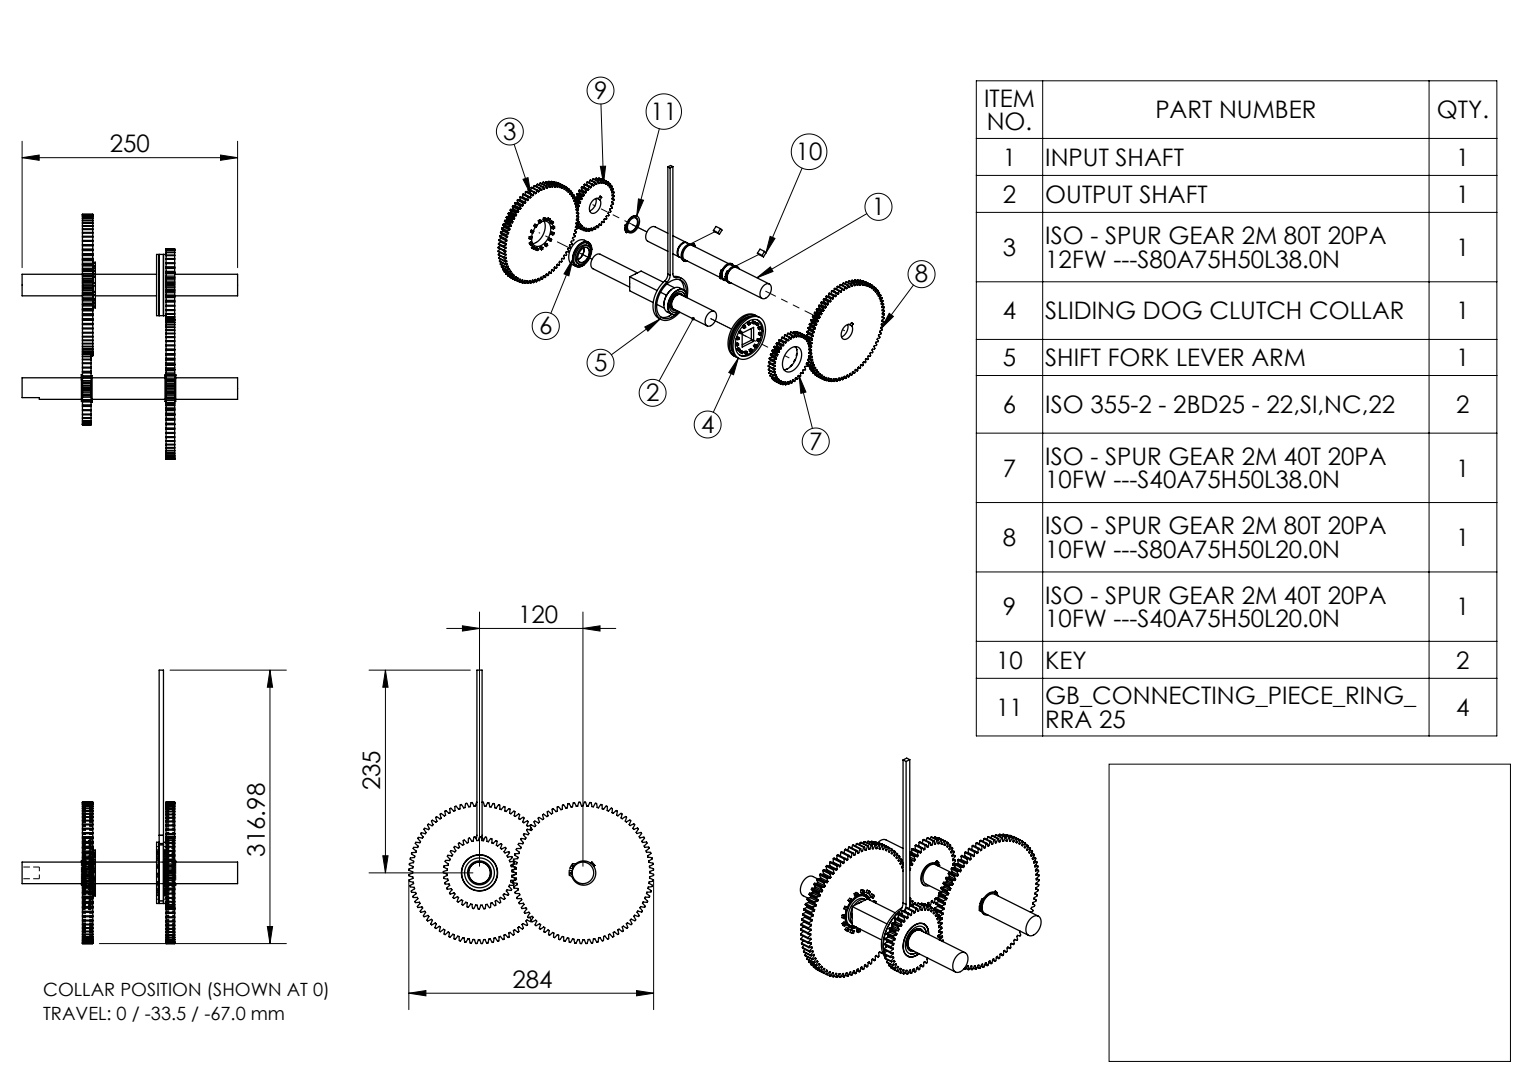
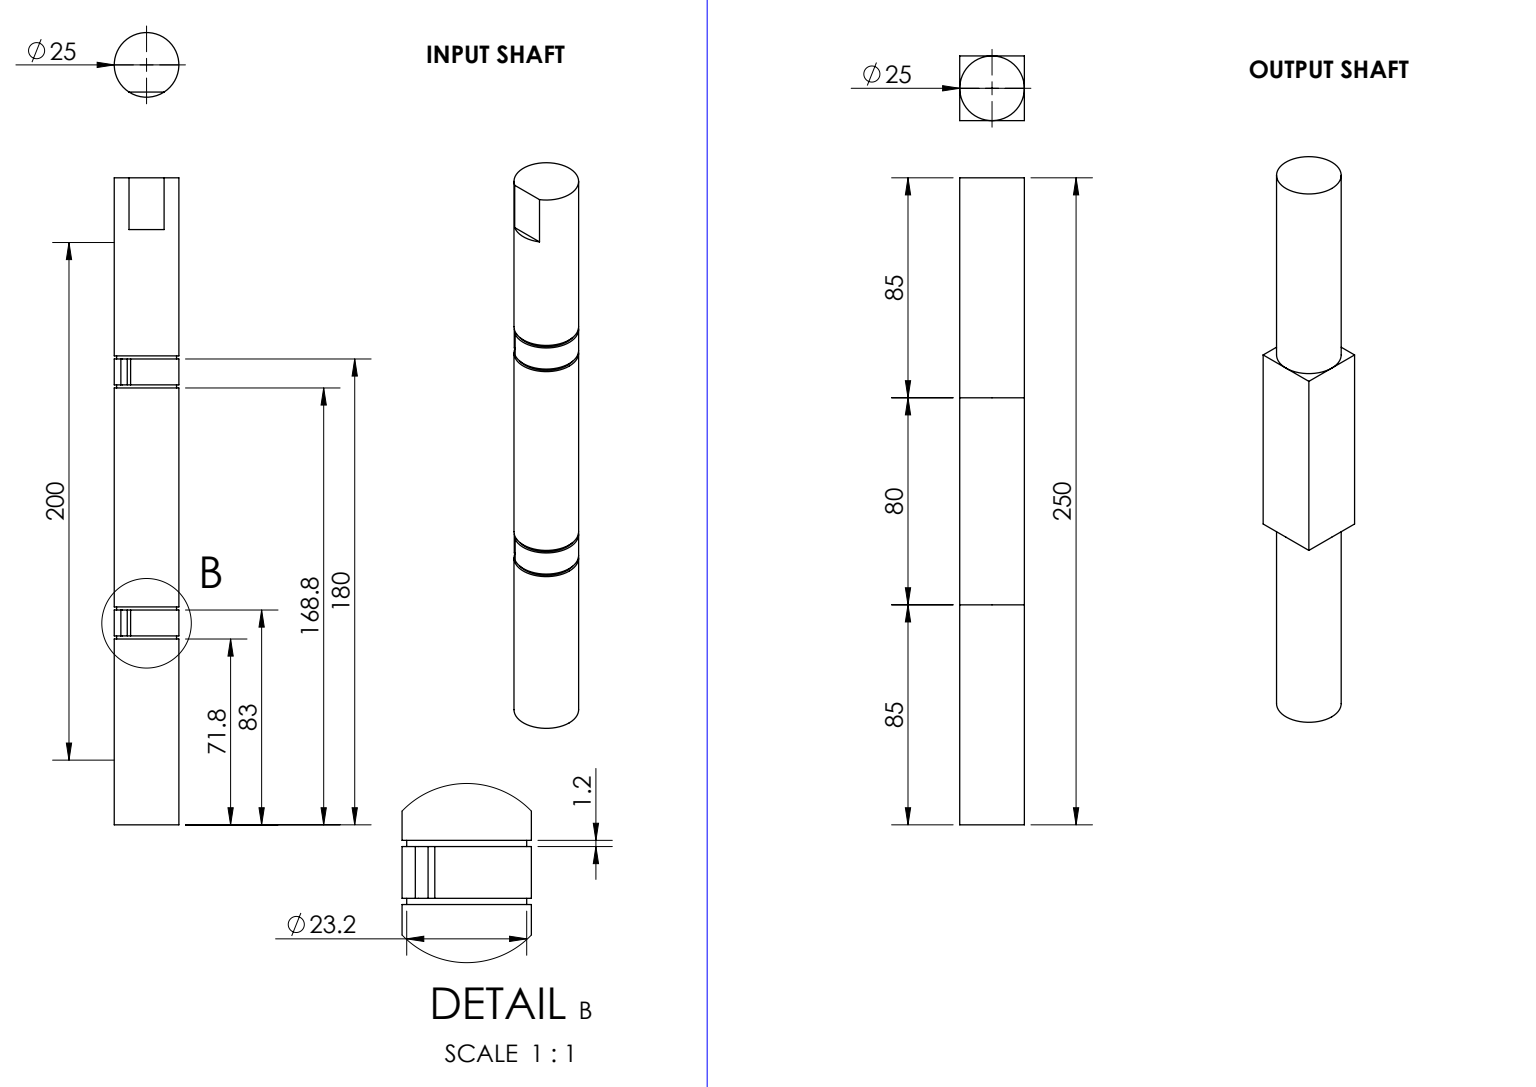
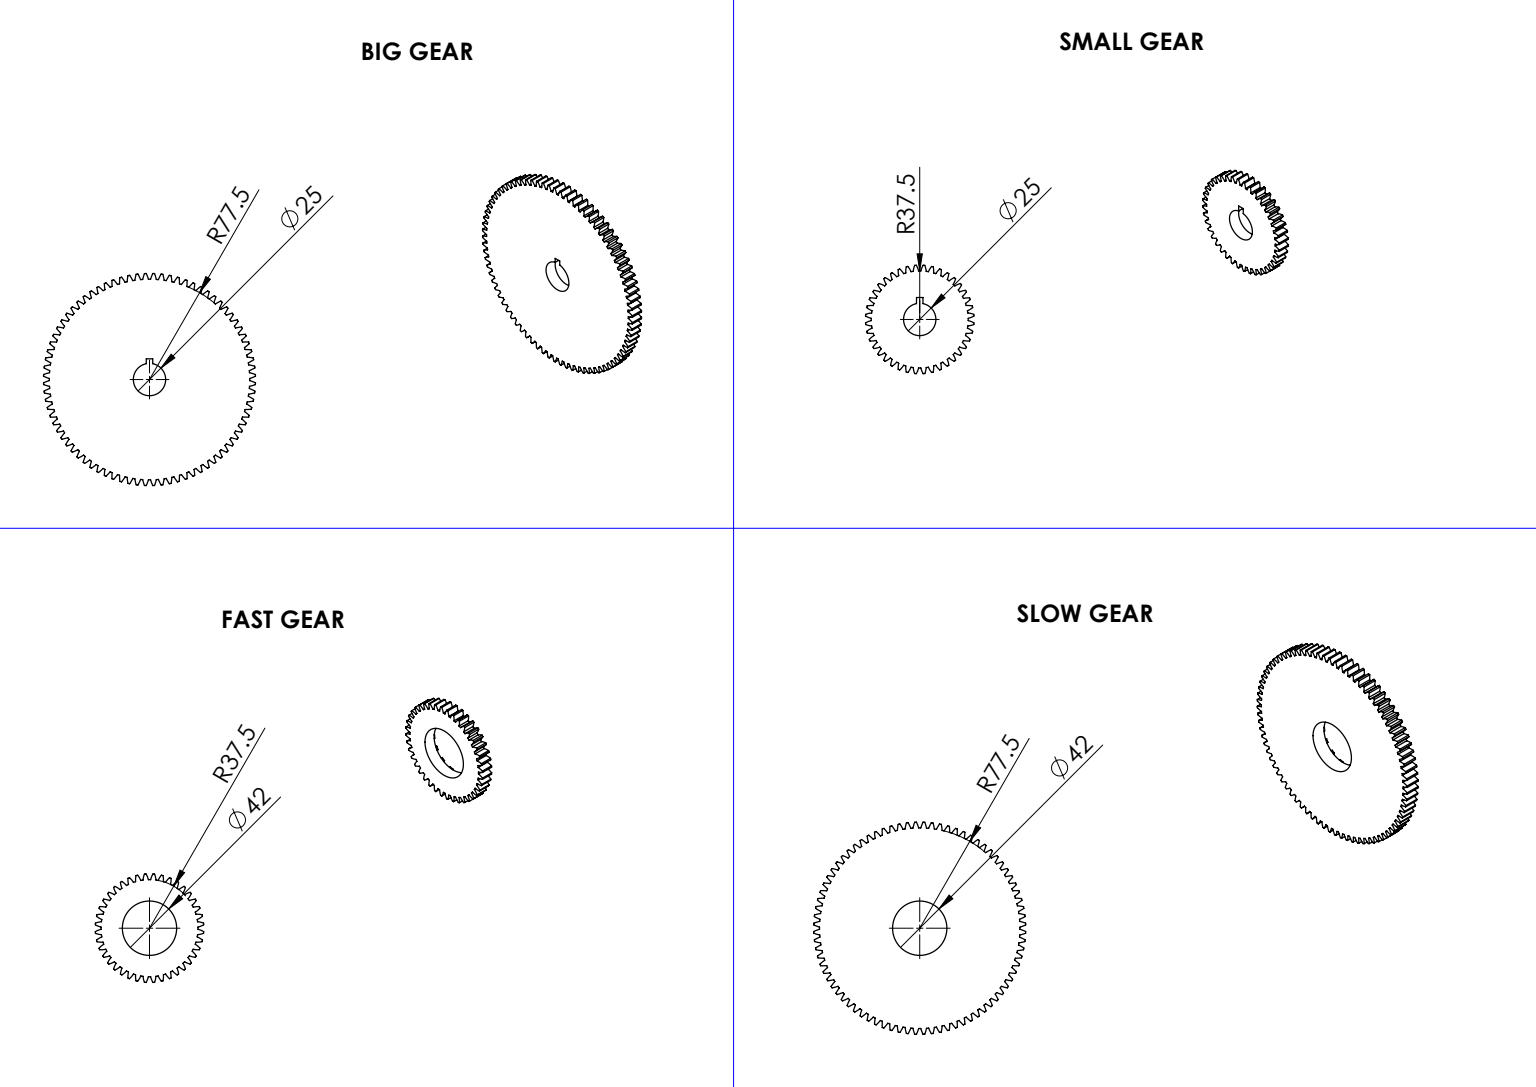
ISO-10303-21;
HEADER;
FILE_DESCRIPTION (('STEP AP214'),
    '1' );
FILE_NAME ('BR-543',
    '2026-09-30T12:41:04',
    ( '' ),
    ( '' ),
    'SwSTEP 2.0',
    'SolidWorks 2026',
    '' );
FILE_SCHEMA (( 'AUTOMOTIVE_DESIGN' ));
ENDSEC;

DATA;
#1 = AXIS2_PLACEMENT_3D ( 'NONE', #4503, #33619, #30682 ) ;
#2 = EDGE_CURVE ( 'NONE', #44254, #29847, #44238, .T. ) ;
#3 = DIRECTION ( 'NONE',  ( -1.000000000000000000, 0.000000000000000000, 0.000000000000000000 ) ) ;
#4 = VECTOR ( 'NONE', #40602, 1000.000000000000000 ) ;
#5 = EDGE_LOOP ( 'NONE', ( #19827, #27831, #3071, #30075 ) ) ;
#6 = ORIENTED_EDGE ( 'NONE', *, *, #30386, .F. ) ;
#7 = CARTESIAN_POINT ( 'NONE',  ( 0.000000000000000000, -15.33399622253423722, -80.55351364060604169 ) ) ;
#8 = ORIENTED_EDGE ( 'NONE', *, *, #47564, .F. ) ;
#9 = CARTESIAN_POINT ( 'NONE',  ( 0.000000000000000000, -120.0000000000000000, -5.500000000000000000 ) ) ;
#10 = DIRECTION ( 'NONE',  ( 1.000000000000000000, 0.000000000000000000, 0.000000000000000000 ) ) ;
#11 = ORIENTED_EDGE ( 'NONE', *, *, #30239, .T. ) ;
#12 = ORIENTED_EDGE ( 'NONE', *, *, #41227, .F. ) ;
#13 = LINE ( 'NONE', #16590, #37780 ) ;
#14 = CARTESIAN_POINT ( 'NONE',  ( 10.00000000000000000, 68.26794271651262136, 31.47745569255165066 ) ) ;
#15 = ORIENTED_EDGE ( 'NONE', *, *, #7786, .T. ) ;
#16 = ADVANCED_FACE ( 'NONE', ( #23120 ), #30468, .T. ) ;
#18 = VERTEX_POINT ( 'NONE', #22403 ) ;
#17 = DIRECTION ( 'NONE',  ( 0.000000000000000000, 0.000000000000000000, 1.000000000000000000 ) ) ;
#19 = CARTESIAN_POINT ( 'NONE',  ( 0.000000000000000000, 44.99326035066052043, 68.55367621811159040 ) ) ;
#20 = VERTEX_POINT ( 'NONE', #356 ) ;
#21 = CARTESIAN_POINT ( 'NONE',  ( 11.99999999999999822, 70.53064760720316428, -26.01480285779861035 ) ) ;
#22 = ORIENTED_EDGE ( 'NONE', *, *, #45043, .F. ) ;
#23 = LINE ( 'NONE', #29422, #16608 ) ;
#24 = DIRECTION ( 'NONE',  ( -1.000000000000000000, 0.000000000000000000, -0.000000000000000000 ) ) ;
#25 = ORIENTED_EDGE ( 'NONE', *, *, #6574, .F. ) ;
#26 = DIRECTION ( 'NONE',  ( -1.000000000000000000, -0.000000000000000000, -0.000000000000000000 ) ) ;
#27 = FACE_BOUND ( 'NONE', #47699, .T. ) ;
#28 = DIRECTION ( 'NONE',  ( 0.000000000000000000, 0.000000000000000000, 1.000000000000000000 ) ) ;
#29 = CARTESIAN_POINT ( 'NONE',  ( 10.00000000000000000, 31.46837873494978055, 68.27212725128286763 ) ) ;
#30 = DIRECTION ( 'NONE',  ( -0.6516173805718067369, 0.7585478161175716050, 0.000000000000000000 ) ) ;
#32 = AXIS2_PLACEMENT_3D ( 'NONE', #39036, #42465, #12856 ) ;
#31 = DIRECTION ( 'NONE',  ( 1.000000000000000000, 0.000000000000000000, -0.000000000000000000 ) ) ;
#33 = VECTOR ( 'NONE', #5683, 1000.000000000000000 ) ;
#34 = DIRECTION ( 'NONE',  ( -1.000000000000000000, 0.000000000000000000, 0.000000000000000000 ) ) ;
#35 = CARTESIAN_POINT ( 'NONE',  ( 10.00000000000000000, 0.000000000000000000, 0.000000000000000000 ) ) ;
#36 = FACE_OUTER_BOUND ( 'NONE', #8537, .T. ) ;
#37 = DIRECTION ( 'NONE',  ( -0.000000000000000000, -0.9945218953682741780, 0.1045284632676447834 ) ) ;
#38 = EDGE_CURVE ( 'NONE', #36456, #38853, #23936, .T. ) ;
#39 = AXIS2_PLACEMENT_3D ( 'NONE', #46336, #27993, #5460 ) ;
#40 = AXIS2_PLACEMENT_3D ( 'NONE', #4431, #34260, #12011 ) ;
#41 = ADVANCED_FACE ( 'NONE', ( #48333 ), #4038, .T. ) ;
#42 = DIRECTION ( 'NONE',  ( -1.000000000000000000, -0.000000000000000000, -0.000000000000000000 ) ) ;
#43 = DIRECTION ( 'NONE',  ( -1.000000000000000000, -0.000000000000000000, -0.000000000000000000 ) ) ;
#44 = CARTESIAN_POINT ( 'NONE',  ( 0.000000000000000000, 73.44644590900061587, 24.73286445877730699 ) ) ;
#45 = CARTESIAN_POINT ( 'NONE',  ( 0.000000000000000000, 0.000000000000000000, 0.000000000000000000 ) ) ;
#46 = EDGE_CURVE ( 'NONE', #39583, #27608, #108, .T. ) ;
#47 = AXIS2_PLACEMENT_3D ( 'NONE', #3704, #48253, #7378 ) ;
#48 = AXIS2_PLACEMENT_3D ( 'NONE', #27504, #9364, #31182 ) ;
#49 = EDGE_LOOP ( 'NONE', ( #19145, #44753, #19555, #4360 ) ) ;
#50 = DIRECTION ( 'NONE',  ( 0.000000000000000000, -0.4999999999999930611, 0.8660254037844425934 ) ) ;
#51 = VECTOR ( 'NONE', #46939, 1000.000000000000000 ) ;
#52 = ORIENTED_EDGE ( 'NONE', *, *, #13978, .F. ) ;
#53 = ADVANCED_FACE ( 'NONE', ( #40751 ), #41250, .T. ) ;
#54 = DIRECTION ( 'NONE',  ( -1.000000000000000000, -0.000000000000000000, -0.000000000000000000 ) ) ;
#55 = CARTESIAN_POINT ( 'NONE',  ( -0.09991859744143775923, 0.8239637576285355758, -54.99999999999998579 ) ) ;
#56 = PLANE ( 'NONE',  #43244 ) ;
#57 = ORIENTED_EDGE ( 'NONE', *, *, #193, .F. ) ;
#58 = DIRECTION ( 'NONE',  ( -1.000000000000000000, -0.000000000000000000, 0.000000000000000000 ) ) ;
#59 = VERTEX_POINT ( 'NONE', #33639 ) ;
#60 = ORIENTED_EDGE ( 'NONE', *, *, #2903, .T. ) ;
#61 = VECTOR ( 'NONE', #12342, 1000.000000000000114 ) ;
#62 = EDGE_CURVE ( 'NONE', #675, #34767, #3595, .T. ) ;
#63 = CARTESIAN_POINT ( 'NONE',  ( -1.895993822078342774E-14, 1.063390998062931622E-14, -55.00000000000000000 ) ) ;
#64 = AXIS2_PLACEMENT_3D ( 'NONE', #6293, #21927, #48124 ) ;
#65 = DIRECTION ( 'NONE',  ( 0.000000000000000000, 1.000000000000000000, 0.000000000000000000 ) ) ;
#67 = ORIENTED_EDGE ( 'NONE', *, *, #48394, .T. ) ;
#66 = DIRECTION ( 'NONE',  ( -0.000000000000000000, -0.000000000000000000, -1.000000000000000000 ) ) ;
#68 = CIRCLE ( 'NONE', #32916, 31.99999999999998224 ) ;
#69 = CIRCLE ( 'NONE', #28969, 16.00000000000000000 ) ;
#70 = EDGE_LOOP ( 'NONE', ( #7032, #13998, #28047, #46307 ) ) ;
#71 = EDGE_LOOP ( 'NONE', ( #28920, #38356, #28549, #18145 ) ) ;
#72 = VECTOR ( 'NONE', #4615, 1000.000000000000000 ) ;
#73 = FACE_OUTER_BOUND ( 'NONE', #11350, .T. ) ;
#74 = CARTESIAN_POINT ( 'NONE',  ( 0.000000000000000000, -132.5000000000000000, -40.00000000000000711 ) ) ;
#75 = AXIS2_PLACEMENT_3D ( 'NONE', #43340, #46778, #40148 ) ;
#76 = CARTESIAN_POINT ( 'NONE',  ( 11.99999999999999822, -79.10210256391353312, -21.60688246758669706 ) ) ;
#77 = EDGE_CURVE ( 'NONE', #36483, #38214, #37203, .T. ) ;
#79 = ORIENTED_EDGE ( 'NONE', *, *, #47708, .T. ) ;
#78 = CYLINDRICAL_SURFACE ( 'NONE', #28876, 31.99999999999999289 ) ;
#80 = ORIENTED_EDGE ( 'NONE', *, *, #29393, .F. ) ;
#81 = CIRCLE ( 'NONE', #41433, 15.99999999999999822 ) ;
#82 = LINE ( 'NONE', #3762, #40454 ) ;
#83 = ORIENTED_EDGE ( 'NONE', *, *, #8742, .F. ) ;
#84 = ORIENTED_EDGE ( 'NONE', *, *, #45252, .T. ) ;
#85 = DIRECTION ( 'NONE',  ( -1.000000000000000000, 0.000000000000000000, 0.000000000000000000 ) ) ;
#86 = DIRECTION ( 'NONE',  ( 0.000000000000000000, -0.9510565162951500895, -0.3090169943749581649 ) ) ;
#87 = CARTESIAN_POINT ( 'NONE',  ( 10.00000000000000000, 40.68715046381928602, 10.41901085202092503 ) ) ;
#88 = DIRECTION ( 'NONE',  ( 0.000000000000000000, 0.000000000000000000, 1.000000000000000000 ) ) ;
#89 = ORIENTED_EDGE ( 'NONE', *, *, #44736, .T. ) ;
#90 = CARTESIAN_POINT ( 'NONE',  ( 50.00005079999999680, 12.24744871391589207, 2.500000000000000000 ) ) ;
#91 = CARTESIAN_POINT ( 'NONE',  ( 10.00000000000000000, -77.49459641780886443, 0.8261519478428377417 ) ) ;
#92 = DIRECTION ( 'NONE',  ( 0.000000000000000000, 0.000000000000000000, 1.000000000000000000 ) ) ;
#93 = DIRECTION ( 'NONE',  ( 0.000000000000000000, -0.8660254037844427044, 0.4999999999999929501 ) ) ;
#94 = DIRECTION ( 'NONE',  ( 0.000000000000000000, 0.7071067811865436870, 0.7071067811865512365 ) ) ;
#95 = DIRECTION ( 'NONE',  ( 1.000000000000000000, -0.000000000000000000, -0.000000000000000000 ) ) ;
#96 = LINE ( 'NONE', #11386, #41562 ) ;
#97 = FACE_OUTER_BOUND ( 'NONE', #38480, .T. ) ;
#98 = EDGE_CURVE ( 'NONE', #12600, #11050, #41482, .T. ) ;
#99 = CARTESIAN_POINT ( 'NONE',  ( 10.00000000000000000, 66.50666863322000211, 39.78640506895629869 ) ) ;
#100 = DIRECTION ( 'NONE',  ( 0.000000000000000000, 0.000000000000000000, 1.000000000000000000 ) ) ;
#101 = EDGE_CURVE ( 'NONE', #47663, #34988, #41134, .T. ) ;
#102 = CARTESIAN_POINT ( 'NONE',  ( 0.000000000000000000, -35.38097989696503021, -12.42422080174676147 ) ) ;
#103 = AXIS2_PLACEMENT_3D ( 'NONE', #39241, #24552, #10332 ) ;
#104 = ORIENTED_EDGE ( 'NONE', *, *, #8668, .T. ) ;
#105 = DIRECTION ( 'NONE',  ( 0.000000000000000000, 0.000000000000000000, -1.000000000000000000 ) ) ;
#106 = CARTESIAN_POINT ( 'NONE',  ( 5.000000000000000000, -21.40280677340398086, 36.13751322684410638 ) ) ;
#107 = AXIS2_PLACEMENT_3D ( 'NONE', #4062, #37590, #7958 ) ;
#108 = LINE ( 'NONE', #14814, #16119 ) ;
#109 = EDGE_CURVE ( 'NONE', #16565, #7964, #26553, .T. ) ;
#110 = FACE_OUTER_BOUND ( 'NONE', #38176, .T. ) ;
#111 = AXIS2_PLACEMENT_3D ( 'NONE', #11902, #26827, #41763 ) ;
#112 = AXIS2_PLACEMENT_3D ( 'NONE', #19745, #19502, #42285 ) ;
#113 = EDGE_CURVE ( 'NONE', #23918, #3261, #44911, .T. ) ;
#114 = CARTESIAN_POINT ( 'NONE',  ( 10.00000000000000000, -75.11764819372145041, 29.05362095685286761 ) ) ;
#115 = CIRCLE ( 'NONE', #9512, 12.49999999999999645 ) ;
#116 = ORIENTED_EDGE ( 'NONE', *, *, #2991, .T. ) ;
#117 = AXIS2_PLACEMENT_3D ( 'NONE', #11604, #8408, #37057 ) ;
#118 = CIRCLE ( 'NONE', #32928, 31.99999999999998224 ) ;
#119 = CARTESIAN_POINT ( 'NONE',  ( 15.00000000000000000, -22.67460108101782978, -6.353146135317906840 ) ) ;
#120 = ORIENTED_EDGE ( 'NONE', *, *, #24250, .F. ) ;
#121 = ADVANCED_FACE ( 'NONE', ( #18943 ), #45382, .T. ) ;
#122 = CARTESIAN_POINT ( 'NONE',  ( 23.49916127795269460, -121.5130826919798039, -5.500000000000000000 ) ) ;
#123 = CARTESIAN_POINT ( 'NONE',  ( 5.999999999999999112, 56.15606465354958488, 59.75363087400094741 ) ) ;
#124 = CARTESIAN_POINT ( 'NONE',  ( 0.000000000000000000, 0.000000000000000000, 0.000000000000000000 ) ) ;
#125 = ORIENTED_EDGE ( 'NONE', *, *, #42452, .T. ) ;
#126 = CARTESIAN_POINT ( 'NONE',  ( 0.000000000000000000, 0.000000000000000000, 0.000000000000000000 ) ) ;
#127 = VERTEX_POINT ( 'NONE', #19425 ) ;
#128 = ORIENTED_EDGE ( 'NONE', *, *, #23966, .T. ) ;
#129 = DIRECTION ( 'NONE',  ( 0.000000000000000000, 0.000000000000000000, 1.000000000000000000 ) ) ;
#130 = CYLINDRICAL_SURFACE ( 'NONE', #29804, 16.00000000000000000 ) ;
#131 = CIRCLE ( 'NONE', #25925, 31.99999999999998934 ) ;
#132 = PLANE ( 'NONE',  #10280 ) ;
#134 = ORIENTED_EDGE ( 'NONE', *, *, #17388, .T. ) ;
#133 = AXIS2_PLACEMENT_3D ( 'NONE', #22370, #41687, #26758 ) ;
#135 = ORIENTED_EDGE ( 'NONE', *, *, #5274, .F. ) ;
#136 = CARTESIAN_POINT ( 'NONE',  ( 11.99999999999999822, 0.000000000000000000, 0.000000000000000000 ) ) ;
#137 = ORIENTED_EDGE ( 'NONE', *, *, #38242, .F. ) ;
#138 = CIRCLE ( 'NONE', #1733, 82.00000000000000000 ) ;
#139 = DIRECTION ( 'NONE',  ( -1.000000000000000000, 0.000000000000000000, 0.000000000000000000 ) ) ;
#140 = EDGE_CURVE ( 'NONE', #28665, #44874, #33290, .T. ) ;
#141 = CARTESIAN_POINT ( 'NONE',  ( 0.000000000000000000, -37.16516213103273714, -4.992566952385376844 ) ) ;
#142 = CARTESIAN_POINT ( 'NONE',  ( 10.00000000000000000, 9.188173127307898369, -40.98264845739739570 ) ) ;
#143 = CARTESIAN_POINT ( 'NONE',  ( 11.99999999999999822, 0.000000000000000000, 0.000000000000000000 ) ) ;
#144 = DIRECTION ( 'NONE',  ( -1.000000000000000000, -0.000000000000000000, -0.000000000000000000 ) ) ;
#145 = CARTESIAN_POINT ( 'NONE',  ( 0.000000000000000000, -27.13269053701078448, -25.88420570971428702 ) ) ;
#146 = EDGE_CURVE ( 'NONE', #7626, #23140, #26277, .T. ) ;
#147 = VECTOR ( 'NONE', #27818, 1000.000000000000000 ) ;
#148 = CARTESIAN_POINT ( 'NONE',  ( -12.49999999999999645, 0.000000000000000000, 125.0000000000000000 ) ) ;
#149 = ORIENTED_EDGE ( 'NONE', *, *, #40004, .F. ) ;
#150 = LINE ( 'NONE', #15351, #37624 ) ;
#151 = DIRECTION ( 'NONE',  ( 0.000000000000000000, 0.000000000000000000, -1.000000000000000000 ) ) ;
#152 = ORIENTED_EDGE ( 'NONE', *, *, #45219, .T. ) ;
#153 = CARTESIAN_POINT ( 'NONE',  ( 10.00000000000000000, 69.42325613327439271, 34.44570377933623462 ) ) ;
#154 = ORIENTED_EDGE ( 'NONE', *, *, #22343, .F. ) ;
#155 = DIRECTION ( 'NONE',  ( 0.000000000000000000, -0.9876883405951359940, -0.1564344650402420545 ) ) ;
#156 = EDGE_LOOP ( 'NONE', ( #423, #28551, #31287, #3442 ) ) ;
#157 = PLANE ( 'NONE',  #35526 ) ;
#158 = LINE ( 'NONE', #18756, #11859 ) ;
#159 = DIRECTION ( 'NONE',  ( 0.000000000000000000, 0.000000000000000000, 1.000000000000000000 ) ) ;
#160 = EDGE_CURVE ( 'NONE', #47761, #19570, #831, .T. ) ;
#161 = ADVANCED_FACE ( 'NONE', ( #29498 ), #7218, .T. ) ;
#162 = EDGE_CURVE ( 'NONE', #27382, #12203, #17667, .T. ) ;
#163 = LINE ( 'NONE', #8479, #41980 ) ;
#164 = DIRECTION ( 'NONE',  ( -0.9966891607226785466, -0.08130631524010122069, 0.000000000000000000 ) ) ;
#165 = CARTESIAN_POINT ( 'NONE',  ( 9.984461079971730157, -95.40710393340120277, 5.500000000000000000 ) ) ;
#166 = DIRECTION ( 'NONE',  ( 0.000000000000000000, 0.000000000000000000, -1.000000000000000000 ) ) ;
#167 = ORIENTED_EDGE ( 'NONE', *, *, #8723, .T. ) ;
#168 = AXIS2_PLACEMENT_3D ( 'NONE', #35916, #17077, #34956 ) ;
#169 = DIRECTION ( 'NONE',  ( 1.000000000000000000, 0.000000000000000000, 0.000000000000000000 ) ) ;
#170 = EDGE_CURVE ( 'NONE', #39780, #42290, #34086, .T. ) ;
#171 = LINE ( 'NONE', #44725, #4221 ) ;
#172 = ORIENTED_EDGE ( 'NONE', *, *, #6354, .T. ) ;
#173 = AXIS2_PLACEMENT_3D ( 'NONE', #10404, #35866, #3285 ) ;
#174 = CIRCLE ( 'NONE', #27550, 82.00000000000000000 ) ;
#175 = EDGE_LOOP ( 'NONE', ( #21889, #27226, #23925, #32939 ) ) ;
#176 = CARTESIAN_POINT ( 'NONE',  ( 10.00000000000000000, -37.01155633439053361, -6.555932627142825986 ) ) ;
#177 = CARTESIAN_POINT ( 'NONE',  ( 11.99999999999999822, -46.53671651293991118, 59.03961581697383565 ) ) ;
#178 = EDGE_LOOP ( 'NONE', ( #25337, #24092, #4200, #25066 ) ) ;
#179 = VECTOR ( 'NONE', #33994, 1000.000000000000227 ) ;
#180 = DIRECTION ( 'NONE',  ( 0.000000000000000000, 0.000000000000000000, 1.000000000000000000 ) ) ;
#181 = ORIENTED_EDGE ( 'NONE', *, *, #17068, .F. ) ;
#182 = EDGE_LOOP ( 'NONE', ( #38740, #26443, #686, #38124 ) ) ;
#183 = DIRECTION ( 'NONE',  ( -1.000000000000000000, 0.000000000000000000, -0.000000000000000000 ) ) ;
#185 = ORIENTED_EDGE ( 'NONE', *, *, #40077, .F. ) ;
#184 = DIRECTION ( 'NONE',  ( -1.000000000000000000, 0.000000000000000000, 0.000000000000000000 ) ) ;
#186 = CARTESIAN_POINT ( 'NONE',  ( -3.000000000000000000, 22.07842321921481243, 8.187992925817422218 ) ) ;
#187 = EDGE_CURVE ( 'NONE', #17280, #1537, #37135, .T. ) ;
#188 = VERTEX_POINT ( 'NONE', #17657 ) ;
#189 = DIRECTION ( 'NONE',  ( -1.000000000000000000, 0.000000000000000000, 0.000000000000000000 ) ) ;
#190 = ORIENTED_EDGE ( 'NONE', *, *, #24530, .T. ) ;
#191 = CARTESIAN_POINT ( 'NONE',  ( -3.000000000000000000, 8.688484142254221609, -21.88630264137359660 ) ) ;
#192 = CIRCLE ( 'NONE', #29910, 31.99999999999999645 ) ;
#193 = EDGE_CURVE ( 'NONE', #40856, #22912, #44332, .T. ) ;
#194 = FACE_OUTER_BOUND ( 'NONE', #46071, .T. ) ;
#195 = AXIS2_PLACEMENT_3D ( 'NONE', #12772, #42643, #24265 ) ;
#196 = LINE ( 'NONE', #26891, #33016 ) ;
#197 = EDGE_CURVE ( 'NONE', #46520, #36004, #14581, .T. ) ;
#198 = EDGE_LOOP ( 'NONE', ( #6220, #43941, #13520, #1756 ) ) ;
#199 = VERTEX_POINT ( 'NONE', #18124 ) ;
#200 = AXIS2_PLACEMENT_3D ( 'NONE', #41654, #37008, #21837 ) ;
#201 = PRESENTATION_STYLE_ASSIGNMENT (( #44758 ) ) ;
#202 = DIRECTION ( 'NONE',  ( -1.000000000000000000, 0.000000000000000000, 0.000000000000000000 ) ) ;
#203 = ORIENTED_EDGE ( 'NONE', *, *, #19001, .T. ) ;
#204 = ORIENTED_EDGE ( 'NONE', *, *, #32028, .T. ) ;
#205 = CARTESIAN_POINT ( 'NONE',  ( 10.00000000000000000, 73.44644590900061587, 24.73286445877730699 ) ) ;
#206 = ORIENTED_EDGE ( 'NONE', *, *, #20064, .T. ) ;
#207 = AXIS2_PLACEMENT_3D ( 'NONE', #33978, #19292, #34217 ) ;
#208 = FACE_OUTER_BOUND ( 'NONE', #42941, .T. ) ;
#209 = DIRECTION ( 'NONE',  ( 1.000000000000000000, 0.000000000000000000, 0.000000000000000000 ) ) ;
#210 = DIRECTION ( 'NONE',  ( 0.000000000000000000, 0.000000000000000000, 1.000000000000000000 ) ) ;
#211 = CARTESIAN_POINT ( 'NONE',  ( 21.85433023846371370, -135.0628101570779620, 5.500000000000000000 ) ) ;
#212 = CARTESIAN_POINT ( 'NONE',  ( 0.4301293587033142574, -121.4370068666438556, 2.500000000000000000 ) ) ;
#213 = LINE ( 'NONE', #34466, #35925 ) ;
#214 = AXIS2_PLACEMENT_3D ( 'NONE', #47187, #31809, #24426 ) ;
#215 = ADVANCED_FACE ( 'NONE', ( #21326 ), #36975, .T. ) ;
#216 = CARTESIAN_POINT ( 'NONE',  ( 0.000000000000000000, 66.50666863322000211, 39.78640506895629159 ) ) ;
#217 = CARTESIAN_POINT ( 'NONE',  ( 5.000000000000000000, -77.16300072079641836, -27.74655509720751567 ) ) ;
#218 = DIRECTION ( 'NONE',  ( 1.000000000000000000, -0.000000000000000000, 0.000000000000000000 ) ) ;
#219 = AXIS2_PLACEMENT_3D ( 'NONE', #16274, #42449, #45632 ) ;
#220 = CYLINDRICAL_SURFACE ( 'NONE', #39354, 42.00000000000000000 ) ;
#221 = DIRECTION ( 'NONE',  ( -1.000000000000000000, 0.000000000000000000, 0.000000000000000000 ) ) ;
#222 = CARTESIAN_POINT ( 'NONE',  ( -8.826826895187510402, -94.96827758698185562, 5.500000000000000000 ) ) ;
#223 = ADVANCED_FACE ( 'NONE', ( #47514 ), #10805, .T. ) ;
#224 = EDGE_LOOP ( 'NONE', ( #47074, #36686, #31550, #45019 ) ) ;
#225 = UNCERTAINTY_MEASURE_WITH_UNIT (LENGTH_MEASURE( 1.000000000000000082E-05 ), #18543, 'distance_accuracy_value', 'NONE');
#226 = CARTESIAN_POINT ( 'NONE',  ( 0.000000000000000000, 39.78640506895604290, 66.50666863322015843 ) ) ;
#227 = CYLINDRICAL_SURFACE ( 'NONE', #7289, 31.99999999999999289 ) ;
#228 = VECTOR ( 'NONE', #26678, 1000.000000000000000 ) ;
#229 = LINE ( 'NONE', #34247, #6562 ) ;
#230 = EDGE_LOOP ( 'NONE', ( #30613, #47609, #22194, #5952 ) ) ;
#231 = CIRCLE ( 'NONE', #23691, 31.99999999999998934 ) ;
#232 = FACE_OUTER_BOUND ( 'NONE', #26033, .T. ) ;
#233 = CIRCLE ( 'NONE', #34611, 32.00000000000000000 ) ;
#234 = AXIS2_PLACEMENT_3D ( 'NONE', #44816, #29883, #40658 ) ;
#235 = EDGE_LOOP ( 'NONE', ( #42907, #14172, #33989, #24634 ) ) ;
#236 = AXIS2_PLACEMENT_3D ( 'NONE', #34388, #44950, #7968 ) ;
#237 = ORIENTED_EDGE ( 'NONE', *, *, #11573, .F. ) ;
#238 = ORIENTED_EDGE ( 'NONE', *, *, #33137, .T. ) ;
#239 = VERTEX_POINT ( 'NONE', #25711 ) ;
#240 = CARTESIAN_POINT ( 'NONE',  ( -10.00000000000000000, 0.000000000000000000, 0.000000000000000000 ) ) ;
#241 = CIRCLE ( 'NONE', #16690, 77.49900000000000944 ) ;
#242 = CARTESIAN_POINT ( 'NONE',  ( 11.99999999999999822, -72.35432306680469594, -20.40083707022958848 ) ) ;
#243 = EDGE_CURVE ( 'NONE', #41330, #45432, #37225, .T. ) ;
#244 = VECTOR ( 'NONE', #1818, 1000.000000000000114 ) ;
#245 = AXIS2_PLACEMENT_3D ( 'NONE', #38051, #45152, #27276 ) ;
#246 = ORIENTED_EDGE ( 'NONE', *, *, #42379, .F. ) ;
#247 = ORIENTED_EDGE ( 'NONE', *, *, #3753, .T. ) ;
#248 = CARTESIAN_POINT ( 'NONE',  ( 0.000000000000000000, -17.80606268964563554, 33.00180498840040855 ) ) ;
#249 = AXIS2_PLACEMENT_3D ( 'NONE', #38479, #7888, #30651 ) ;
#250 = EDGE_LOOP ( 'NONE', ( #16090, #5934 ) ) ;
#251 = EDGE_CURVE ( 'NONE', #37160, #31484, #24741, .T. ) ;
#252 = CARTESIAN_POINT ( 'NONE',  ( 15.00000000000000000, -18.13022148937242761, 15.02647892043569122 ) ) ;
#253 = CARTESIAN_POINT ( 'NONE',  ( 11.99999999999999822, 0.000000000000000000, 0.000000000000000000 ) ) ;
#254 = EDGE_LOOP ( 'NONE', ( #41035, #46518, #11215, #569 ) ) ;
#255 = EDGE_CURVE ( 'NONE', #32703, #15443, #43843, .T. ) ;
#257 = ORIENTED_EDGE ( 'NONE', *, *, #33177, .T. ) ;
#256 = VECTOR ( 'NONE', #6458, 1000.000000000000000 ) ;
#258 = DIRECTION ( 'NONE',  ( -1.000000000000000000, -0.000000000000000000, 0.000000000000000000 ) ) ;
#259 = DIRECTION ( 'NONE',  ( -1.000000000000000000, -0.000000000000000000, -0.000000000000000000 ) ) ;
#260 = ORIENTED_EDGE ( 'NONE', *, *, #36083, .F. ) ;
#261 = DIRECTION ( 'NONE',  ( 1.000000000000000000, 0.000000000000000000, 0.000000000000000000 ) ) ;
#262 = FACE_OUTER_BOUND ( 'NONE', #8926, .T. ) ;
#263 = ORIENTED_EDGE ( 'NONE', *, *, #42270, .F. ) ;
#264 = CARTESIAN_POINT ( 'NONE',  ( 10.00000000000000000, 51.03279382321166224, -55.19960302592011914 ) ) ;
#265 = ORIENTED_EDGE ( 'NONE', *, *, #11352, .T. ) ;
#266 = EDGE_LOOP ( 'NONE', ( #6, #16108, #6404, #41831 ) ) ;
#267 = CARTESIAN_POINT ( 'NONE',  ( 10.00000000000000000, -39.04073710021356192, 15.48615015657568250 ) ) ;
#268 = CYLINDRICAL_SURFACE ( 'NONE', #17660, 42.00000000000000000 ) ;
#269 = EDGE_CURVE ( 'NONE', #2093, #2200, #29638, .T. ) ;
#270 = VERTEX_POINT ( 'NONE', #3695 ) ;
#271 = CARTESIAN_POINT ( 'NONE',  ( 0.000000000000000000, 0.000000000000000000, 0.000000000000000000 ) ) ;
#272 = DIRECTION ( 'NONE',  ( -1.000000000000000000, 0.000000000000000000, 0.000000000000000000 ) ) ;
#273 = DIRECTION ( 'NONE',  ( -0.6064928550163533050, -0.7950889364178781449, 0.000000000000000000 ) ) ;
#274 = CYLINDRICAL_SURFACE ( 'NONE', #40603, 1.000000000000000888 ) ;
#275 = ADVANCED_FACE ( 'NONE', ( #40907 ), #7371, .T. ) ;
#276 = DIRECTION ( 'NONE',  ( 0.000000000000000000, -1.301042606982602560E-15, 1.000000000000000000 ) ) ;
#277 = ADVANCED_FACE ( 'NONE', ( #13989 ), #2725, .T. ) ;
#278 = CIRCLE ( 'NONE', #3373, 13.90444123027096879 ) ;
#279 = CARTESIAN_POINT ( 'NONE',  ( 10.00000000000000000, -26.79245525562738095, 32.34446384429961796 ) ) ;
#280 = CARTESIAN_POINT ( 'NONE',  ( 0.000000000000000000, 55.38113227695782115, 54.21277698773695164 ) ) ;
#281 = EDGE_CURVE ( 'NONE', #11209, #5995, #44811, .T. ) ;
#282 = DIRECTION ( 'NONE',  ( -1.000000000000000000, -0.000000000000000000, 0.000000000000000000 ) ) ;
#283 = DIRECTION ( 'NONE',  ( -0.3853207896976533764, 0.9227826878668546895, 0.000000000000000000 ) ) ;
#284 = CARTESIAN_POINT ( 'NONE',  ( 8.452893869119503023, -12.51233732111638375, -1.199999999999999956 ) ) ;
#285 = VECTOR ( 'NONE', #16064, 1000.000000000000114 ) ;
#286 = CIRCLE ( 'NONE', #18276, 31.99999999999998934 ) ;
#287 = AXIS2_PLACEMENT_3D ( 'NONE', #20110, #9559, #24504 ) ;
#288 = DIRECTION ( 'NONE',  ( 0.000000000000000000, 0.000000000000000000, 1.000000000000000000 ) ) ;
#289 = CARTESIAN_POINT ( 'NONE',  ( 4.250000000000000000, -13.95926121303099343, 0.000000000000000000 ) ) ;
#290 = DIRECTION ( 'NONE',  ( -0.000000000000000000, -0.000000000000000000, -1.000000000000000000 ) ) ;
#291 = DIRECTION ( 'NONE',  ( 0.000000000000000000, 0.8910065241883657894, 0.4539904997395510788 ) ) ;
#292 = ADVANCED_FACE ( 'NONE', ( #26219 ), #25226, .T. ) ;
#293 = VERTEX_POINT ( 'NONE', #36498 ) ;
#295 = CARTESIAN_POINT ( 'NONE',  ( 12.00000000000000000, -22.67460108101782268, -6.353146135317906840 ) ) ;
#294 = AXIS2_PLACEMENT_3D ( 'NONE', #42649, #20350, #47033 ) ;
#296 = VECTOR ( 'NONE', #11332, 1000.000000000000227 ) ;
#297 = ORIENTED_EDGE ( 'NONE', *, *, #34739, .T. ) ;
#298 = VECTOR ( 'NONE', #22798, 1000.000000000000000 ) ;
#299 = CARTESIAN_POINT ( 'NONE',  ( 10.00000000000000000, 0.000000000000000000, 37.49900000000000233 ) ) ;
#300 = CIRCLE ( 'NONE', #29270, 31.99999999999998934 ) ;
#301 = LINE ( 'NONE', #38005, #1852 ) ;
#302 = CIRCLE ( 'NONE', #25312, 77.49899999999999523 ) ;
#303 = ORIENTED_EDGE ( 'NONE', *, *, #45962, .F. ) ;
#304 = FACE_OUTER_BOUND ( 'NONE', #9767, .T. ) ;
#305 = ORIENTED_EDGE ( 'NONE', *, *, #40170, .F. ) ;
#306 = AXIS2_PLACEMENT_3D ( 'NONE', #44003, #15120, #25632 ) ;
#307 = AXIS2_PLACEMENT_3D ( 'NONE', #36278, #3214, #10821 ) ;
#308 = LINE ( 'NONE', #34316, #47986 ) ;
#309 = DIRECTION ( 'NONE',  ( 0.8774505977381978905, 0.4796670183876304283, 0.000000000000000000 ) ) ;
#310 = AXIS2_PLACEMENT_3D ( 'NONE', #28216, #39492, #24550 ) ;
#312 = ORIENTED_EDGE ( 'NONE', *, *, #16850, .T. ) ;
#311 = CARTESIAN_POINT ( 'NONE',  ( -12.49999999999999822, -120.0000000000000000, 125.0000000000000000 ) ) ;
#313 = CIRCLE ( 'NONE', #39395, 32.00000000000000000 ) ;
#314 = EDGE_LOOP ( 'NONE', ( #30103, #6984, #5328, #6114 ) ) ;
#315 = EDGE_CURVE ( 'NONE', #36078, #25303, #48171, .T. ) ;
#316 = ORIENTED_EDGE ( 'NONE', *, *, #31067, .T. ) ;
#317 = EDGE_CURVE ( 'NONE', #20770, #27040, #8563, .T. ) ;
#318 = EDGE_CURVE ( 'NONE', #41614, #22825, #9882, .T. ) ;
#319 = DIRECTION ( 'NONE',  ( 0.000000000000000000, -1.000000000000000000, -1.047444401652940007E-14 ) ) ;
#320 = CYLINDRICAL_SURFACE ( 'NONE', #47599, 37.49900000000000233 ) ;
#321 = CYLINDRICAL_SURFACE ( 'NONE', #35288, 31.99999999999998579 ) ;
#322 = EDGE_CURVE ( 'NONE', #35660, #31329, #38199, .T. ) ;
#323 = CARTESIAN_POINT ( 'NONE',  ( 11.99999999999999822, -49.70050353004846500, -59.46389618802017907 ) ) ;
#324 = VECTOR ( 'NONE', #48391, 1000.000000000000114 ) ;
#325 = AXIS2_PLACEMENT_3D ( 'NONE', #13479, #5912, #24495 ) ;
#326 = EDGE_LOOP ( 'NONE', ( #36542, #32345 ) ) ;
#327 = CARTESIAN_POINT ( 'NONE',  ( 21.07894319797337701, -103.8699611390234878, 5.500000000000000000 ) ) ;
#328 = ORIENTED_EDGE ( 'NONE', *, *, #15612, .F. ) ;
#329 = ORIENTED_EDGE ( 'NONE', *, *, #30247, .T. ) ;
#330 = EDGE_CURVE ( 'NONE', #44007, #20943, #37237, .T. ) ;
#331 = AXIS2_PLACEMENT_3D ( 'NONE', #33275, #33743, #3658 ) ;
#332 = LINE ( 'NONE', #22378, #45772 ) ;
#333 = AXIS2_PLACEMENT_3D ( 'NONE', #25881, #22476, #15130 ) ;
#334 = LINE ( 'NONE', #7681, #29329 ) ;
#335 = CARTESIAN_POINT ( 'NONE',  ( 10.00000000000000000, 0.000000000000000000, 0.000000000000000000 ) ) ;
#336 = CARTESIAN_POINT ( 'NONE',  ( 0.000000000000000000, 0.000000000000000000, 0.000000000000000000 ) ) ;
#337 = VERTEX_POINT ( 'NONE', #15210 ) ;
#338 = CARTESIAN_POINT ( 'NONE',  ( 5.000000000000002665, -80.28980883073769803, 16.65972982744906261 ) ) ;
#339 = VECTOR ( 'NONE', #11184, 1000.000000000000000 ) ;
#340 = DIRECTION ( 'NONE',  ( -1.000000000000000000, 0.000000000000000000, -0.000000000000000000 ) ) ;
#341 = CARTESIAN_POINT ( 'NONE',  ( 11.99999999999999822, 0.000000000000000000, 0.000000000000000000 ) ) ;
#342 = CARTESIAN_POINT ( 'NONE',  ( -12.50000000000000000, -107.5000000000000000, 2.500000000000000000 ) ) ;
#343 = CYLINDRICAL_SURFACE ( 'NONE', #30928, 31.99999999999998579 ) ;
#344 = DIRECTION ( 'NONE',  ( 0.000000000000000000, -0.1045284632676569680, -0.9945218953682730678 ) ) ;
#345 = ADVANCED_FACE ( 'NONE', ( #515 ), #15447, .T. ) ;
#346 = DIRECTION ( 'NONE',  ( -1.000000000000000000, -0.000000000000000000, 0.000000000000000000 ) ) ;
#347 = CARTESIAN_POINT ( 'NONE',  ( 0.000000000000000000, 68.27212725128275395, -31.46837873495001503 ) ) ;
#348 = DIRECTION ( 'NONE',  ( -1.000000000000000000, 0.000000000000000000, -0.000000000000000000 ) ) ;
#349 = CYLINDRICAL_SURFACE ( 'NONE', #37017, 77.49899999999999523 ) ;
#350 = LINE ( 'NONE', #7467, #9858 ) ;
#351 = EDGE_CURVE ( 'NONE', #24067, #38319, #7847, .T. ) ;
#352 = VERTEX_POINT ( 'NONE', #977 ) ;
#353 = CIRCLE ( 'NONE', #5049, 42.00000000000000000 ) ;
#354 = DIRECTION ( 'NONE',  ( -1.000000000000000000, 0.000000000000000000, 0.000000000000000000 ) ) ;
#355 = DIRECTION ( 'NONE',  ( 0.8541291221503275466, -0.5200609990132993854, 0.000000000000000000 ) ) ;
#356 = CARTESIAN_POINT ( 'NONE',  ( 10.00000000000000000, -41.91543099594816368, -2.663952781846588014 ) ) ;
#357 = AXIS2_PLACEMENT_3D ( 'NONE', #6016, #12869, #17238 ) ;
#358 = CIRCLE ( 'NONE', #28492, 42.00000000000000000 ) ;
#359 = DIRECTION ( 'NONE',  ( -1.000000000000000000, 0.000000000000000000, 0.000000000000000000 ) ) ;
#360 = ORIENTED_EDGE ( 'NONE', *, *, #10558, .T. ) ;
#361 = VERTEX_POINT ( 'NONE', #3941 ) ;
#362 = ADVANCED_FACE ( 'NONE', ( #19342 ), #12497, .T. ) ;
#363 = AXIS2_PLACEMENT_3D ( 'NONE', #3070, #22645, #37583 ) ;
#364 = CIRCLE ( 'NONE', #26154, 16.00000000000000355 ) ;
#365 = EDGE_LOOP ( 'NONE', ( #14092, #42320, #15486, #37127 ) ) ;
#366 = AXIS2_PLACEMENT_3D ( 'NONE', #37130, #40340, #3598 ) ;
#367 = ORIENTED_EDGE ( 'NONE', *, *, #45108, .T. ) ;
#368 = VECTOR ( 'NONE', #28016, 1000.000000000000000 ) ;
#369 = AXIS2_PLACEMENT_3D ( 'NONE', #26235, #32831, #22557 ) ;
#370 = CARTESIAN_POINT ( 'NONE',  ( 12.13205353604972991, -140.1820037904669789, 5.500000000000000000 ) ) ;
#371 = VERTEX_POINT ( 'NONE', #8335 ) ;
#372 = AXIS2_PLACEMENT_3D ( 'NONE', #44697, #34162, #22185 ) ;
#373 = ADVANCED_FACE ( 'NONE', ( #37707 ), #45293, .T. ) ;
#374 = DIRECTION ( 'NONE',  ( -1.000000000000000000, -0.000000000000000000, -0.000000000000000000 ) ) ;
#375 = EDGE_LOOP ( 'NONE', ( #30574, #18631, #26654, #43679 ) ) ;
#376 = EDGE_CURVE ( 'NONE', #24228, #15279, #8089, .T. ) ;
#377 = DIRECTION ( 'NONE',  ( 0.000000000000000000, 0.000000000000000000, 1.000000000000000000 ) ) ;
#378 = DIRECTION ( 'NONE',  ( 0.000000000000000000, -0.8660254037844421493, -0.4999999999999939493 ) ) ;
#379 = ORIENTED_EDGE ( 'NONE', *, *, #23228, .F. ) ;
#380 = CARTESIAN_POINT ( 'NONE',  ( -10.00000000000000000, 0.000000000000000000, 0.000000000000000000 ) ) ;
#381 = ORIENTED_EDGE ( 'NONE', *, *, #30250, .F. ) ;
#382 = EDGE_CURVE ( 'NONE', #975, #23651, #30608, .T. ) ;
#383 = ORIENTED_EDGE ( 'NONE', *, *, #20661, .T. ) ;
#384 = ORIENTED_EDGE ( 'NONE', *, *, #2359, .F. ) ;
#385 = ADVANCED_FACE ( 'NONE', ( #12022 ), #4437, .F. ) ;
#386 = FACE_OUTER_BOUND ( 'NONE', #9470, .T. ) ;
#387 = CARTESIAN_POINT ( 'NONE',  ( 12.00000000000000000, 6.762365576493647445, 25.66652317338391498 ) ) ;
#389 = DIRECTION ( 'NONE',  ( 0.000000000000000000, -0.9510565162951500895, -0.3090169943749581649 ) ) ;
#388 = CIRCLE ( 'NONE', #33997, 31.99999999999998579 ) ;
#390 = VERTEX_POINT ( 'NONE', #37472 ) ;
#391 = ORIENTED_EDGE ( 'NONE', *, *, #18436, .F. ) ;
#392 = ORIENTED_EDGE ( 'NONE', *, *, #17689, .T. ) ;
#393 = DIRECTION ( 'NONE',  ( -1.000000000000000000, 0.000000000000000000, -0.000000000000000000 ) ) ;
#394 = ORIENTED_EDGE ( 'NONE', *, *, #24277, .T. ) ;
#395 = EDGE_CURVE ( 'NONE', #25211, #20236, #36366, .T. ) ;
#396 = DIRECTION ( 'NONE',  ( 0.000000000000000000, 0.000000000000000000, 1.000000000000000000 ) ) ;
#397 = FACE_OUTER_BOUND ( 'NONE', #27506, .T. ) ;
#398 = CARTESIAN_POINT ( 'NONE',  ( 5.000000000000002665, 80.55351364060589958, 15.33399622253511829 ) ) ;
#399 = CARTESIAN_POINT ( 'NONE',  ( 10.00000000000000000, 17.80606268964585226, -33.00180498840028775 ) ) ;
#400 = DIRECTION ( 'NONE',  ( -1.000000000000000000, 0.000000000000000000, -0.000000000000000000 ) ) ;
#401 = DIRECTION ( 'NONE',  ( 0.000000000000000000, 0.9945218953682730678, -0.1045284632676570791 ) ) ;
#402 = DIRECTION ( 'NONE',  ( -1.000000000000000000, 0.000000000000000000, -0.000000000000000000 ) ) ;
#403 = FILL_AREA_STYLE ('',( #33451 ) ) ;
#404 = DIRECTION ( 'NONE',  ( -1.000000000000000000, 0.000000000000000000, 0.000000000000000000 ) ) ;
#405 = ORIENTED_EDGE ( 'NONE', *, *, #13443, .T. ) ;
#406 = CARTESIAN_POINT ( 'NONE',  ( 10.00000000000000000, 0.000000000000000000, 0.000000000000000000 ) ) ;
#407 = CIRCLE ( 'NONE', #6661, 16.00000000000000000 ) ;
#408 = AXIS2_PLACEMENT_3D ( 'NONE', #31501, #26915, #8309 ) ;
#409 = VERTEX_POINT ( 'NONE', #38435 ) ;
#410 = VERTEX_POINT ( 'NONE', #19816 ) ;
#411 = PLANE ( 'NONE',  #16338 ) ;
#412 = VECTOR ( 'NONE', #23395, 1000.000000000000000 ) ;
#413 = DIRECTION ( 'NONE',  ( -5.778480238264233142E-17, 1.000000000000000000, 0.000000000000000000 ) ) ;
#414 = CARTESIAN_POINT ( 'NONE',  ( 0.000000000000000000, -0.8828120875898013420, -37.48860685352291711 ) ) ;
#415 = DIRECTION ( 'NONE',  ( 0.000000000000000000, -0.9723699203976740035, -0.2334453638559161881 ) ) ;
#416 = AXIS2_PLACEMENT_3D ( 'NONE', #18456, #18686, #44643 ) ;
#417 = VECTOR ( 'NONE', #47685, 1000.000000000000000 ) ;
#418 = CARTESIAN_POINT ( 'NONE',  ( 10.00000000000000000, 32.34446384430010113, -26.79245525562679831 ) ) ;
#419 = DIRECTION ( 'NONE',  ( -1.000000000000000000, 0.000000000000000000, 0.000000000000000000 ) ) ;
#420 = AXIS2_PLACEMENT_3D ( 'NONE', #44361, #25025, #2755 ) ;
#421 = CARTESIAN_POINT ( 'NONE',  ( 0.000000000000000000, -37.01155633439053361, -6.555932627142825986 ) ) ;
#422 = LINE ( 'NONE', #22928, #45953 ) ;
#423 = ORIENTED_EDGE ( 'NONE', *, *, #2653, .T. ) ;
#424 = CIRCLE ( 'NONE', #33232, 31.99999999999999289 ) ;
#425 = DIRECTION ( 'NONE',  ( 0.000000000000000000, 0.000000000000000000, 1.000000000000000000 ) ) ;
#426 = CYLINDRICAL_SURFACE ( 'NONE', #16685, 16.00000000000000000 ) ;
#427 = ORIENTED_EDGE ( 'NONE', *, *, #28237, .T. ) ;
#428 = AXIS2_PLACEMENT_3D ( 'NONE', #42188, #26543, #8177 ) ;
#429 = ORIENTED_EDGE ( 'NONE', *, *, #45946, .F. ) ;
#430 = EDGE_LOOP ( 'NONE', ( #22082, #37942, #14548, #45186 ) ) ;
#431 = CARTESIAN_POINT ( 'NONE',  ( 5.000000000000002665, -81.50828551894234408, 8.966570791700407383 ) ) ;
#432 = CARTESIAN_POINT ( 'NONE',  ( 12.00000000000000000, 18.84667830672579925, -18.68964196561269375 ) ) ;
#433 = ORIENTED_EDGE ( 'NONE', *, *, #40581, .T. ) ;
#434 = AXIS2_PLACEMENT_3D ( 'NONE', #9833, #1772, #36012 ) ;
#435 = CIRCLE ( 'NONE', #37935, 16.00000000000000000 ) ;
#436 = EDGE_CURVE ( 'NONE', #26945, #36459, #32495, .T. ) ;
#437 = DIRECTION ( 'NONE',  ( 0.000000000000000000, 0.000000000000000000, 1.000000000000000000 ) ) ;
#438 = ORIENTED_EDGE ( 'NONE', *, *, #14400, .T. ) ;
#439 = EDGE_LOOP ( 'NONE', ( #31934, #23620, #8333, #8403 ) ) ;
#440 = CIRCLE ( 'NONE', #27049, 77.49900000000000944 ) ;
#441 = VERTEX_POINT ( 'NONE', #27431 ) ;
#442 = EDGE_CURVE ( 'NONE', #1544, #24479, #1223, .T. ) ;
#443 = CIRCLE ( 'NONE', #16876, 77.49899999999999523 ) ;
#444 = DIRECTION ( 'NONE',  ( 0.000000000000000000, 0.000000000000000000, 1.000000000000000000 ) ) ;
#445 = ADVANCED_FACE ( 'NONE', ( #22776 ), #33780, .F. ) ;
#447 = ORIENTED_EDGE ( 'NONE', *, *, #24140, .T. ) ;
#446 = CARTESIAN_POINT ( 'NONE',  ( -13.05994868825747446, -139.5943292883446532, 5.500000000000000000 ) ) ;
#448 = DIRECTION ( 'NONE',  ( -0.000000000000000000, -0.000000000000000000, -1.000000000000000000 ) ) ;
#449 = ORIENTED_EDGE ( 'NONE', *, *, #48116, .F. ) ;
#450 = CYLINDRICAL_SURFACE ( 'NONE', #508, 42.00000000000000000 ) ;
#451 = VERTEX_POINT ( 'NONE', #26459 ) ;
#452 = EDGE_LOOP ( 'NONE', ( #39151, #42607, #27629, #45892 ) ) ;
#453 = EDGE_CURVE ( 'NONE', #25264, #47247, #1479, .T. ) ;
#454 = FACE_OUTER_BOUND ( 'NONE', #32688, .T. ) ;
#455 = CIRCLE ( 'NONE', #41872, 77.49899999999999523 ) ;
#456 = EDGE_CURVE ( 'NONE', #8338, #715, #31710, .T. ) ;
#457 = CARTESIAN_POINT ( 'NONE',  ( 0.000000000000000000, 0.000000000000000000, 0.000000000000000000 ) ) ;
#458 = DIRECTION ( 'NONE',  ( 1.000000000000000000, 0.000000000000000000, 0.000000000000000000 ) ) ;
#459 = VECTOR ( 'NONE', #14578, 1000.000000000000114 ) ;
#460 = ORIENTED_EDGE ( 'NONE', *, *, #19536, .T. ) ;
#461 = VERTEX_POINT ( 'NONE', #39664 ) ;
#462 = FACE_OUTER_BOUND ( 'NONE', #2649, .T. ) ;
#463 = VECTOR ( 'NONE', #18147, 1000.000000000000114 ) ;
#464 = FACE_OUTER_BOUND ( 'NONE', #20083, .T. ) ;
#465 = ORIENTED_EDGE ( 'NONE', *, *, #395, .F. ) ;
#466 = ORIENTED_EDGE ( 'NONE', *, *, #39065, .F. ) ;
#467 = LINE ( 'NONE', #3892, #11924 ) ;
#468 = ORIENTED_EDGE ( 'NONE', *, *, #40787, .T. ) ;
#469 = CARTESIAN_POINT ( 'NONE',  ( 0.000000000000000000, 0.000000000000000000, 0.000000000000000000 ) ) ;
#471 = EDGE_CURVE ( 'NONE', #36574, #26337, #5917, .T. ) ;
#470 = DIRECTION ( 'NONE',  ( 1.000000000000000000, -0.000000000000000000, 0.000000000000000000 ) ) ;
#472 = DIRECTION ( 'NONE',  ( 0.000000000000000000, 0.000000000000000000, 1.000000000000000000 ) ) ;
#473 = DIRECTION ( 'NONE',  ( -0.000000000000000000, -0.000000000000000000, -1.000000000000000000 ) ) ;
#474 = ORIENTED_EDGE ( 'NONE', *, *, #31629, .F. ) ;
#475 = DIRECTION ( 'NONE',  ( -0.000000000000000000, 6.938893903907229364E-16, 1.000000000000000000 ) ) ;
#476 = DIRECTION ( 'NONE',  ( -1.000000000000000000, 0.000000000000000000, 0.000000000000000000 ) ) ;
#477 = ADVANCED_FACE ( 'NONE', ( #20544 ), #17119, .F. ) ;
#478 = CARTESIAN_POINT ( 'NONE',  ( 0.000000000000000000, -37.22597642581153821, -5.202137450156795850 ) ) ;
#479 = VECTOR ( 'NONE', #15922, 1000.000000000000000 ) ;
#480 = PLANE ( 'NONE',  #23178 ) ;
#481 = LINE ( 'NONE', #3406, #9026 ) ;
#482 = ORIENTED_EDGE ( 'NONE', *, *, #3297, .T. ) ;
#483 = CARTESIAN_POINT ( 'NONE',  ( 10.00000000000000000, 37.58145647212453611, 0.6853352020791767529 ) ) ;
#484 = CARTESIAN_POINT ( 'NONE',  ( 10.00000000000000000, 0.000000000000000000, 0.000000000000000000 ) ) ;
#485 = FILL_AREA_STYLE ('',( #30352 ) ) ;
#486 = AXIS2_PLACEMENT_3D ( 'NONE', #8349, #993, #38213 ) ;
#487 = LINE ( 'NONE', #45760, #16267 ) ;
#488 = VERTEX_POINT ( 'NONE', #2425 ) ;
#489 = EDGE_CURVE ( 'NONE', #6953, #36450, #38933, .T. ) ;
#490 = AXIS2_PLACEMENT_3D ( 'NONE', #7122, #21805, #36731 ) ;
#491 = CARTESIAN_POINT ( 'NONE',  ( 10.00000000000000000, -33.00180498840035170, -17.80606268964575278 ) ) ;
#492 = ADVANCED_FACE ( 'NONE', ( #9294 ), #21030, .T. ) ;
#493 = VECTOR ( 'NONE', #19133, 1000.000000000000000 ) ;
#494 = LINE ( 'NONE', #44786, #14354 ) ;
#495 = AXIS2_PLACEMENT_3D ( 'NONE', #15450, #22781, #48249 ) ;
#496 = FACE_OUTER_BOUND ( 'NONE', #5249, .T. ) ;
#497 = EDGE_CURVE ( 'NONE', #19153, #6597, #35001, .T. ) ;
#498 = EDGE_LOOP ( 'NONE', ( #18860, #40919, #13713 ) ) ;
#499 = AXIS2_PLACEMENT_3D ( 'NONE', #29602, #44534, #40396 ) ;
#500 = VERTEX_POINT ( 'NONE', #16404 ) ;
#501 = FACE_OUTER_BOUND ( 'NONE', #22747, .T. ) ;
#502 = ORIENTED_EDGE ( 'NONE', *, *, #10661, .T. ) ;
#503 = ORIENTED_EDGE ( 'NONE', *, *, #28074, .T. ) ;
#504 = ORIENTED_EDGE ( 'NONE', *, *, #40543, .F. ) ;
#505 = EDGE_CURVE ( 'NONE', #45334, #15443, #24468, .T. ) ;
#506 = EDGE_CURVE ( 'NONE', #11777, #14224, #24669, .T. ) ;
#507 = EDGE_CURVE ( 'NONE', #9625, #26682, #29342, .T. ) ;
#508 = AXIS2_PLACEMENT_3D ( 'NONE', #33725, #41100, #29346 ) ;
#509 = FACE_OUTER_BOUND ( 'NONE', #15713, .T. ) ;
#510 = ORIENTED_EDGE ( 'NONE', *, *, #9166, .F. ) ;
#511 = ORIENTED_EDGE ( 'NONE', *, *, #46423, .T. ) ;
#512 = CYLINDRICAL_SURFACE ( 'NONE', #29821, 16.00000000000000000 ) ;
#513 = ORIENTED_EDGE ( 'NONE', *, *, #3767, .F. ) ;
#514 = CIRCLE ( 'NONE', #27902, 82.00000000000000000 ) ;
#515 = FACE_OUTER_BOUND ( 'NONE', #30757, .T. ) ;
#516 = CARTESIAN_POINT ( 'NONE',  ( 10.00000000000000000, 0.000000000000000000, 0.000000000000000000 ) ) ;
#517 = ORIENTED_EDGE ( 'NONE', *, *, #27272, .F. ) ;
#518 = CARTESIAN_POINT ( 'NONE',  ( 0.000000000000000000, 0.000000000000000000, 0.000000000000000000 ) ) ;
#519 = ORIENTED_EDGE ( 'NONE', *, *, #3917, .T. ) ;
#520 = EDGE_CURVE ( 'NONE', #45830, #43377, #33250, .T. ) ;
#521 = CARTESIAN_POINT ( 'NONE',  ( 5.000000000000000000, 64.81221759200343513, 50.23322058963371006 ) ) ;
#522 = CYLINDRICAL_SURFACE ( 'NONE', #3979, 16.00000000000000000 ) ;
#523 = ORIENTED_EDGE ( 'NONE', *, *, #34532, .F. ) ;
#524 = AXIS2_PLACEMENT_3D ( 'NONE', #22263, #15169, #37667 ) ;
#525 = DIRECTION ( 'NONE',  ( 0.000000000000000000, 0.4539904997395412534, 0.8910065241883706744 ) ) ;
#526 = VERTEX_POINT ( 'NONE', #2197 ) ;
#527 = ORIENTED_EDGE ( 'NONE', *, *, #14213, .F. ) ;
#528 = CARTESIAN_POINT ( 'NONE',  ( 10.00000000000000000, 0.000000000000000000, 0.000000000000000000 ) ) ;
#529 = LINE ( 'NONE', #8818, #19135 ) ;
#530 = CARTESIAN_POINT ( 'NONE',  ( 12.00000000000000000, -19.89357724625003598, -12.59942793731059041 ) ) ;
#531 = FACE_OUTER_BOUND ( 'NONE', #25724, .T. ) ;
#532 = CARTESIAN_POINT ( 'NONE',  ( 11.99999999999999822, 0.000000000000000000, 0.000000000000000000 ) ) ;
#533 = PRESENTATION_LAYER_ASSIGNMENT (  '', '', ( #26317 ) ) ;
#534 = DIRECTION ( 'NONE',  ( -1.000000000000000000, 0.000000000000000000, 0.000000000000000000 ) ) ;
#535 = CARTESIAN_POINT ( 'NONE',  ( 0.000000000000000000, -65.59268652807183742, -36.72794159290312166 ) ) ;
#536 = CIRCLE ( 'NONE', #37253, 37.49900000000000944 ) ;
#537 = DIRECTION ( 'NONE',  ( -0.9730327541852497042, 0.2306669878475622604, 0.000000000000000000 ) ) ;
#538 = ORIENTED_EDGE ( 'NONE', *, *, #45114, .T. ) ;
#539 = CARTESIAN_POINT ( 'NONE',  ( 0.000000000000000000, -6.555932627142676772, 37.01155633439056203 ) ) ;
#540 = FACE_OUTER_BOUND ( 'NONE', #34689, .T. ) ;
#541 = DIRECTION ( 'NONE',  ( -1.000000000000000000, -0.000000000000000000, 0.000000000000000000 ) ) ;
#542 = DIRECTION ( 'NONE',  ( -0.000000000000000000, -0.000000000000000000, -1.000000000000000000 ) ) ;
#543 = FACE_OUTER_BOUND ( 'NONE', #33687, .T. ) ;
#544 = DIRECTION ( 'NONE',  ( 0.9918136447140100120, -0.1276937514489704939, 0.000000000000000000 ) ) ;
#545 = CARTESIAN_POINT ( 'NONE',  ( -10.00000000000000000, 0.000000000000000000, 0.000000000000000000 ) ) ;
#546 = ORIENTED_EDGE ( 'NONE', *, *, #47429, .F. ) ;
#547 = ORIENTED_EDGE ( 'NONE', *, *, #34805, .F. ) ;
#548 = CIRCLE ( 'NONE', #12256, 20.99999999999999645 ) ;
#549 = EDGE_CURVE ( 'NONE', #46629, #10383, #44192, .T. ) ;
#550 = FACE_BOUND ( 'NONE', #1348, .T. ) ;
#551 = VERTEX_POINT ( 'NONE', #27927 ) ;
#552 = CARTESIAN_POINT ( 'NONE',  ( 10.00000000000000000, 15.48615015657638239, -39.04073710021328480 ) ) ;
#553 = ADVANCED_FACE ( 'NONE', ( #16645 ), #46266, .T. ) ;
#554 = DIRECTION ( 'NONE',  ( -1.000000000000000000, -0.000000000000000000, -0.000000000000000000 ) ) ;
#555 = EDGE_CURVE ( 'NONE', #16750, #43974, #5886, .T. ) ;
#556 = ORIENTED_EDGE ( 'NONE', *, *, #41925, .F. ) ;
#557 = VECTOR ( 'NONE', #31928, 1000.000000000000000 ) ;
#558 = CARTESIAN_POINT ( 'NONE',  ( 11.99999999999999822, 0.000000000000000000, 0.000000000000000000 ) ) ;
#559 = ORIENTED_EDGE ( 'NONE', *, *, #10857, .F. ) ;
#560 = ORIENTED_EDGE ( 'NONE', *, *, #33166, .F. ) ;
#561 = EDGE_CURVE ( 'NONE', #22588, #42551, #8244, .T. ) ;
#562 = EDGE_CURVE ( 'NONE', #29283, #1846, #39411, .T. ) ;
#563 = CIRCLE ( 'NONE', #16197, 37.49900000000000233 ) ;
#564 = DIRECTION ( 'NONE',  ( 1.000000000000000000, 0.000000000000000000, 0.000000000000000000 ) ) ;
#565 = ORIENTED_EDGE ( 'NONE', *, *, #8773, .T. ) ;
#566 = CARTESIAN_POINT ( 'NONE',  ( 5.000000000000000000, -39.04073710021332744, -15.48615015657624205 ) ) ;
#568 = ORIENTED_EDGE ( 'NONE', *, *, #2288, .F. ) ;
#567 = LINE ( 'NONE', #45118, #45725 ) ;
#569 = ORIENTED_EDGE ( 'NONE', *, *, #23324, .F. ) ;
#570 = CARTESIAN_POINT ( 'NONE',  ( 16.30584220631899228, -140.9432449716519784, 5.500000000000000000 ) ) ;
#571 = CARTESIAN_POINT ( 'NONE',  ( 1.029419772574596825, -118.9089936151275140, 2.500000000000000000 ) ) ;
#572 = CARTESIAN_POINT ( 'NONE',  ( 0.000000000000000000, 35.92658777277525672, -10.74501242461245809 ) ) ;
#573 = ADVANCED_FACE ( 'NONE', ( #39161 ), #35489, .T. ) ;
#576 = ORIENTED_EDGE ( 'NONE', *, *, #44143, .F. ) ;
#575 = DIRECTION ( 'NONE',  ( 0.000000000000000000, 0.000000000000000000, -1.000000000000000000 ) ) ;
#574 = AXIS2_PLACEMENT_3D ( 'NONE', #17954, #2794, #25781 ) ;
#577 = ORIENTED_EDGE ( 'NONE', *, *, #21771, .T. ) ;
#578 = PLANE ( 'NONE',  #34185 ) ;
#579 = ORIENTED_EDGE ( 'NONE', *, *, #16817, .F. ) ;
#580 = ORIENTED_EDGE ( 'NONE', *, *, #37141, .T. ) ;
#581 = FACE_OUTER_BOUND ( 'NONE', #182, .T. ) ;
#582 = AXIS2_PLACEMENT_3D ( 'NONE', #32036, #28341, #6089 ) ;
#583 = DIRECTION ( 'NONE',  ( 0.000000000000000000, -6.938893903907231533E-15, 1.000000000000000000 ) ) ;
#584 = DIRECTION ( 'NONE',  ( -1.000000000000000000, 0.000000000000000000, -0.000000000000000000 ) ) ;
#585 = DIRECTION ( 'NONE',  ( 1.000000000000000000, -0.000000000000000000, -0.000000000000000000 ) ) ;
#586 = ORIENTED_EDGE ( 'NONE', *, *, #36028, .F. ) ;
#587 = DIRECTION ( 'NONE',  ( -1.000000000000000000, -0.000000000000000000, -0.000000000000000000 ) ) ;
#588 = CARTESIAN_POINT ( 'NONE',  ( -10.00000000000000000, 0.000000000000000000, 0.000000000000000000 ) ) ;
#589 = CARTESIAN_POINT ( 'NONE',  ( 11.99999999999999822, -75.11764819372145041, -2.946379043147127064 ) ) ;
#590 = CARTESIAN_POINT ( 'NONE',  ( 11.99999999999999822, 70.52718814184294160, -26.02418014898236720 ) ) ;
#591 = DIRECTION ( 'NONE',  ( 0.000000000000000000, 0.000000000000000000, 1.000000000000000000 ) ) ;
#592 = VECTOR ( 'NONE', #29908, 1000.000000000000000 ) ;
#593 = CARTESIAN_POINT ( 'NONE',  ( 11.99999999999999822, 23.16143007188530589, -73.95703589263951017 ) ) ;
#594 = LINE ( 'NONE', #15524, #29851 ) ;
#595 = DIRECTION ( 'NONE',  ( 0.000000000000000000, 0.000000000000000000, 1.000000000000000000 ) ) ;
#596 = DIRECTION ( 'NONE',  ( -1.000000000000000000, -0.000000000000000000, -0.000000000000000000 ) ) ;
#597 = CYLINDRICAL_SURFACE ( 'NONE', #16693, 16.00000000000000000 ) ;
#598 = CARTESIAN_POINT ( 'NONE',  ( 4.903647372192503795, -146.0423547792665886, 2.500000000000000000 ) ) ;
#599 = VECTOR ( 'NONE', #28662, 1000.000000000000000 ) ;
#600 = CARTESIAN_POINT ( 'NONE',  ( 10.00000000000000000, 20.41045688087824317, 72.35160999960824313 ) ) ;
#601 = CARTESIAN_POINT ( 'NONE',  ( 20.85212586905262100, -130.9402397935870965, 5.500000000000000000 ) ) ;
#602 = DIRECTION ( 'NONE',  ( 0.000000000000000000, 0.8910065241883655673, 0.4539904997395510233 ) ) ;
#603 = ORIENTED_EDGE ( 'NONE', *, *, #34407, .F. ) ;
#604 = ADVANCED_FACE ( 'NONE', ( #14175 ), #10985, .T. ) ;
#605 = ADVANCED_BREP_SHAPE_REPRESENTATION ( '', ( #3244, #11636 ), #6986 ) ;
#606 = EDGE_CURVE ( 'NONE', #20108, #44086, #18071, .T. ) ;
#607 = CYLINDRICAL_SURFACE ( 'NONE', #35407, 77.49899999999999523 ) ;
#608 = ADVANCED_FACE ( 'NONE', ( #40130 ), #32540, .F. ) ;
#609 = EDGE_LOOP ( 'NONE', ( #7379, #41637, #36281, #24453 ) ) ;
#610 = AXIS2_PLACEMENT_3D ( 'NONE', #4448, #45074, #4672 ) ;
#611 = ADVANCED_FACE ( 'NONE', ( #47931 ), #25903, .T. ) ;
#612 = CIRCLE ( 'NONE', #38144, 16.00000000000000355 ) ;
#613 = EDGE_LOOP ( 'NONE', ( #246, #43774, #36331, #19803 ) ) ;
#614 = DIRECTION ( 'NONE',  ( 0.000000000000000000, 0.000000000000000000, 1.000000000000000000 ) ) ;
#615 = ORIENTED_EDGE ( 'NONE', *, *, #34197, .T. ) ;
#616 = ADVANCED_FACE ( 'NONE', ( #6592 ), #18570, .T. ) ;
#617 = DIRECTION ( 'NONE',  ( 0.000000000000000000, 0.2334453638558991462, 0.9723699203976781114 ) ) ;
#618 = EDGE_CURVE ( 'NONE', #28447, #9412, #30123, .T. ) ;
#619 = DIRECTION ( 'NONE',  ( 0.000000000000000000, 0.000000000000000000, 1.000000000000000000 ) ) ;
#621 = ORIENTED_EDGE ( 'NONE', *, *, #41797, .T. ) ;
#620 = CARTESIAN_POINT ( 'NONE',  ( 10.00000000000000000, -10.41901085202050403, -40.68715046381940681 ) ) ;
#622 = EDGE_LOOP ( 'NONE', ( #38651, #1089, #2965, #8815 ) ) ;
#623 = DIRECTION ( 'NONE',  ( 0.000000000000000000, 0.000000000000000000, 1.000000000000000000 ) ) ;
#624 = ORIENTED_EDGE ( 'NONE', *, *, #30351, .F. ) ;
#625 = ORIENTED_EDGE ( 'NONE', *, *, #43707, .T. ) ;
#626 = LINE ( 'NONE', #4313, #10010 ) ;
#627 = LINE ( 'NONE', #33665, #22788 ) ;
#628 = CIRCLE ( 'NONE', #35006, 77.49899999999999523 ) ;
#629 = EDGE_CURVE ( 'NONE', #239, #20013, #47344, .T. ) ;
#630 = ORIENTED_EDGE ( 'NONE', *, *, #5378, .T. ) ;
#631 = EDGE_LOOP ( 'NONE', ( #17363, #21113 ) ) ;
#632 = ORIENTED_EDGE ( 'NONE', *, *, #24201, .T. ) ;
#633 = DIRECTION ( 'NONE',  ( 1.000000000000000000, 0.000000000000000000, 0.000000000000000000 ) ) ;
#634 = ORIENTED_EDGE ( 'NONE', *, *, #31497, .F. ) ;
#635 = DIRECTION ( 'NONE',  ( 0.000000000000000000, -0.1045284632676578424, 0.9945218953682729568 ) ) ;
#636 = DIRECTION ( 'NONE',  ( 0.000000000000000000, -0.5877852522924625900, -0.8090169943749551118 ) ) ;
#637 = DIRECTION ( 'NONE',  ( -1.000000000000000000, 0.000000000000000000, 0.000000000000000000 ) ) ;
#638 = CARTESIAN_POINT ( 'NONE',  ( 0.000000000000000000, -73.44644590900043113, -24.73286445877782924 ) ) ;
#639 = PLANE ( 'NONE',  #10239 ) ;
#640 = DIRECTION ( 'NONE',  ( -1.000000000000000000, 0.000000000000000000, 0.000000000000000000 ) ) ;
#641 = CARTESIAN_POINT ( 'NONE',  ( 0.000000000000000000, -74.18225833017913828, 34.94270380257611919 ) ) ;
#642 = DIRECTION ( 'NONE',  ( -0.000000000000000000, 1.000000000000000000, 0.000000000000000000 ) ) ;
#643 = CARTESIAN_POINT ( 'NONE',  ( 5.000000000000000000, 39.04073710021366139, -15.48615015657542138 ) ) ;
#644 = ORIENTED_EDGE ( 'NONE', *, *, #19554, .F. ) ;
#645 = EDGE_CURVE ( 'NONE', #28702, #28196, #9047, .T. ) ;
#646 = CARTESIAN_POINT ( 'NONE',  ( 0.000000000000000000, 74.18225833017937987, -34.94270380257560049 ) ) ;
#647 = AXIS2_PLACEMENT_3D ( 'NONE', #9074, #34765, #1982 ) ;
#648 = VERTEX_POINT ( 'NONE', #33003 ) ;
#649 = ORIENTED_EDGE ( 'NONE', *, *, #42063, .F. ) ;
#650 = CARTESIAN_POINT ( 'NONE',  ( 11.99999999999999822, 72.35160999960817207, 20.41045688087850607 ) ) ;
#651 = AXIS2_PLACEMENT_3D ( 'NONE', #9967, #24891, #25367 ) ;
#652 = CYLINDRICAL_SURFACE ( 'NONE', #35679, 31.99999999999998579 ) ;
#653 = DIRECTION ( 'NONE',  ( -1.000000000000000000, 0.000000000000000000, 0.000000000000000000 ) ) ;
#654 = DIRECTION ( 'NONE',  ( -1.000000000000000000, 0.000000000000000000, 0.000000000000000000 ) ) ;
#655 = AXIS2_PLACEMENT_3D ( 'NONE', #32476, #47405, #13879 ) ;
#656 = PLANE ( 'NONE',  #42750 ) ;
#657 = CYLINDRICAL_SURFACE ( 'NONE', #22466, 32.00000000000000000 ) ;
#658 = LINE ( 'NONE', #45694, #5225 ) ;
#659 = DIRECTION ( 'NONE',  ( -1.000000000000000000, 0.000000000000000000, 0.000000000000000000 ) ) ;
#660 = EDGE_CURVE ( 'NONE', #19520, #43729, #39526, .T. ) ;
#661 = EDGE_CURVE ( 'NONE', #30938, #23562, #21515, .T. ) ;
#662 = PRESENTATION_STYLE_ASSIGNMENT (( #11926 ) ) ;
#663 = CARTESIAN_POINT ( 'NONE',  ( 12.00000000000000000, 23.49999999999999645, -1.500000000000003997 ) ) ;
#664 = EDGE_CURVE ( 'NONE', #21593, #23778, #16081, .T. ) ;
#665 = ORIENTED_EDGE ( 'NONE', *, *, #3488, .F. ) ;
#666 = CIRCLE ( 'NONE', #23340, 82.00000000000000000 ) ;
#667 = EDGE_CURVE ( 'NONE', #33047, #27075, #32761, .T. ) ;
#668 = ORIENTED_EDGE ( 'NONE', *, *, #4841, .F. ) ;
#669 = ORIENTED_EDGE ( 'NONE', *, *, #7293, .T. ) ;
#670 = DIRECTION ( 'NONE',  ( 0.000000000000000000, 0.8090169943749486725, -0.5877852522924713607 ) ) ;
#671 = CYLINDRICAL_SURFACE ( 'NONE', #3431, 12.49999999999999645 ) ;
#672 = ORIENTED_EDGE ( 'NONE', *, *, #10306, .F. ) ;
#673 = ORIENTED_EDGE ( 'NONE', *, *, #36061, .T. ) ;
#674 = DIRECTION ( 'NONE',  ( -1.000000000000000000, 0.000000000000000000, 0.000000000000000000 ) ) ;
#675 = VERTEX_POINT ( 'NONE', #43788 ) ;
#676 = ORIENTED_EDGE ( 'NONE', *, *, #28784, .F. ) ;
#677 = AXIS2_PLACEMENT_3D ( 'NONE', #21476, #3341, #40339 ) ;
#678 = VECTOR ( 'NONE', #24830, 1000.000000000000114 ) ;
#679 = CARTESIAN_POINT ( 'NONE',  ( 0.000000000000000000, -37.16516213103273714, -4.992566952385376844 ) ) ;
#681 = ORIENTED_EDGE ( 'NONE', *, *, #2964, .F. ) ;
#680 = FACE_OUTER_BOUND ( 'NONE', #41723, .T. ) ;
#682 = CARTESIAN_POINT ( 'NONE',  ( 10.00000000000000000, -21.53537804866103045, 30.80686688397002371 ) ) ;
#683 = EDGE_LOOP ( 'NONE', ( #21682, #11838, #793, #16650 ) ) ;
#684 = CARTESIAN_POINT ( 'NONE',  ( 11.99999999999999822, 0.000000000000000000, 0.000000000000000000 ) ) ;
#685 = ORIENTED_EDGE ( 'NONE', *, *, #43394, .F. ) ;
#686 = ORIENTED_EDGE ( 'NONE', *, *, #40398, .T. ) ;
#687 = CARTESIAN_POINT ( 'NONE',  ( -3.000000000000000000, -0.9646360437375307573, 23.52805723605590060 ) ) ;
#688 = CARTESIAN_POINT ( 'NONE',  ( 11.99999999999999822, 0.000000000000000000, 0.000000000000000000 ) ) ;
#689 = DIRECTION ( 'NONE',  ( 0.000000000000000000, 0.000000000000000000, 1.000000000000000000 ) ) ;
#690 = VERTEX_POINT ( 'NONE', #14422 ) ;
#691 = ORIENTED_EDGE ( 'NONE', *, *, #27156, .F. ) ;
#692 = LINE ( 'NONE', #22726, #7106 ) ;
#693 = PLANE ( 'NONE',  #5618 ) ;
#694 = ORIENTED_EDGE ( 'NONE', *, *, #7584, .T. ) ;
#695 = APPLICATION_CONTEXT ( 'automotive_design' ) ;
#696 = DIRECTION ( 'NONE',  ( -1.000000000000000000, -0.000000000000000000, 0.000000000000000000 ) ) ;
#697 = VERTEX_POINT ( 'NONE', #29093 ) ;
#698 = DIRECTION ( 'NONE',  ( -1.000000000000000000, 0.000000000000000000, 0.000000000000000000 ) ) ;
#699 = CARTESIAN_POINT ( 'NONE',  ( 0.000000000000000000, 77.19088730480524418, 6.903761155838049390 ) ) ;
#700 = CARTESIAN_POINT ( 'NONE',  ( 0.000000000000000000, -17.28742895386031719, -75.54627589209962935 ) ) ;
#701 = DIRECTION ( 'NONE',  ( -1.000000000000000000, -0.000000000000000000, -0.000000000000000000 ) ) ;
#702 = CARTESIAN_POINT ( 'NONE',  ( 0.000000000000000000, -68.55367621811112144, -44.99326035066125939 ) ) ;
#703 = CARTESIAN_POINT ( 'NONE',  ( 0.000000000000000000, -35.38097989696520074, 12.42422080174625520 ) ) ;
#704 = CARTESIAN_POINT ( 'NONE',  ( 10.00000000000000000, -72.35432306680498016, 20.40083707022857951 ) ) ;
#705 = CARTESIAN_POINT ( 'NONE',  ( 0.000000000000000000, 56.15606465354958488, 59.75363087400094741 ) ) ;
#706 = CIRCLE ( 'NONE', #20238, 77.49900000000000944 ) ;
#707 = CARTESIAN_POINT ( 'NONE',  ( 10.00000000000000000, -46.11716303203234446, 67.80270845531873647 ) ) ;
#708 = VERTEX_POINT ( 'NONE', #39885 ) ;
#709 = ADVANCED_FACE ( 'NONE', ( #21264 ), #44029, .T. ) ;
#710 = VECTOR ( 'NONE', #35157, 1000.000000000000000 ) ;
#711 = DIRECTION ( 'NONE',  ( -1.000000000000000000, 0.000000000000000000, -0.000000000000000000 ) ) ;
#712 = CYLINDRICAL_SURFACE ( 'NONE', #5093, 82.00000000000000000 ) ;
#713 = ADVANCED_FACE ( 'NONE', ( #33259 ), #6835, .T. ) ;
#715 = VERTEX_POINT ( 'NONE', #2662 ) ;
#714 = AXIS2_PLACEMENT_3D ( 'NONE', #45123, #37045, #11592 ) ;
#716 = CARTESIAN_POINT ( 'NONE',  ( 10.00000000000000000, -6.555932627142143865, -37.01155633439065440 ) ) ;
#717 = ORIENTED_EDGE ( 'NONE', *, *, #17572, .F. ) ;
#718 = UNCERTAINTY_MEASURE_WITH_UNIT (LENGTH_MEASURE( 1.000000000000000082E-05 ), #46005, 'distance_accuracy_value', 'NONE');
#719 = DIRECTION ( 'NONE',  ( 0.000000000000000000, 0.5000000000000028866, 0.8660254037844369313 ) ) ;
#720 = EDGE_CURVE ( 'NONE', #1645, #9950, #13569, .T. ) ;
#721 = EDGE_CURVE ( 'NONE', #7607, #27429, #23665, .T. ) ;
#722 = LINE ( 'NONE', #11518, #33116 ) ;
#723 = LINE ( 'NONE', #22755, #12067 ) ;
#724 = ORIENTED_EDGE ( 'NONE', *, *, #41620, .T. ) ;
#725 =( GEOMETRIC_REPRESENTATION_CONTEXT ( 3 ) GLOBAL_UNCERTAINTY_ASSIGNED_CONTEXT ( ( #225 ) ) GLOBAL_UNIT_ASSIGNED_CONTEXT ( ( #18543, #39862, #44251 ) ) REPRESENTATION_CONTEXT ( 'NONE', 'WORKASPACE' ) );
#726 = CARTESIAN_POINT ( 'NONE',  ( 10.00000000000000000, 0.6853352020795618893, -37.58145647212453611 ) ) ;
#727 = ORIENTED_EDGE ( 'NONE', *, *, #37638, .F. ) ;
#728 = ORIENTED_EDGE ( 'NONE', *, *, #7555, .T. ) ;
#729 = CIRCLE ( 'NONE', #29676, 31.99999999999998579 ) ;
#730 = CARTESIAN_POINT ( 'NONE',  ( 20.85212586905262100, -130.9402397935870965, 2.500000000000000000 ) ) ;
#732 = ORIENTED_EDGE ( 'NONE', *, *, #4706, .T. ) ;
#731 = AXIS2_PLACEMENT_3D ( 'NONE', #30251, #12141, #377 ) ;
#733 = CARTESIAN_POINT ( 'NONE',  ( -23.30023580412278505, -123.4057321492263384, -5.500000000000000000 ) ) ;
#734 = ORIENTED_EDGE ( 'NONE', *, *, #13088, .T. ) ;
#735 = LINE ( 'NONE', #38434, #18069 ) ;
#736 = ORIENTED_EDGE ( 'NONE', *, *, #18878, .F. ) ;
#737 = CIRCLE ( 'NONE', #34347, 32.00000000000000000 ) ;
#738 = DIRECTION ( 'NONE',  ( 0.000000000000000000, 0.000000000000000000, 1.000000000000000000 ) ) ;
#739 = LINE ( 'NONE', #4192, #39255 ) ;
#740 = ORIENTED_EDGE ( 'NONE', *, *, #7261, .F. ) ;
#741 = FACE_OUTER_BOUND ( 'NONE', #31676, .T. ) ;
#742 = ORIENTED_EDGE ( 'NONE', *, *, #33981, .F. ) ;
#744 = ORIENTED_EDGE ( 'NONE', *, *, #10469, .F. ) ;
#743 = FACE_OUTER_BOUND ( 'NONE', #7183, .T. ) ;
#745 = ADVANCED_FACE ( 'NONE', ( #194 ), #26408, .T. ) ;
#746 = CARTESIAN_POINT ( 'NONE',  ( -10.00000000000000000, 0.000000000000000000, 0.000000000000000000 ) ) ;
#747 = VERTEX_POINT ( 'NONE', #30811 ) ;
#748 = CARTESIAN_POINT ( 'NONE',  ( -7.572224309238338336, -145.4393675041377492, 5.500000000000000000 ) ) ;
#749 = VECTOR ( 'NONE', #11834, 1000.000000000000000 ) ;
#750 = CYLINDRICAL_SURFACE ( 'NONE', #22884, 37.49900000000000233 ) ;
#751 = LINE ( 'NONE', #15941, #40255 ) ;
#752 = ADVANCED_FACE ( 'NONE', ( #11712 ), #22720, .F. ) ;
#753 = CARTESIAN_POINT ( 'NONE',  ( 12.49999999999999645, 1.530808498934191127E-15, 125.0000000000000000 ) ) ;
#754 = CYLINDRICAL_SURFACE ( 'NONE', #7068, 42.00000000000000000 ) ;
#755 = DIRECTION ( 'NONE',  ( 0.000000000000000000, 0.000000000000000000, 1.000000000000000000 ) ) ;
#756 = EDGE_CURVE ( 'NONE', #40958, #16750, #45009, .T. ) ;
#757 = LINE ( 'NONE', #37729, #2312 ) ;
#758 = CARTESIAN_POINT ( 'NONE',  ( 10.00000000000000000, 30.41916302227113178, 71.27951684758036777 ) ) ;
#759 = CARTESIAN_POINT ( 'NONE',  ( 10.00000000000000000, 6.555932627142952995, -37.01155633439051940 ) ) ;
#760 = ORIENTED_EDGE ( 'NONE', *, *, #16844, .T. ) ;
#761 = FACE_OUTER_BOUND ( 'NONE', #5201, .T. ) ;
#762 = CYLINDRICAL_SURFACE ( 'NONE', #35772, 82.00000000000000000 ) ;
#763 = CARTESIAN_POINT ( 'NONE',  ( -10.00000000000000000, 0.000000000000000000, 0.000000000000000000 ) ) ;
#764 = ORIENTED_EDGE ( 'NONE', *, *, #26987, .T. ) ;
#765 = CARTESIAN_POINT ( 'NONE',  ( 11.99999999999999822, 0.000000000000000000, 0.000000000000000000 ) ) ;
#766 = LINE ( 'NONE', #19371, #42587 ) ;
#767 = DIRECTION ( 'NONE',  ( 0.000000000000000000, 0.8526401643540935105, -0.5224985647159466895 ) ) ;
#768 = EDGE_CURVE ( 'NONE', #35835, #19346, #17395, .T. ) ;
#769 = CARTESIAN_POINT ( 'NONE',  ( -13.05994868825747446, -139.5943292883446532, 5.500000000000000000 ) ) ;
#770 = EDGE_CURVE ( 'NONE', #31111, #40387, #22091, .T. ) ;
#771 = ORIENTED_EDGE ( 'NONE', *, *, #42514, .T. ) ;
#772 = EDGE_CURVE ( 'NONE', #17865, #18490, #11973, .T. ) ;
#773 = VERTEX_POINT ( 'NONE', #37412 ) ;
#774 = CIRCLE ( 'NONE', #21067, 37.49900000000001654 ) ;
#775 = CARTESIAN_POINT ( 'NONE',  ( 12.00000000000000000, 20.85821328998756385, 10.92862929874494249 ) ) ;
#776 = CIRCLE ( 'NONE', #14873, 15.99999999999999822 ) ;
#777 = ORIENTED_EDGE ( 'NONE', *, *, #41476, .T. ) ;
#778 = CARTESIAN_POINT ( 'NONE',  ( -3.000000000000000000, -26.23277895567245821, -4.042438405570103477 ) ) ;
#779 = AXIS2_PLACEMENT_3D ( 'NONE', #14946, #44074, #36487 ) ;
#780 = SHAPE_DEFINITION_REPRESENTATION ( #5794, #22809 ) ;
#781 = EDGE_LOOP ( 'NONE', ( #17034, #22607, #22558, #21129 ) ) ;
#782 = EDGE_CURVE ( 'NONE', #24639, #37652, #34589, .T. ) ;
#783 = CYLINDRICAL_SURFACE ( 'NONE', #16695, 82.00000000000000000 ) ;
#784 = ORIENTED_EDGE ( 'NONE', *, *, #48196, .T. ) ;
#785 = CIRCLE ( 'NONE', #47688, 16.00000000000000355 ) ;
#786 = AXIS2_PLACEMENT_3D ( 'NONE', #16949, #35064, #31906 ) ;
#787 = LINE ( 'NONE', #33836, #29193 ) ;
#788 = EDGE_CURVE ( 'NONE', #34900, #7136, #30324, .T. ) ;
#789 = ORIENTED_EDGE ( 'NONE', *, *, #23042, .T. ) ;
#790 = PLANE ( 'NONE',  #33904 ) ;
#791 = DIRECTION ( 'NONE',  ( -1.000000000000000000, 0.000000000000000000, 0.000000000000000000 ) ) ;
#792 = CARTESIAN_POINT ( 'NONE',  ( 0.1219594728601484379, -121.4950337410840149, 2.500000000000000000 ) ) ;
#793 = ORIENTED_EDGE ( 'NONE', *, *, #14867, .F. ) ;
#794 = CARTESIAN_POINT ( 'NONE',  ( 10.00000000000000000, 41.76106447765580043, -62.50884508063379741 ) ) ;
#795 = DIRECTION ( 'NONE',  ( 1.000000000000000000, 0.000000000000000000, 0.000000000000000000 ) ) ;
#796 = ADVANCED_FACE ( 'NONE', ( #15397 ), #45242, .T. ) ;
#797 = LINE ( 'NONE', #12088, #13433 ) ;
#798 = CIRCLE ( 'NONE', #14870, 82.00000000000000000 ) ;
#799 = CYLINDRICAL_SURFACE ( 'NONE', #46893, 20.99999999999999645 ) ;
#800 = EDGE_CURVE ( 'NONE', #47535, #10792, #4146, .T. ) ;
#801 = ORIENTED_EDGE ( 'NONE', *, *, #27801, .T. ) ;
#802 = CARTESIAN_POINT ( 'NONE',  ( 10.00000000000000000, 22.64427369931212297, -30.00120703465181293 ) ) ;
#803 = ORIENTED_EDGE ( 'NONE', *, *, #18055, .T. ) ;
#804 = ORIENTED_EDGE ( 'NONE', *, *, #24709, .F. ) ;
#805 = CARTESIAN_POINT ( 'NONE',  ( 10.00000000000000178, 0.000000000000000000, 0.000000000000000000 ) ) ;
#806 = AXIS2_PLACEMENT_3D ( 'NONE', #23101, #7683, #8409 ) ;
#807 = CIRCLE ( 'NONE', #34414, 77.49899999999999523 ) ;
#808 = EDGE_CURVE ( 'NONE', #42195, #25666, #13500, .T. ) ;
#809 = CYLINDRICAL_SURFACE ( 'NONE', #2722, 82.00000000000000000 ) ;
#810 = DIRECTION ( 'NONE',  ( 0.000000000000000000, 0.4539904997395413644, 0.8910065241883706744 ) ) ;
#811 = CARTESIAN_POINT ( 'NONE',  ( 11.99999999999999822, -71.27951684758045303, 30.41916302227090085 ) ) ;
#812 = ORIENTED_EDGE ( 'NONE', *, *, #18312, .T. ) ;
#813 = DIRECTION ( 'NONE',  ( -1.000000000000000000, 0.000000000000000000, 0.000000000000000000 ) ) ;
#814 = EDGE_CURVE ( 'NONE', #4586, #33388, #24439, .T. ) ;
#815 = CARTESIAN_POINT ( 'NONE',  ( 10.00000000000000000, -12.26510123303234501, -35.53030884539098366 ) ) ;
#816 = DIRECTION ( 'NONE',  ( 1.000000000000000000, 0.000000000000000000, 0.000000000000000000 ) ) ;
#817 = CYLINDRICAL_SURFACE ( 'NONE', #34592, 77.49899999999999523 ) ;
#818 = DIRECTION ( 'NONE',  ( 0.000000000000000000, 0.000000000000000000, -1.000000000000000000 ) ) ;
#819 = CIRCLE ( 'NONE', #2393, 16.00000000000000355 ) ;
#820 = LINE ( 'NONE', #30223, #45753 ) ;
#821 = DIRECTION ( 'NONE',  ( -1.000000000000000000, -0.000000000000000000, 0.000000000000000000 ) ) ;
#822 = DIRECTION ( 'NONE',  ( 0.000000000000000000, 0.000000000000000000, 1.000000000000000000 ) ) ;
#823 = DIRECTION ( 'NONE',  ( -1.000000000000000000, 0.000000000000000000, 0.000000000000000000 ) ) ;
#824 = CARTESIAN_POINT ( 'NONE',  ( 10.00000000000000000, 37.48860685352291000, -0.8828120875901940279 ) ) ;
#825 = EDGE_CURVE ( 'NONE', #38067, #45904, #11958, .T. ) ;
#826 = EDGE_CURVE ( 'NONE', #20918, #40419, #19730, .T. ) ;
#827 = CARTESIAN_POINT ( 'NONE',  ( 12.00000000000000355, 2.571758278209441661E-15, -21.00000000000000000 ) ) ;
#828 = VERTEX_POINT ( 'NONE', #23209 ) ;
#829 = CARTESIAN_POINT ( 'NONE',  ( 10.00000000000000000, 0.000000000000000000, 37.49900000000000233 ) ) ;
#830 = CARTESIAN_POINT ( 'NONE',  ( 6.782329983125267248, 10.49999999999999645, -105.0000000000000000 ) ) ;
#831 = LINE ( 'NONE', #10898, #11447 ) ;
#832 = ORIENTED_EDGE ( 'NONE', *, *, #10836, .F. ) ;
#833 = LINE ( 'NONE', #11630, #4915 ) ;
#834 = ORIENTED_EDGE ( 'NONE', *, *, #44618, .F. ) ;
#835 = ADVANCED_FACE ( 'NONE', ( #4609 ), #34448, .T. ) ;
#836 = CIRCLE ( 'NONE', #46174, 82.00000000000000000 ) ;
#837 = CIRCLE ( 'NONE', #14133, 82.00000000000000000 ) ;
#838 = ORIENTED_EDGE ( 'NONE', *, *, #16567, .F. ) ;
#839 = AXIS2_PLACEMENT_3D ( 'NONE', #13782, #32608, #9855 ) ;
#840 = AXIS2_PLACEMENT_3D ( 'NONE', #6349, #2417, #28626 ) ;
#841 = ORIENTED_EDGE ( 'NONE', *, *, #9017, .F. ) ;
#842 = VERTEX_POINT ( 'NONE', #29823 ) ;
#843 = DIRECTION ( 'NONE',  ( -1.000000000000000000, -0.000000000000000000, -0.000000000000000000 ) ) ;
#844 = VERTEX_POINT ( 'NONE', #44749 ) ;
#845 = AXIS2_PLACEMENT_3D ( 'NONE', #12506, #45535, #19573 ) ;
#846 = AXIS2_PLACEMENT_3D ( 'NONE', #12039, #42367, #4917 ) ;
#847 = CARTESIAN_POINT ( 'NONE',  ( 10.00000000000000000, -59.46389618801999433, 49.70050353004867816 ) ) ;
#848 = CIRCLE ( 'NONE', #7885, 31.99999999999998579 ) ;
#849 = LINE ( 'NONE', #7234, #16375 ) ;
#850 = DIRECTION ( 'NONE',  ( 0.000000000000000000, -0.5877852522924689183, -0.8090169943749504489 ) ) ;
#851 = ORIENTED_EDGE ( 'NONE', *, *, #38332, .T. ) ;
#852 = FACE_OUTER_BOUND ( 'NONE', #8625, .T. ) ;
#853 = ORIENTED_EDGE ( 'NONE', *, *, #27879, .T. ) ;
#854 = DIRECTION ( 'NONE',  ( 1.000000000000000000, 0.000000000000000000, 0.000000000000000000 ) ) ;
#855 = FACE_OUTER_BOUND ( 'NONE', #20424, .T. ) ;
#856 = EDGE_LOOP ( 'NONE', ( #31821, #46197, #31070, #23598 ) ) ;
#857 = ORIENTED_EDGE ( 'NONE', *, *, #37873, .T. ) ;
#858 = CARTESIAN_POINT ( 'NONE',  ( 5.000000000000000000, 32.34446384430010113, -26.79245525562679831 ) ) ;
#859 = ORIENTED_EDGE ( 'NONE', *, *, #34994, .T. ) ;
#860 = DIRECTION ( 'NONE',  ( 0.000000000000000000, 0.000000000000000000, 1.000000000000000000 ) ) ;
#861 = EDGE_CURVE ( 'NONE', #2920, #21783, #40860, .T. ) ;
#862 = DIRECTION ( 'NONE',  ( -1.000000000000000000, 0.000000000000000000, 0.000000000000000000 ) ) ;
#863 = DIRECTION ( 'NONE',  ( -1.000000000000000000, 0.000000000000000000, 0.000000000000000000 ) ) ;
#864 = CARTESIAN_POINT ( 'NONE',  ( -14.87942725330654348, -141.9795960975983178, 5.500000000000000000 ) ) ;
#865 = CARTESIAN_POINT ( 'NONE',  ( 10.00000000000000000, -63.18004540532994184, -44.88180994100446952 ) ) ;
#866 = LINE ( 'NONE', #30749, #3355 ) ;
#867 = ADVANCED_FACE ( 'NONE', ( #3881 ), #46705, .T. ) ;
#868 = DIRECTION ( 'NONE',  ( -1.000000000000000000, -0.000000000000000000, -0.000000000000000000 ) ) ;
#869 = FACE_OUTER_BOUND ( 'NONE', #6666, .T. ) ;
#870 = CYLINDRICAL_SURFACE ( 'NONE', #41795, 82.00000000000000000 ) ;
#871 = DIRECTION ( 'NONE',  ( 0.000000000000000000, 0.6691306063588569053, 0.7431448254773954654 ) ) ;
#872 = LINE ( 'NONE', #4802, #26195 ) ;
#873 = ORIENTED_EDGE ( 'NONE', *, *, #27466, .T. ) ;
#874 = ORIENTED_EDGE ( 'NONE', *, *, #29513, .T. ) ;
#875 = CIRCLE ( 'NONE', #1653, 32.00000000000000000 ) ;
#876 = DIRECTION ( 'NONE',  ( 0.000000000000000000, 0.5877852522924744694, -0.8090169943749465631 ) ) ;
#877 = AXIS2_PLACEMENT_3D ( 'NONE', #15679, #17351, #43081 ) ;
#878 = AXIS2_PLACEMENT_3D ( 'NONE', #26880, #35416, #24170 ) ;
#879 = LINE ( 'NONE', #34648, #19134 ) ;
#880 = DIRECTION ( 'NONE',  ( 0.000000000000000000, -0.5877852522924625900, -0.8090169943749551118 ) ) ;
#881 = DIRECTION ( 'NONE',  ( -1.000000000000000000, 0.000000000000000000, 0.000000000000000000 ) ) ;
#882 = EDGE_CURVE ( 'NONE', #4419, #38922, #39322, .T. ) ;
#883 = CARTESIAN_POINT ( 'NONE',  ( 0.000000000000000000, 0.000000000000000000, 0.000000000000000000 ) ) ;
#884 = CARTESIAN_POINT ( 'NONE',  ( 10.00000000000000000, 37.22597642581158084, -5.202137450156524068 ) ) ;
#885 = ORIENTED_EDGE ( 'NONE', *, *, #47454, .F. ) ;
#886 = CARTESIAN_POINT ( 'NONE',  ( 10.00000000000000000, 0.000000000000000000, 0.000000000000000000 ) ) ;
#887 = CARTESIAN_POINT ( 'NONE',  ( 10.00000000000000000, 6.903761155838878061, -77.19088730480517313 ) ) ;
#888 = EDGE_CURVE ( 'NONE', #38891, #23195, #37753, .T. ) ;
#889 = AXIS2_PLACEMENT_3D ( 'NONE', #38696, #5883, #2196 ) ;
#890 = SURFACE_SIDE_STYLE ('',( #34415 ) ) ;
#891 = CARTESIAN_POINT ( 'NONE',  ( -10.00000000000000000, 0.000000000000000000, 0.000000000000000000 ) ) ;
#892 = ORIENTED_EDGE ( 'NONE', *, *, #13818, .F. ) ;
#893 = EDGE_CURVE ( 'NONE', #25663, #39708, #9572, .T. ) ;
#894 = VERTEX_POINT ( 'NONE', #39345 ) ;
#895 = ORIENTED_EDGE ( 'NONE', *, *, #6333, .T. ) ;
#896 = CARTESIAN_POINT ( 'NONE',  ( -10.43921258969510824, -98.89258801967538659, 5.500000000000000000 ) ) ;
#897 = VERTEX_POINT ( 'NONE', #42547 ) ;
#898 = ORIENTED_EDGE ( 'NONE', *, *, #43837, .F. ) ;
#899 = CIRCLE ( 'NONE', #28278, 31.99999999999999645 ) ;
#900 = FACE_OUTER_BOUND ( 'NONE', #34327, .T. ) ;
#901 = VECTOR ( 'NONE', #25481, 1000.000000000000000 ) ;
#902 = ORIENTED_EDGE ( 'NONE', *, *, #18463, .T. ) ;
#903 = ORIENTED_EDGE ( 'NONE', *, *, #45602, .F. ) ;
#904 = VECTOR ( 'NONE', #28225, 999.9999999999998863 ) ;
#905 = VECTOR ( 'NONE', #29776, 1000.000000000000000 ) ;
#906 = DIRECTION ( 'NONE',  ( 0.5200609990133008287, 0.8541291221503266584, -0.000000000000000000 ) ) ;
#908 = VERTEX_POINT ( 'NONE', #20751 ) ;
#907 = CARTESIAN_POINT ( 'NONE',  ( 10.00000000000000000, 22.48208911017551515, -35.47612816024499693 ) ) ;
#909 = DIRECTION ( 'NONE',  ( 0.000000000000000000, 0.000000000000000000, 1.000000000000000000 ) ) ;
#910 = EDGE_LOOP ( 'NONE', ( #134, #29416, #27347, #29269 ) ) ;
#911 = VERTEX_POINT ( 'NONE', #5832 ) ;
#912 = DIRECTION ( 'NONE',  ( 0.000000000000000000, -0.3826834323650969427, 0.9238795325112838519 ) ) ;
#913 = VERTEX_POINT ( 'NONE', #43024 ) ;
#914 = ORIENTED_EDGE ( 'NONE', *, *, #29615, .F. ) ;
#915 = EDGE_CURVE ( 'NONE', #27090, #32864, #9476, .T. ) ;
#916 = CARTESIAN_POINT ( 'NONE',  ( 5.999999999999999112, 59.75363087400076267, 56.15606465354979093 ) ) ;
#917 = DIRECTION ( 'NONE',  ( 0.000000000000000000, 0.000000000000000000, 1.000000000000000000 ) ) ;
#918 = AXIS2_PLACEMENT_3D ( 'NONE', #22717, #15619, #8281 ) ;
#919 = VERTEX_POINT ( 'NONE', #32019 ) ;
#920 = ADVANCED_FACE ( 'NONE', ( #35680 ), #31058, .T. ) ;
#921 = DIRECTION ( 'NONE',  ( -1.000000000000000000, 0.000000000000000000, 0.000000000000000000 ) ) ;
#922 = FACE_OUTER_BOUND ( 'NONE', #42259, .T. ) ;
#923 = VERTEX_POINT ( 'NONE', #46935 ) ;
#924 = EDGE_CURVE ( 'NONE', #15440, #36912, #16644, .T. ) ;
#925 = VERTEX_POINT ( 'NONE', #42791 ) ;
#926 = DIRECTION ( 'NONE',  ( 1.000000000000000000, -0.000000000000000000, 0.000000000000000000 ) ) ;
#927 = EDGE_CURVE ( 'NONE', #44612, #1839, #4897, .T. ) ;
#928 = CARTESIAN_POINT ( 'NONE',  ( -3.000000000000000000, 16.61724383029390140, -20.69703378468903665 ) ) ;
#930 = ADVANCED_FACE ( 'NONE', ( #45978 ), #31294, .T. ) ;
#929 = VERTEX_POINT ( 'NONE', #43263 ) ;
#931 = EDGE_CURVE ( 'NONE', #18736, #38437, #11161, .T. ) ;
#932 = CARTESIAN_POINT ( 'NONE',  ( 0.000000000000000000, -19.89357724624986901, -12.59942793731086041 ) ) ;
#933 = ORIENTED_EDGE ( 'NONE', *, *, #27214, .F. ) ;
#934 = CARTESIAN_POINT ( 'NONE',  ( 10.00000000000000000, -6.903761155837252694, -77.19088730480530103 ) ) ;
#935 = CARTESIAN_POINT ( 'NONE',  ( -15.44521549751111422, -137.7748507232956001, 2.500000000000000000 ) ) ;
#936 = DIRECTION ( 'NONE',  ( -1.000000000000000000, -0.000000000000000000, -0.000000000000000000 ) ) ;
#937 = DIRECTION ( 'NONE',  ( -1.000000000000000000, 0.000000000000000000, -0.000000000000000000 ) ) ;
#938 = LINE ( 'NONE', #4404, #46109 ) ;
#940 = VECTOR ( 'NONE', #6028, 1000.000000000000000 ) ;
#939 = CARTESIAN_POINT ( 'NONE',  ( 0.000000000000000000, -0.6853352020787742971, -37.58145647212455032 ) ) ;
#941 = DIRECTION ( 'NONE',  ( 0.1736481776669309418, -0.9848077530122080203, 0.000000000000000000 ) ) ;
#942 = DIRECTION ( 'NONE',  ( -1.000000000000000000, 0.000000000000000000, 0.000000000000000000 ) ) ;
#943 = ORIENTED_EDGE ( 'NONE', *, *, #31488, .T. ) ;
#944 = AXIS2_PLACEMENT_3D ( 'NONE', #4438, #29878, #37708 ) ;
#945 = CARTESIAN_POINT ( 'NONE',  ( 11.99999999999999822, -36.72794159290197769, -65.59268652807249111 ) ) ;
#946 = CARTESIAN_POINT ( 'NONE',  ( 10.00000000000000000, -37.58145647212455032, 16.68533520207890319 ) ) ;
#947 = CIRCLE ( 'NONE', #11904, 77.49899999999999523 ) ;
#948 = ORIENTED_EDGE ( 'NONE', *, *, #40567, .F. ) ;
#949 = EDGE_CURVE ( 'NONE', #35290, #37233, #9719, .T. ) ;
#950 = DIRECTION ( 'NONE',  ( 0.000000000000000000, 0.9876883405951383255, -0.1564344650402277048 ) ) ;
#951 = AXIS2_PLACEMENT_3D ( 'NONE', #23413, #47391, #6503 ) ;
#952 = CARTESIAN_POINT ( 'NONE',  ( 11.99999999999999822, -23.16143007188479430, 73.95703589263968070 ) ) ;
#953 = EDGE_CURVE ( 'NONE', #32836, #15279, #24665, .T. ) ;
#954 = CARTESIAN_POINT ( 'NONE',  ( 10.00000000000000000, -20.41045688087876897, 72.35160999960810102 ) ) ;
#955 = EDGE_LOOP ( 'NONE', ( #35156, #19832, #28140, #2313 ) ) ;
#956 = VERTEX_POINT ( 'NONE', #20256 ) ;
#957 = EDGE_CURVE ( 'NONE', #21733, #22651, #38640, .T. ) ;
#958 = DIRECTION ( 'NONE',  ( 0.000000000000000000, 0.000000000000000000, 1.000000000000000000 ) ) ;
#959 = CIRCLE ( 'NONE', #40842, 31.99999999999998224 ) ;
#960 = VERTEX_POINT ( 'NONE', #42297 ) ;
#961 = ORIENTED_EDGE ( 'NONE', *, *, #33534, .T. ) ;
#962 = VERTEX_POINT ( 'NONE', #31539 ) ;
#963 = ORIENTED_EDGE ( 'NONE', *, *, #16321, .F. ) ;
#964 = AXIS2_PLACEMENT_3D ( 'NONE', #24083, #12583, #5247 ) ;
#965 = EDGE_CURVE ( 'NONE', #5424, #6597, #20017, .T. ) ;
#966 = CIRCLE ( 'NONE', #47104, 16.00000000000000000 ) ;
#967 = DIRECTION ( 'NONE',  ( 1.000000000000000000, 0.000000000000000000, 0.000000000000000000 ) ) ;
#968 = EDGE_LOOP ( 'NONE', ( #45128, #38184, #40200, #11196 ) ) ;
#969 = ORIENTED_EDGE ( 'NONE', *, *, #15817, .T. ) ;
#970 = CYLINDRICAL_SURFACE ( 'NONE', #19200, 16.00000000000000000 ) ;
#971 = ORIENTED_EDGE ( 'NONE', *, *, #12058, .F. ) ;
#972 = ADVANCED_FACE ( 'NONE', ( #39107 ), #5579, .T. ) ;
#973 = DIRECTION ( 'NONE',  ( -1.000000000000000000, 0.000000000000000000, -0.000000000000000000 ) ) ;
#974 = VECTOR ( 'NONE', #38147, 1000.000000000000000 ) ;
#975 = VERTEX_POINT ( 'NONE', #29535 ) ;
#976 = AXIS2_PLACEMENT_3D ( 'NONE', #12212, #8513, #41339 ) ;
#977 = CARTESIAN_POINT ( 'NONE',  ( 11.99999999999999822, 65.64334221924964652, -41.19522573413665611 ) ) ;
#978 = EDGE_CURVE ( 'NONE', #43018, #47530, #46348, .T. ) ;
#979 = CARTESIAN_POINT ( 'NONE',  ( 0.000000000000000000, 0.000000000000000000, 0.000000000000000000 ) ) ;
#980 = AXIS2_PLACEMENT_3D ( 'NONE', #9861, #42429, #9370 ) ;
#981 = ORIENTED_EDGE ( 'NONE', *, *, #24577, .T. ) ;
#982 = DIRECTION ( 'NONE',  ( 0.000000000000000000, 0.000000000000000000, 1.000000000000000000 ) ) ;
#983 = ORIENTED_EDGE ( 'NONE', *, *, #4572, .T. ) ;
#984 = CYLINDRICAL_SURFACE ( 'NONE', #17972, 31.99999999999999289 ) ;
#985 = CARTESIAN_POINT ( 'NONE',  ( 10.00000000000000000, -62.20884554314051940, 46.21855187248608132 ) ) ;
#986 = ORIENTED_EDGE ( 'NONE', *, *, #39691, .T. ) ;
#987 = CIRCLE ( 'NONE', #17401, 77.49900000000002365 ) ;
#988 = CARTESIAN_POINT ( 'NONE',  ( 0.000000000000000000, -40.65526001592564853, -71.21200624218839437 ) ) ;
#989 = EDGE_LOOP ( 'NONE', ( #38099, #45863, #32407, #6459 ) ) ;
#990 = ORIENTED_EDGE ( 'NONE', *, *, #33029, .T. ) ;
#991 = ADVANCED_FACE ( 'NONE', ( #36397 ), #10703, .T. ) ;
#992 = CARTESIAN_POINT ( 'NONE',  ( 12.00000000000000000, -20.55727247249748402, -16.78983467731284307 ) ) ;
#993 = DIRECTION ( 'NONE',  ( -1.000000000000000000, 0.000000000000000000, 0.000000000000000000 ) ) ;
#994 = VERTEX_POINT ( 'NONE', #33207 ) ;
#995 = CIRCLE ( 'NONE', #22097, 37.49900000000000233 ) ;
#996 = CARTESIAN_POINT ( 'NONE',  ( -12.50000000000000000, -132.5000000000000000, -40.00000000000000000 ) ) ;
#997 = CARTESIAN_POINT ( 'NONE',  ( -8.637688417678550223, 13.69818742750669749, -44.99999999999998579 ) ) ;
#998 = DIRECTION ( 'NONE',  ( 0.000000000000000000, 0.000000000000000000, 1.000000000000000000 ) ) ;
#999 = CARTESIAN_POINT ( 'NONE',  ( 4.999999999999999112, -40.68715046381937128, 10.41901085202062660 ) ) ;
#1000 = CYLINDRICAL_SURFACE ( 'NONE', #43127, 37.49900000000000233 ) ;
#1001 = FACE_OUTER_BOUND ( 'NONE', #11697, .T. ) ;
#1002 = DIRECTION ( 'NONE',  ( -1.000000000000000000, -0.000000000000000000, -0.000000000000000000 ) ) ;
#1003 = CARTESIAN_POINT ( 'NONE',  ( 10.00000000000000000, -21.53537804866058991, -30.80686688397033635 ) ) ;
#1004 = DIRECTION ( 'NONE',  ( -1.000000000000000000, 0.000000000000000000, 0.000000000000000000 ) ) ;
#1005 = ORIENTED_EDGE ( 'NONE', *, *, #37761, .T. ) ;
#1006 = CYLINDRICAL_SURFACE ( 'NONE', #40884, 31.99999999999999289 ) ;
#1007 = DIRECTION ( 'NONE',  ( 0.000000000000000000, 0.000000000000000000, -1.000000000000000000 ) ) ;
#1009 = VECTOR ( 'NONE', #15720, 1000.000000000000000 ) ;
#1008 = CARTESIAN_POINT ( 'NONE',  ( -3.000000000000000000, 26.50000000000000000, -1.500000000000001332 ) ) ;
#1010 = DIRECTION ( 'NONE',  ( 0.000000000000000000, 0.7071067811865487940, -0.7071067811865462405 ) ) ;
#1011 = EDGE_CURVE ( 'NONE', #47351, #17279, #48133, .T. ) ;
#1012 = AXIS2_PLACEMENT_3D ( 'NONE', #9094, #45554, #24027 ) ;
#1013 = VERTEX_POINT ( 'NONE', #43512 ) ;
#1014 = CARTESIAN_POINT ( 'NONE',  ( 10.00000000000000000, -30.00120703465222149, 22.64427369931158296 ) ) ;
#1015 = ORIENTED_EDGE ( 'NONE', *, *, #23172, .F. ) ;
#1016 = CARTESIAN_POINT ( 'NONE',  ( 11.99999999999999822, -30.41916302227164337, 71.27951684758015460 ) ) ;
#1017 = VECTOR ( 'NONE', #5041, 1000.000000000000000 ) ;
#1018 = AXIS2_PLACEMENT_3D ( 'NONE', #794, #30668, #45589 ) ;
#1019 = CONTEXT_DEPENDENT_SHAPE_REPRESENTATION ( #34147, #40589 ) ;
#1020 = AXIS2_PLACEMENT_3D ( 'NONE', #37359, #37842, #19459 ) ;
#1021 = CARTESIAN_POINT ( 'NONE',  ( 19.29194287201271862, -133.5026271600380880, -5.500000000000000000 ) ) ;
#1022 = AXIS2_PLACEMENT_3D ( 'NONE', #2617, #17562, #47432 ) ;
#1023 = ORIENTED_EDGE ( 'NONE', *, *, #15434, .F. ) ;
#1024 = CIRCLE ( 'NONE', #13552, 0.2999999999999981570 ) ;
#1025 = EDGE_CURVE ( 'NONE', #38548, #48127, #43741, .T. ) ;
#1026 = DIRECTION ( 'NONE',  ( -0.000000000000000000, -0.000000000000000000, -1.000000000000000000 ) ) ;
#1027 = VERTEX_POINT ( 'NONE', #25126 ) ;
#1028 = CIRCLE ( 'NONE', #30787, 82.00000000000000000 ) ;
#1029 = CARTESIAN_POINT ( 'NONE',  ( 0.000000000000000000, -16.65560815589439159, 38.55633173627004595 ) ) ;
#1030 = CYLINDRICAL_SURFACE ( 'NONE', #44594, 16.00000000000000000 ) ;
#1032 = ORIENTED_EDGE ( 'NONE', *, *, #24148, .T. ) ;
#1031 = CARTESIAN_POINT ( 'NONE',  ( 11.99999999999999822, 75.11725578898472122, -2.956366410619845730 ) ) ;
#1033 = EDGE_LOOP ( 'NONE', ( #40955, #9788, #11053, #10812 ) ) ;
#1034 = EDGE_CURVE ( 'NONE', #715, #25865, #46377, .T. ) ;
#1035 = EDGE_CURVE ( 'NONE', #37389, #41148, #14338, .T. ) ;
#1036 = EDGE_CURVE ( 'NONE', #43938, #40433, #32954, .T. ) ;
#1037 = DIRECTION ( 'NONE',  ( -1.000000000000000000, 0.000000000000000000, -0.000000000000000000 ) ) ;
#1038 = DIRECTION ( 'NONE',  ( 0.000000000000000000, 0.000000000000000000, 1.000000000000000000 ) ) ;
#1039 = CYLINDRICAL_SURFACE ( 'NONE', #12663, 77.49899999999999523 ) ;
#1040 = AXIS2_PLACEMENT_3D ( 'NONE', #40870, #18818, #15177 ) ;
#1042 = ORIENTED_EDGE ( 'NONE', *, *, #8061, .F. ) ;
#1041 = DIRECTION ( 'NONE',  ( 1.000000000000000000, 0.000000000000000000, 0.000000000000000000 ) ) ;
#1043 = ORIENTED_EDGE ( 'NONE', *, *, #44084, .F. ) ;
#1044 = CARTESIAN_POINT ( 'NONE',  ( 11.99999999999999822, 56.15606465355041621, -59.75363087400016582 ) ) ;
#1045 = ORIENTED_EDGE ( 'NONE', *, *, #3920, .T. ) ;
#1046 = VERTEX_POINT ( 'NONE', #7254 ) ;
#1047 = EDGE_CURVE ( 'NONE', #15687, #30366, #2369, .T. ) ;
#1048 = VECTOR ( 'NONE', #20936, 1000.000000000000000 ) ;
#1049 = LINE ( 'NONE', #11840, #21553 ) ;
#1050 = CIRCLE ( 'NONE', #26849, 82.00000000000000000 ) ;
#1051 = EDGE_LOOP ( 'NONE', ( #8665, #8541, #35186, #7160 ) ) ;
#1052 = CIRCLE ( 'NONE', #10463, 19.05560546998412974 ) ;
#1053 = LINE ( 'NONE', #30214, #3540 ) ;
#1054 = EDGE_CURVE ( 'NONE', #20071, #37949, #13540, .T. ) ;
#1055 = DIRECTION ( 'NONE',  ( 0.000000000000000000, 0.7071067811865489050, -0.7071067811865462405 ) ) ;
#1056 = CARTESIAN_POINT ( 'NONE',  ( 0.000000000000000000, -27.74655509720726343, 77.16300072079651784 ) ) ;
#1057 = ORIENTED_EDGE ( 'NONE', *, *, #29918, .F. ) ;
#1058 = DIRECTION ( 'NONE',  ( -1.000000000000000000, -0.000000000000000000, 0.000000000000000000 ) ) ;
#1059 = DIRECTION ( 'NONE',  ( 0.000000000000000000, 0.000000000000000000, 1.000000000000000000 ) ) ;
#1060 = DIRECTION ( 'NONE',  ( -1.000000000000000000, 0.000000000000000000, 0.000000000000000000 ) ) ;
#1061 = CARTESIAN_POINT ( 'NONE',  ( 11.99999999999999822, -36.73666225445845157, -65.58780272294114866 ) ) ;
#1062 = DIRECTION ( 'NONE',  ( 1.000000000000000000, 0.000000000000000000, 0.000000000000000000 ) ) ;
#1063 = VECTOR ( 'NONE', #13673, 1000.000000000000000 ) ;
#1064 = AXIS2_PLACEMENT_3D ( 'NONE', #19658, #43416, #17441 ) ;
#1065 = CARTESIAN_POINT ( 'NONE',  ( 10.00000000000000000, 0.000000000000000000, 0.000000000000000000 ) ) ;
#1066 = CARTESIAN_POINT ( 'NONE',  ( 0.000000000000000000, 75.54627589209943039, 17.28742895386112721 ) ) ;
#1067 = DIRECTION ( 'NONE',  ( 0.000000000000000000, 0.000000000000000000, 1.000000000000000000 ) ) ;
#1068 = VECTOR ( 'NONE', #42092, 1000.000000000000000 ) ;
#1069 = EDGE_CURVE ( 'NONE', #1265, #28940, #39365, .T. ) ;
#1070 = DIRECTION ( 'NONE',  ( 0.000000000000000000, 0.000000000000000000, 1.000000000000000000 ) ) ;
#1071 = CYLINDRICAL_SURFACE ( 'NONE', #19808, 12.50000000000000000 ) ;
#1072 = VECTOR ( 'NONE', #42654, 1000.000000000000000 ) ;
#1073 = ORIENTED_EDGE ( 'NONE', *, *, #12908, .T. ) ;
#1074 = ORIENTED_EDGE ( 'NONE', *, *, #30261, .F. ) ;
#1075 = CARTESIAN_POINT ( 'NONE',  ( 0.000000000000000000, 41.81611651403861885, 3.925862922256313503 ) ) ;
#1076 = DIRECTION ( 'NONE',  ( 0.000000000000000000, 0.000000000000000000, 1.000000000000000000 ) ) ;
#1077 = ORIENTED_EDGE ( 'NONE', *, *, #30969, .F. ) ;
#1078 = ORIENTED_EDGE ( 'NONE', *, *, #46239, .F. ) ;
#1079 = DIRECTION ( 'NONE',  ( -1.000000000000000000, 0.000000000000000000, -0.000000000000000000 ) ) ;
#1080 = VERTEX_POINT ( 'NONE', #36865 ) ;
#1081 = CIRCLE ( 'NONE', #30024, 42.00000000000000000 ) ;
#1082 = AXIS2_PLACEMENT_3D ( 'NONE', #14006, #36515, #13779 ) ;
#1083 = EDGE_CURVE ( 'NONE', #9308, #24221, #40129, .T. ) ;
#1084 = ORIENTED_EDGE ( 'NONE', *, *, #24140, .F. ) ;
#1085 = AXIS2_PLACEMENT_3D ( 'NONE', #8224, #22667, #30020 ) ;
#1086 = AXIS2_PLACEMENT_3D ( 'NONE', #36826, #38287, #19916 ) ;
#1087 = ADVANCED_FACE ( 'NONE', ( #43978, #17297, #32251, #21211, #40330, #14365, #36627, #36147, #6784, #21706, #21939, #17545, #3091, #47414, #18018, #47170, #44228 ), #2603, .F. ) ;
#1088 = ORIENTED_EDGE ( 'NONE', *, *, #25577, .T. ) ;
#1089 = ORIENTED_EDGE ( 'NONE', *, *, #1604, .T. ) ;
#1090 = EDGE_CURVE ( 'NONE', #29594, #25561, #7011, .T. ) ;
#1091 = AXIS2_PLACEMENT_3D ( 'NONE', #34675, #1411, #16107 ) ;
#1092 = AXIS2_PLACEMENT_3D ( 'NONE', #19598, #38229, #1007 ) ;
#1093 = CARTESIAN_POINT ( 'NONE',  ( 11.99999999999999822, -71.91182617369167929, -28.89263327155821059 ) ) ;
#1094 = VECTOR ( 'NONE', #31075, 1000.000000000000000 ) ;
#1095 = DIRECTION ( 'NONE',  ( 0.000000000000000000, 0.000000000000000000, 1.000000000000000000 ) ) ;
#1096 = AXIS2_PLACEMENT_3D ( 'NONE', #43302, #16385, #16157 ) ;
#1097 = DIRECTION ( 'NONE',  ( 0.000000000000000000, -0.9723699203976741146, -0.2334453638559158550 ) ) ;
#1098 = ORIENTED_EDGE ( 'NONE', *, *, #5630, .T. ) ;
#1099 = CARTESIAN_POINT ( 'NONE',  ( -10.90093335751250692, 0.000000000000000000, 0.000000000000000000 ) ) ;
#1100 = ORIENTED_EDGE ( 'NONE', *, *, #618, .T. ) ;
#1101 = VERTEX_POINT ( 'NONE', #11435 ) ;
#1102 = CIRCLE ( 'NONE', #45658, 31.99999999999999645 ) ;
#1103 = ADVANCED_FACE ( 'NONE', ( #30272 ), #41519, .T. ) ;
#1104 = ADVANCED_FACE ( 'NONE', ( #15345 ), #8223, .T. ) ;
#1105 = CARTESIAN_POINT ( 'NONE',  ( -1.459549131277904976, -119.6539995182286304, 2.500000000000000000 ) ) ;
#1106 = DIRECTION ( 'NONE',  ( -1.000000000000000000, -0.000000000000000000, -0.000000000000000000 ) ) ;
#1107 = DIRECTION ( 'NONE',  ( -1.000000000000000000, -0.000000000000000000, -0.000000000000000000 ) ) ;
#1108 = EDGE_LOOP ( 'NONE', ( #42456, #30771, #37756, #30253 ) ) ;
#1109 = ORIENTED_EDGE ( 'NONE', *, *, #34348, .F. ) ;
#1110 = DIRECTION ( 'NONE',  ( 0.9997280174009349762, -0.02332147558787674158, 0.000000000000000000 ) ) ;
#1111 = ORIENTED_EDGE ( 'NONE', *, *, #6339, .T. ) ;
#1112 = LINE ( 'NONE', #26822, #9011 ) ;
#1113 = CARTESIAN_POINT ( 'NONE',  ( 2.874421927457452952, -143.3717286177755739, 5.500000000000000000 ) ) ;
#1114 = LINE ( 'NONE', #18135, #7231 ) ;
#1115 = DIRECTION ( 'NONE',  ( -1.000000000000000000, 0.000000000000000000, 0.000000000000000000 ) ) ;
#1116 = DIRECTION ( 'NONE',  ( 0.000000000000000000, 0.000000000000000000, 1.000000000000000000 ) ) ;
#1117 = AXIS2_PLACEMENT_3D ( 'NONE', #40933, #34964, #15238 ) ;
#1118 = DIRECTION ( 'NONE',  ( 0.000000000000000000, 0.5877852522924685852, 0.8090169943749508930 ) ) ;
#1119 = CARTESIAN_POINT ( 'NONE',  ( 10.00000000000000000, -10.96151621346461447, -35.95386929396268272 ) ) ;
#1120 = CARTESIAN_POINT ( 'NONE',  ( 10.00000000000000000, 14.67089635893819377, -73.72996012237423713 ) ) ;
#1122 = LINE ( 'NONE', #23633, #13666 ) ;
#1121 = PRODUCT_DEFINITION ( 'UNKNOWN', '', #32690, #14935 ) ;
#1123 = DIRECTION ( 'NONE',  ( -1.000000000000000000, 0.000000000000000000, 0.000000000000000000 ) ) ;
#1124 = AXIS2_PLACEMENT_3D ( 'NONE', #13235, #28158, #27444 ) ;
#1125 = CARTESIAN_POINT ( 'NONE',  ( 0.000000000000000000, -3.925862922256468046, 41.81611651403860463 ) ) ;
#1126 = ORIENTED_EDGE ( 'NONE', *, *, #27531, .F. ) ;
#1127 = ORIENTED_EDGE ( 'NONE', *, *, #25941, .T. ) ;
#1128 = CARTESIAN_POINT ( 'NONE',  ( 10.00000000000000000, 0.000000000000000000, 0.000000000000000000 ) ) ;
#1129 = AXIS2_PLACEMENT_3D ( 'NONE', #7232, #11155, #3564 ) ;
#1130 = CIRCLE ( 'NONE', #35513, 16.00000000000000000 ) ;
#1131 = CARTESIAN_POINT ( 'NONE',  ( 11.99999999999999822, 8.830959090342393125, 74.65491531819122883 ) ) ;
#1132 = VECTOR ( 'NONE', #38496, 1000.000000000000000 ) ;
#1133 = DIRECTION ( 'NONE',  ( 0.000000000000000000, 1.000000000000000000, -9.787530781167596740E-16 ) ) ;
#1134 = CYLINDRICAL_SURFACE ( 'NONE', #8852, 32.00000000000000000 ) ;
#1135 = PLANE ( 'NONE',  #15388 ) ;
#1136 = DIRECTION ( 'NONE',  ( -1.000000000000000000, -0.000000000000000000, 0.000000000000000000 ) ) ;
#1137 = AXIS2_PLACEMENT_3D ( 'NONE', #6055, #21192, #2136 ) ;
#1138 = DIRECTION ( 'NONE',  ( -1.000000000000000000, -0.000000000000000000, 0.000000000000000000 ) ) ;
#1139 = DIRECTION ( 'NONE',  ( -0.000000000000000000, -0.3090169943749450088, 0.9510565162951543083 ) ) ;
#1140 = ORIENTED_EDGE ( 'NONE', *, *, #8337, .F. ) ;
#1141 = AXIS2_PLACEMENT_3D ( 'NONE', #1935, #20508, #43039 ) ;
#1142 = AXIS2_PLACEMENT_3D ( 'NONE', #18898, #7171, #48288 ) ;
#1143 =( NAMED_UNIT ( * ) PLANE_ANGLE_UNIT ( ) SI_UNIT ( $, .RADIAN. ) );
#1144 = CARTESIAN_POINT ( 'NONE',  ( 10.00000000000000000, -39.78640506895559525, -66.50666863322042843 ) ) ;
#1145 = CIRCLE ( 'NONE', #23016, 31.99999999999999645 ) ;
#1146 = ORIENTED_EDGE ( 'NONE', *, *, #27077, .F. ) ;
#1147 = VERTEX_POINT ( 'NONE', #11900 ) ;
#1148 = EDGE_CURVE ( 'NONE', #30085, #18493, #4073, .T. ) ;
#1149 = ORIENTED_EDGE ( 'NONE', *, *, #47202, .T. ) ;
#1150 = EDGE_CURVE ( 'NONE', #40355, #10383, #4177, .T. ) ;
#1151 = DIRECTION ( 'NONE',  ( -1.000000000000000000, 0.000000000000000000, 0.000000000000000000 ) ) ;
#1152 = ORIENTED_EDGE ( 'NONE', *, *, #6211, .T. ) ;
#1153 = EDGE_CURVE ( 'NONE', #46024, #36078, #21357, .T. ) ;
#1154 = ORIENTED_EDGE ( 'NONE', *, *, #22036, .F. ) ;
#1155 = AXIS2_PLACEMENT_3D ( 'NONE', #6083, #29721, #35918 ) ;
#1156 = DIRECTION ( 'NONE',  ( -1.000000000000000000, -0.000000000000000000, -0.000000000000000000 ) ) ;
#1157 = AXIS2_PLACEMENT_3D ( 'NONE', #25787, #14062, #26038 ) ;
#1158 = EDGE_CURVE ( 'NONE', #7124, #22172, #18982, .T. ) ;
#1159 = DIRECTION ( 'NONE',  ( 1.000000000000000000, -0.000000000000000000, -0.000000000000000000 ) ) ;
#1160 = EDGE_LOOP ( 'NONE', ( #13684, #21800, #27783, #5983 ) ) ;
#1161 = ORIENTED_EDGE ( 'NONE', *, *, #38046, .F. ) ;
#1162 = PRODUCT_DEFINITION_SHAPE ( 'NONE', 'NONE',  #48468 ) ;
#1163 = ADVANCED_FACE ( 'NONE', ( #7510 ), #44699, .T. ) ;
#1164 = EDGE_CURVE ( 'NONE', #6579, #913, #16687, .T. ) ;
#1165 = CYLINDRICAL_SURFACE ( 'NONE', #34218, 31.99999999999999289 ) ;
#1166 = DIRECTION ( 'NONE',  ( 0.000000000000000000, -0.1564344650402380854, 0.9876883405951365491 ) ) ;
#1167 = DIRECTION ( 'NONE',  ( 1.000000000000000000, 0.000000000000000000, 0.000000000000000000 ) ) ;
#1168 = AXIS2_PLACEMENT_3D ( 'NONE', #16765, #2531, #17466 ) ;
#1169 = CIRCLE ( 'NONE', #12893, 42.00000000000000000 ) ;
#1170 = ORIENTED_EDGE ( 'NONE', *, *, #42785, .F. ) ;
#1171 = DIRECTION ( 'NONE',  ( -1.000000000000000000, 0.000000000000000000, 0.000000000000000000 ) ) ;
#1172 = ADVANCED_FACE ( 'NONE', ( #11178 ), #37599, .T. ) ;
#1173 = ORIENTED_EDGE ( 'NONE', *, *, #17166, .T. ) ;
#1174 = EDGE_LOOP ( 'NONE', ( #32465, #41102, #15608, #21253 ) ) ;
#1175 = FACE_OUTER_BOUND ( 'NONE', #13442, .T. ) ;
#1176 = DIRECTION ( 'NONE',  ( 0.8774505977381983346, 0.4796670183876293736, 0.000000000000000000 ) ) ;
#1177 = ORIENTED_EDGE ( 'NONE', *, *, #36182, .T. ) ;
#1178 = VECTOR ( 'NONE', #30755, 1000.000000000000000 ) ;
#1179 = DIRECTION ( 'NONE',  ( -1.000000000000000000, 0.000000000000000000, -0.000000000000000000 ) ) ;
#1180 = DIRECTION ( 'NONE',  ( -1.000000000000000000, 0.000000000000000000, 0.000000000000000000 ) ) ;
#1181 = LINE ( 'NONE', #42793, #34588 ) ;
#1183 = VERTEX_POINT ( 'NONE', #26825 ) ;
#1182 = AXIS2_PLACEMENT_3D ( 'NONE', #36099, #2558, #37112 ) ;
#1184 = VECTOR ( 'NONE', #11769, 1000.000000000000000 ) ;
#1185 = ORIENTED_EDGE ( 'NONE', *, *, #40362, .F. ) ;
#1186 = FACE_OUTER_BOUND ( 'NONE', #12739, .T. ) ;
#1187 = EDGE_CURVE ( 'NONE', #16097, #10794, #33915, .T. ) ;
#1188 = DIRECTION ( 'NONE',  ( -1.000000000000000000, 0.000000000000000000, -0.000000000000000000 ) ) ;
#1189 = ORIENTED_EDGE ( 'NONE', *, *, #35205, .F. ) ;
#1190 = ORIENTED_EDGE ( 'NONE', *, *, #32089, .F. ) ;
#1191 = CARTESIAN_POINT ( 'NONE',  ( 10.00000000000000000, -27.75498641678720446, -31.52238457039628727 ) ) ;
#1192 = EDGE_LOOP ( 'NONE', ( #46128, #20788, #45078, #27773 ) ) ;
#1193 = LINE ( 'NONE', #27150, #21499 ) ;
#1194 = CARTESIAN_POINT ( 'NONE',  ( 11.99999999999999822, 0.000000000000000000, 0.000000000000000000 ) ) ;
#1195 = DIRECTION ( 'NONE',  ( -1.000000000000000000, -0.000000000000000000, 0.000000000000000000 ) ) ;
#1196 = VECTOR ( 'NONE', #44535, 1000.000000000000000 ) ;
#1197 = EDGE_LOOP ( 'NONE', ( #31822, #10125, #45167, #10166 ) ) ;
#1198 = CARTESIAN_POINT ( 'NONE',  ( 0.000000000000000000, 59.03342792756328095, -46.54456581323744757 ) ) ;
#1199 = ORIENTED_EDGE ( 'NONE', *, *, #4695, .T. ) ;
#1200 = CARTESIAN_POINT ( 'NONE',  ( 0.000000000000000000, 34.44570377933598593, 69.42325613327452061 ) ) ;
#1201 = CYLINDRICAL_SURFACE ( 'NONE', #10724, 31.99999999999999289 ) ;
#1202 = CIRCLE ( 'NONE', #19188, 31.99999999999998579 ) ;
#1203 = CARTESIAN_POINT ( 'NONE',  ( 10.00000000000000000, 30.00120703465236716, -22.64427369931138756 ) ) ;
#1204 = FACE_OUTER_BOUND ( 'NONE', #23258, .T. ) ;
#1205 = ORIENTED_EDGE ( 'NONE', *, *, #27577, .F. ) ;
#1206 = AXIS2_PLACEMENT_3D ( 'NONE', #14979, #37488, #45543 ) ;
#1207 = CARTESIAN_POINT ( 'NONE',  ( 21.07894319797337701, -103.8699611390234878, -5.500000000000000000 ) ) ;
#1208 =( NAMED_UNIT ( * ) PLANE_ANGLE_UNIT ( ) SI_UNIT ( $, .RADIAN. ) );
#1209 = ORIENTED_EDGE ( 'NONE', *, *, #5096, .T. ) ;
#1210 = ORIENTED_EDGE ( 'NONE', *, *, #1703, .T. ) ;
#1211 = VECTOR ( 'NONE', #20604, 1000.000000000000000 ) ;
#1212 = AXIS2_PLACEMENT_3D ( 'NONE', #4040, #47841, #6417 ) ;
#1213 = DIRECTION ( 'NONE',  ( 1.000000000000000000, 0.000000000000000000, 0.000000000000000000 ) ) ;
#1214 = VERTEX_POINT ( 'NONE', #142 ) ;
#1215 = EDGE_CURVE ( 'NONE', #19020, #41278, #26852, .T. ) ;
#1216 = CIRCLE ( 'NONE', #16076, 82.00000000000000000 ) ;
#1217 = CYLINDRICAL_SURFACE ( 'NONE', #28054, 82.00000000000000000 ) ;
#1218 = DIRECTION ( 'NONE',  ( -1.000000000000000000, 0.000000000000000000, 0.000000000000000000 ) ) ;
#1219 = EDGE_CURVE ( 'NONE', #15799, #16528, #41699, .T. ) ;
#1220 = AXIS2_PLACEMENT_3D ( 'NONE', #45133, #44166, #37055 ) ;
#1221 = ORIENTED_EDGE ( 'NONE', *, *, #12348, .F. ) ;
#1222 = ADVANCED_FACE ( 'NONE', ( #19239 ), #15566, .T. ) ;
#1223 = CIRCLE ( 'NONE', #4347, 31.99999999999999289 ) ;
#1224 = EDGE_CURVE ( 'NONE', #4717, #6044, #41761, .T. ) ;
#1225 = EDGE_CURVE ( 'NONE', #39044, #16230, #45604, .T. ) ;
#1226 = SHAPE_REPRESENTATION ( 'output shaft', ( #11636 ), #38234 ) ;
#1227 = DIRECTION ( 'NONE',  ( 0.000000000000000000, 0.6691306063588579045, -0.7431448254773945772 ) ) ;
#1228 = ORIENTED_EDGE ( 'NONE', *, *, #26320, .T. ) ;
#1229 = ORIENTED_EDGE ( 'NONE', *, *, #3126, .T. ) ;
#1230 = CIRCLE ( 'NONE', #23908, 31.99999999999999289 ) ;
#1231 = ORIENTED_EDGE ( 'NONE', *, *, #45937, .T. ) ;
#1232 = VECTOR ( 'NONE', #47384, 1000.000000000000000 ) ;
#1233 = EDGE_CURVE ( 'NONE', #2023, #43990, #3585, .T. ) ;
#1234 = AXIS2_PLACEMENT_3D ( 'NONE', #9549, #35983, #13242 ) ;
#1235 = CARTESIAN_POINT ( 'NONE',  ( 10.00000000000000000, 0.000000000000000000, 0.000000000000000000 ) ) ;
#1236 = VERTEX_POINT ( 'NONE', #14851 ) ;
#1237 = CARTESIAN_POINT ( 'NONE',  ( -2.977765906491215642, 0.000000000000000000, -15.39727592589476579 ) ) ;
#1238 = EDGE_CURVE ( 'NONE', #40188, #24194, #34617, .T. ) ;
#1239 = ORIENTED_EDGE ( 'NONE', *, *, #15759, .F. ) ;
#1240 = CARTESIAN_POINT ( 'NONE',  ( 0.000000000000000000, -75.16055320797016748, -18.89407956138335365 ) ) ;
#1241 = DIRECTION ( 'NONE',  ( -1.000000000000000000, 0.000000000000000000, 0.000000000000000000 ) ) ;
#1242 = CARTESIAN_POINT ( 'NONE',  ( 4.999999999999999112, -41.81611651403864727, 3.925862922256025289 ) ) ;
#1243 = ORIENTED_EDGE ( 'NONE', *, *, #34817, .T. ) ;
#1244 = DIRECTION ( 'NONE',  ( -1.000000000000000000, -0.000000000000000000, -0.000000000000000000 ) ) ;
#1245 = ORIENTED_EDGE ( 'NONE', *, *, #43663, .T. ) ;
#1246 = DIRECTION ( 'NONE',  ( 0.000000000000000000, 0.000000000000000000, 1.000000000000000000 ) ) ;
#1247 = ADVANCED_FACE ( 'NONE', ( #5038 ), #27809, .T. ) ;
#1248 = CARTESIAN_POINT ( 'NONE',  ( -6.170112525937310188, 10.87104923258429068, 125.0000000000000000 ) ) ;
#1249 = AXIS2_PLACEMENT_3D ( 'NONE', #32536, #21027, #13697 ) ;
#1250 = EDGE_LOOP ( 'NONE', ( #31034, #1486, #9936, #25997 ) ) ;
#1251 = LINE ( 'NONE', #31604, #45966 ) ;
#1252 = ORIENTED_EDGE ( 'NONE', *, *, #38710, .F. ) ;
#1253 = ORIENTED_EDGE ( 'NONE', *, *, #14819, .F. ) ;
#1254 = CARTESIAN_POINT ( 'NONE',  ( 10.00000000000000000, -37.22597642581153821, -5.202137450156795850 ) ) ;
#1255 = DIRECTION ( 'NONE',  ( -1.000000000000000000, -0.000000000000000000, -0.000000000000000000 ) ) ;
#1256 = FACE_OUTER_BOUND ( 'NONE', #41126, .T. ) ;
#1257 = VECTOR ( 'NONE', #6911, 1000.000000000000000 ) ;
#1258 = LINE ( 'NONE', #997, #32148 ) ;
#1259 = DIRECTION ( 'NONE',  ( 1.000000000000000000, 0.000000000000000000, 0.000000000000000000 ) ) ;
#1260 = AXIS2_PLACEMENT_3D ( 'NONE', #16246, #12806, #42175 ) ;
#1261 = CARTESIAN_POINT ( 'NONE',  ( 0.000000000000000000, 0.000000000000000000, 0.000000000000000000 ) ) ;
#1262 = CARTESIAN_POINT ( 'NONE',  ( 10.00000000000000000, 0.000000000000000000, 0.000000000000000000 ) ) ;
#1263 = DIRECTION ( 'NONE',  ( 0.000000000000000000, 0.8910065241883656784, 0.4539904997395511344 ) ) ;
#1264 = EDGE_CURVE ( 'NONE', #16392, #35973, #42970, .T. ) ;
#1265 = VERTEX_POINT ( 'NONE', #6423 ) ;
#1266 = AXIS2_PLACEMENT_3D ( 'NONE', #25808, #44665, #11863 ) ;
#1267 = CARTESIAN_POINT ( 'NONE',  ( -2.499999999999997780, 8.494897427831771708, -19.01812422950394676 ) ) ;
#1268 = DIRECTION ( 'NONE',  ( -1.000000000000000000, 0.000000000000000000, 0.000000000000000000 ) ) ;
#1269 = PLANE ( 'NONE',  #48175 ) ;
#1270 = CIRCLE ( 'NONE', #2826, 37.49900000000000233 ) ;
#1271 = DIRECTION ( 'NONE',  ( 0.000000000000000000, -0.3090169943749461745, 0.9510565162951539753 ) ) ;
#1272 = CARTESIAN_POINT ( 'NONE',  ( -2.981742216678212820, 0.000000000000000000, 15.39727592608509177 ) ) ;
#1273 =( LENGTH_UNIT ( ) NAMED_UNIT ( * ) SI_UNIT ( .MILLI., .METRE. ) );
#1274 = AXIS2_PLACEMENT_3D ( 'NONE', #31416, #5223, #23810 ) ;
#1275 = CARTESIAN_POINT ( 'NONE',  ( 0.000000000000000000, 20.85821328998756385, -10.92862929874494959 ) ) ;
#1276 = ORIENTED_EDGE ( 'NONE', *, *, #12127, .F. ) ;
#1277 = VERTEX_POINT ( 'NONE', #16782 ) ;
#1278 = AXIS2_PLACEMENT_3D ( 'NONE', #25443, #22741, #38164 ) ;
#1279 = FACE_OUTER_BOUND ( 'NONE', #14037, .T. ) ;
#1280 = ORIENTED_EDGE ( 'NONE', *, *, #21742, .F. ) ;
#1281 = EDGE_CURVE ( 'NONE', #3891, #9834, #46158, .T. ) ;
#1282 = LINE ( 'NONE', #16217, #3372 ) ;
#1283 = APPLICATION_PROTOCOL_DEFINITION ( 'draft international standard', 'automotive_design', 1998, #28226 ) ;
#1284 = CARTESIAN_POINT ( 'NONE',  ( 11.99999999999999822, -44.88180994100329713, -63.18004540533077318 ) ) ;
#1285 = AXIS2_PLACEMENT_3D ( 'NONE', #2106, #31249, #17021 ) ;
#1286 = VERTEX_POINT ( 'NONE', #12623 ) ;
#1287 = EDGE_CURVE ( 'NONE', #4413, #25450, #37700, .T. ) ;
#1288 = AXIS2_PLACEMENT_3D ( 'NONE', #684, #1171, #23680 ) ;
#1289 = EDGE_CURVE ( 'NONE', #18460, #24623, #27553, .T. ) ;
#1290 = CYLINDRICAL_SURFACE ( 'NONE', #13658, 82.00000000000000000 ) ;
#1291 = AXIS2_PLACEMENT_3D ( 'NONE', #24020, #34057, #4922 ) ;
#1292 = ORIENTED_EDGE ( 'NONE', *, *, #44650, .T. ) ;
#1293 = CYLINDRICAL_SURFACE ( 'NONE', #38311, 82.00000000000000000 ) ;
#1294 = DIRECTION ( 'NONE',  ( 0.000000000000000000, 0.000000000000000000, 1.000000000000000000 ) ) ;
#1295 = VERTEX_POINT ( 'NONE', #5517 ) ;
#1296 = AXIS2_PLACEMENT_3D ( 'NONE', #32032, #29723, #44658 ) ;
#1297 = LINE ( 'NONE', #39215, #33 ) ;
#1298 = VERTEX_POINT ( 'NONE', #21338 ) ;
#1300 = ORIENTED_EDGE ( 'NONE', *, *, #4039, .F. ) ;
#1299 = LINE ( 'NONE', #311, #9038 ) ;
#1301 = EDGE_LOOP ( 'NONE', ( #26832, #25489, #4890, #25246 ) ) ;
#1302 = AXIS2_PLACEMENT_3D ( 'NONE', #45858, #8870, #25484 ) ;
#1303 = CARTESIAN_POINT ( 'NONE',  ( 0.000000000000000000, 3.925862922256160736, 41.81611651403863306 ) ) ;
#1304 = CARTESIAN_POINT ( 'NONE',  ( 0.000000000000000000, -30.84782396557201878, -21.32104025579148399 ) ) ;
#1305 = DIRECTION ( 'NONE',  ( 0.000000000000000000, 0.3090169943749480064, -0.9510565162951534202 ) ) ;
#1306 = DIRECTION ( 'NONE',  ( -1.000000000000000000, 0.000000000000000000, -0.000000000000000000 ) ) ;
#1307 = CARTESIAN_POINT ( 'NONE',  ( 0.000000000000000000, 0.000000000000000000, 0.000000000000000000 ) ) ;
#1308 = ORIENTED_EDGE ( 'NONE', *, *, #5264, .F. ) ;
#1309 = CARTESIAN_POINT ( 'NONE',  ( 10.00000000000000000, 46.21855187248719687, -62.20884554313968806 ) ) ;
#1310 = VERTEX_POINT ( 'NONE', #46646 ) ;
#1311 = VERTEX_POINT ( 'NONE', #25009 ) ;
#1312 = CARTESIAN_POINT ( 'NONE',  ( 0.000000000000000000, 5.256550761633951296, -77.32052557432835727 ) ) ;
#1313 = ORIENTED_EDGE ( 'NONE', *, *, #44195, .F. ) ;
#1314 = CARTESIAN_POINT ( 'NONE',  ( 10.00000000000000000, 0.000000000000000000, 0.000000000000000000 ) ) ;
#1315 = CARTESIAN_POINT ( 'NONE',  ( 10.00000000000000000, -17.67226234102849958, 33.17418723428301774 ) ) ;
#1316 = DIRECTION ( 'NONE',  ( -1.000000000000000000, 0.000000000000000000, 0.000000000000000000 ) ) ;
#1317 = VERTEX_POINT ( 'NONE', #20431 ) ;
#1318 = CARTESIAN_POINT ( 'NONE',  ( 0.000000000000000000, 0.000000000000000000, 0.000000000000000000 ) ) ;
#1319 = CARTESIAN_POINT ( 'NONE',  ( 5.000000000000002665, -74.18225833017913828, 34.94270380257611919 ) ) ;
#1320 = CARTESIAN_POINT ( 'NONE',  ( -10.00000000000000000, 0.000000000000000000, 0.000000000000000000 ) ) ;
#1321 = DIRECTION ( 'NONE',  ( -1.000000000000000000, 0.000000000000000000, -0.000000000000000000 ) ) ;
#1322 = DIRECTION ( 'NONE',  ( 0.000000000000000000, -0.4539904997395350916, -0.8910065241883738940 ) ) ;
#1323 = VECTOR ( 'NONE', #45414, 1000.000000000000000 ) ;
#1324 = CARTESIAN_POINT ( 'NONE',  ( 0.000000000000000000, -55.19960302592104284, 51.03279382321070301 ) ) ;
#1325 = FACE_OUTER_BOUND ( 'NONE', #41133, .T. ) ;
#1326 = DIRECTION ( 'NONE',  ( 0.000000000000000000, 0.000000000000000000, -1.000000000000000000 ) ) ;
#1327 = AXIS2_PLACEMENT_3D ( 'NONE', #22740, #4153, #19068 ) ;
#1328 = DIRECTION ( 'NONE',  ( 0.000000000000000000, 0.3090169943749573878, -0.9510565162951503115 ) ) ;
#1329 = DIRECTION ( 'NONE',  ( -0.000000000000000000, 0.000000000000000000, 1.000000000000000000 ) ) ;
#1330 = VERTEX_POINT ( 'NONE', #16061 ) ;
#1331 = ORIENTED_EDGE ( 'NONE', *, *, #47345, .T. ) ;
#1332 = EDGE_CURVE ( 'NONE', #12095, #23501, #35123, .T. ) ;
#1333 = CARTESIAN_POINT ( 'NONE',  ( 5.000000000000000000, 39.04073710021366139, -15.48615015657542138 ) ) ;
#1334 = CIRCLE ( 'NONE', #24007, 31.99999999999998579 ) ;
#1335 = ORIENTED_EDGE ( 'NONE', *, *, #38814, .F. ) ;
#1336 = EDGE_LOOP ( 'NONE', ( #24915, #24539, #28080, #17825 ) ) ;
#1337 = EDGE_CURVE ( 'NONE', #36518, #44508, #19728, .T. ) ;
#1338 = DIRECTION ( 'NONE',  ( -1.000000000000000000, -0.000000000000000000, 0.000000000000000000 ) ) ;
#1339 = ADVANCED_FACE ( 'NONE', ( #12388 ), #35368, .F. ) ;
#1340 = AXIS2_PLACEMENT_3D ( 'NONE', #28538, #38843, #47128 ) ;
#1341 = CARTESIAN_POINT ( 'NONE',  ( 0.000000000000000000, -73.73191006444561424, -14.66109333815538918 ) ) ;
#1342 = EDGE_LOOP ( 'NONE', ( #36126, #36973, #5943, #20745 ) ) ;
#1343 = AXIS2_PLACEMENT_3D ( 'NONE', #35872, #24626, #2337 ) ;
#1344 = EDGE_CURVE ( 'NONE', #45431, #43260, #12727, .T. ) ;
#1346 = ADVANCED_FACE ( 'NONE', ( #39959 ), #1370, .T. ) ;
#1345 = VERTEX_POINT ( 'NONE', #5286 ) ;
#1347 = EDGE_LOOP ( 'NONE', ( #24405, #19869, #14111, #4047 ) ) ;
#1348 = EDGE_LOOP ( 'NONE', ( #15991, #38347, #37593, #28798 ) ) ;
#1349 = CIRCLE ( 'NONE', #20109, 37.49900000000000944 ) ;
#1350 = DIRECTION ( 'NONE',  ( 0.000000000000000000, 0.000000000000000000, 1.000000000000000000 ) ) ;
#1351 = DIRECTION ( 'NONE',  ( -0.000000000000000000, -0.000000000000000000, -1.000000000000000000 ) ) ;
#1353 = ORIENTED_EDGE ( 'NONE', *, *, #38597, .F. ) ;
#1352 = DIRECTION ( 'NONE',  ( -1.000000000000000000, 0.000000000000000000, 0.000000000000000000 ) ) ;
#1354 = ORIENTED_EDGE ( 'NONE', *, *, #41018, .T. ) ;
#1355 = VECTOR ( 'NONE', #38110, 1000.000000000000000 ) ;
#1356 = PLANE ( 'NONE',  #32 ) ;
#1357 = VERTEX_POINT ( 'NONE', #16298 ) ;
#1358 = ORIENTED_EDGE ( 'NONE', *, *, #47675, .T. ) ;
#1359 = ORIENTED_EDGE ( 'NONE', *, *, #3672, .F. ) ;
#1360 = CARTESIAN_POINT ( 'NONE',  ( 0.000000000000000000, 0.000000000000000000, -2.500000000000000000 ) ) ;
#1361 = DIRECTION ( 'NONE',  ( -0.9997280174009349762, 0.02332147558787674504, 0.000000000000000000 ) ) ;
#1362 = DIRECTION ( 'NONE',  ( -1.000000000000000000, 0.000000000000000000, 0.000000000000000000 ) ) ;
#1363 = ORIENTED_EDGE ( 'NONE', *, *, #20315, .T. ) ;
#1364 = CIRCLE ( 'NONE', #16222, 37.49900000000000233 ) ;
#1365 = ORIENTED_EDGE ( 'NONE', *, *, #31617, .T. ) ;
#1366 = LINE ( 'NONE', #16294, #2088 ) ;
#1367 = ORIENTED_EDGE ( 'NONE', *, *, #14530, .T. ) ;
#1368 = CARTESIAN_POINT ( 'NONE',  ( -3.000000000000000000, -26.23277895567251505, 4.042438405569750870 ) ) ;
#1369 = DIRECTION ( 'NONE',  ( -1.000000000000000000, -0.000000000000000000, 0.000000000000000000 ) ) ;
#1370 = CYLINDRICAL_SURFACE ( 'NONE', #43195, 31.99999999999999289 ) ;
#1371 = CARTESIAN_POINT ( 'NONE',  ( 10.00000000000000000, 0.000000000000000000, 0.000000000000000000 ) ) ;
#1372 = CARTESIAN_POINT ( 'NONE',  ( 0.000000000000000000, 0.000000000000000000, 0.000000000000000000 ) ) ;
#1373 = CARTESIAN_POINT ( 'NONE',  ( 10.00000000000000000, 55.20638768913831029, -51.02545421589267960 ) ) ;
#1374 = CARTESIAN_POINT ( 'NONE',  ( 11.99999999999999822, -55.16347631942997509, -60.67117009219195722 ) ) ;
#1375 = ORIENTED_EDGE ( 'NONE', *, *, #6520, .T. ) ;
#1376 = DIRECTION ( 'NONE',  ( 1.000000000000000000, 0.000000000000000000, 0.000000000000000000 ) ) ;
#1377 = DIRECTION ( 'NONE',  ( 0.000000000000000000, 0.000000000000000000, 1.000000000000000000 ) ) ;
#1378 = AXIS2_PLACEMENT_3D ( 'NONE', #14927, #11262, #26189 ) ;
#1379 = DIRECTION ( 'NONE',  ( 0.000000000000000000, 0.000000000000000000, 1.000000000000000000 ) ) ;
#1380 = CARTESIAN_POINT ( 'NONE',  ( 10.00000000000000000, -66.50666863321973210, -39.78640506895676765 ) ) ;
#1381 = ADVANCED_FACE ( 'NONE', ( #38826 ), #8689, .T. ) ;
#1382 = ORIENTED_EDGE ( 'NONE', *, *, #44642, .T. ) ;
#1383 = FACE_OUTER_BOUND ( 'NONE', #39454, .T. ) ;
#1384 = EDGE_CURVE ( 'NONE', #15972, #17779, #966, .T. ) ;
#1385 = DIRECTION ( 'NONE',  ( 0.000000000000000000, 0.000000000000000000, 1.000000000000000000 ) ) ;
#1386 = CARTESIAN_POINT ( 'NONE',  ( 10.00000000000000000, 70.53064760720278059, 26.01480285779964774 ) ) ;
#1387 = CARTESIAN_POINT ( 'NONE',  ( 5.000000000000000000, 22.48208911017500355, 35.47612816024530957 ) ) ;
#1388 = ADVANCED_FACE ( 'NONE', ( #23626 ), #38573, .F. ) ;
#1389 = DIRECTION ( 'NONE',  ( -0.000000000000000000, -0.000000000000000000, -1.000000000000000000 ) ) ;
#1390 = DIRECTION ( 'NONE',  ( 0.000000000000000000, 0.000000000000000000, 1.000000000000000000 ) ) ;
#1391 = VECTOR ( 'NONE', #38209, 1000.000000000000000 ) ;
#1392 = CYLINDRICAL_SURFACE ( 'NONE', #37281, 42.00000000000000000 ) ;
#1393 = CARTESIAN_POINT ( 'NONE',  ( 0.000000000000000000, -20.41045688087772092, -72.35160999960838524 ) ) ;
#1394 = ORIENTED_EDGE ( 'NONE', *, *, #24254, .F. ) ;
#1395 = VECTOR ( 'NONE', #46062, 1000.000000000000000 ) ;
#1396 = ORIENTED_EDGE ( 'NONE', *, *, #18111, .T. ) ;
#1397 = EDGE_CURVE ( 'NONE', #5571, #4001, #1114, .T. ) ;
#1398 = SHAPE_REPRESENTATION_RELATIONSHIP ( 'NONE' , 'NONE' ,  #45973, #29206 ) ;
#1399 = CARTESIAN_POINT ( 'NONE',  ( 0.000000000000000000, 75.16055320797057959, -18.89407956138176914 ) ) ;
#1400 = ORIENTED_EDGE ( 'NONE', *, *, #442, .F. ) ;
#1401 = ADVANCED_FACE ( 'NONE', ( #33077 ), #25974, .F. ) ;
#1402 = EDGE_CURVE ( 'NONE', #39822, #36554, #3210, .T. ) ;
#1403 = ORIENTED_EDGE ( 'NONE', *, *, #15375, .F. ) ;
#1404 = VECTOR ( 'NONE', #12182, 1000.000000000000000 ) ;
#1405 = ORIENTED_EDGE ( 'NONE', *, *, #27096, .F. ) ;
#1406 = EDGE_LOOP ( 'NONE', ( #44187, #851, #16151, #32013, #39258, #34914, #30211, #46182, #40253, #8744, #32601, #5738, #8437, #35308, #6785, #38820, #24635, #22335, #27916, #10075, #21931, #10575, #10917, #31410, #35401, #42530, #37969, #35902, #18172, #45179, #15217, #38139, #2520, #22701, #38439, #8650, #22176, #10980, #39985, #39632, #21189, #10177, #31778, #13615, #23126, #8998, #8605, #12486, #15270, #5758, #3556, #41046, #35219, #13981, #10814, #45251, #38015, #8989, #38322, #2957, #12835, #40110, #33377, #9015, #45132, #6446, #4060, #15543, #9713, #1923, #4974, #33948, #15557, #27433, #21991, #28211, #52, #19143, #20680, #16400, #16233, #37415, #47232, #22432, #5609, #34863, #43006, #18752, #2227, #12909, #20265, #35784, #12863, #40893, #48244, #32237, #10185, #20021, #45773, #4169, #21994, #42387, #35733, #20224, #41583, #7616, #3436, #3522, #21144, #31096, #29873, #21909, #17178, #17236, #42591, #44308, #27167, #3327, #19540, #17304, #43273, #34334, #29486, #13292, #27427, #17646, #36750, #39250, #41550, #23205, #3793, #29281, #21740, #14756, #25667, #14435, #43677, #17361, #5963, #47909, #32224, #12785, #25008, #3249, #5193, #18962, #15611, #39659, #27866, #30437, #29122, #22529, #45861, #31420, #34746, #13562, #43320, #23452, #41438, #27595, #43642, #42857, #46772, #2329, #25702, #23015, #13375, #11440, #13834, #23374, #27108, #34189, #48182, #13153, #8350, #1292, #25597, #6814, #5051, #4185, #18557, #26961, #34078, #47806, #24936, #26171, #27864, #22320, #48119, #35177, #7749, #35771, #21924, #8386, #18950, #33971, #11547, #42895, #41553, #21025, #48297, #46749, #29219, #45568, #13093, #15648, #12008, #28289, #41325, #32133, #39831, #6166, #31150, #46038, #23029, #5694, #14557, #32226, #38031, #28574, #27546, #38603, #38285, #47085, #14334, #538, #26280, #47847, #43799, #46236, #30265, #14582, #1359, #7623, #31518, #9229, #36770, #29130, #33937, #19383, #24383, #31117, #22046, #44473, #39655, #38538, #44655, #8658, #35914, #6126, #15622, #34153, #32377, #14827, #36259, #28610, #9630, #37227, #43660, #38733, #42207, #38358, #15482, #38016, #28009, #40050, #41624, #28653, #31105, #27545, #30597, #12499, #580, #41162, #20176, #47738, #4392, #44224, #47633, #32763, #22225, #21557, #8287, #21504, #30030, #3982, #19693, #23475, #42162, #31218, #16215, #23747, #18849, #35352, #16331, #28310, #34223, #43490, #37156, #34270, #12944, #7350, #43908, #31896, #18607, #13835, #36970, #25423, #27906, #36056, #29474, #47968, #43467, #26638, #19232, #37050, #35035, #17266, #10825, #28885, #42300, #45745, #5527, #43446, #30053 ) ) ;
#1407 = CARTESIAN_POINT ( 'NONE',  ( 11.59999999999999787, 1.420590287010929336E-15, 40.80000000000001847 ) ) ;
#1408 = ORIENTED_EDGE ( 'NONE', *, *, #3201, .T. ) ;
#1409 = ORIENTED_EDGE ( 'NONE', *, *, #931, .T. ) ;
#1410 = CARTESIAN_POINT ( 'NONE',  ( 10.00000000000000000, -51.03279382321125723, 55.19960302592048862 ) ) ;
#1412 = VERTEX_POINT ( 'NONE', #15225 ) ;
#1411 = DIRECTION ( 'NONE',  ( -1.000000000000000000, 0.000000000000000000, 0.000000000000000000 ) ) ;
#1413 = ORIENTED_EDGE ( 'NONE', *, *, #26432, .T. ) ;
#1414 = ORIENTED_EDGE ( 'NONE', *, *, #47268, .F. ) ;
#1415 = CYLINDRICAL_SURFACE ( 'NONE', #42874, 77.49899999999999523 ) ;
#1417 = ORIENTED_EDGE ( 'NONE', *, *, #20509, .T. ) ;
#1416 = DIRECTION ( 'NONE',  ( 0.000000000000000000, 0.000000000000000000, 1.000000000000000000 ) ) ;
#1418 = AXIS2_PLACEMENT_3D ( 'NONE', #30277, #10937, #45196 ) ;
#1419 = LINE ( 'NONE', #8503, #29009 ) ;
#1420 = VERTEX_POINT ( 'NONE', #6899 ) ;
#1421 = DIRECTION ( 'NONE',  ( -1.000000000000000000, 0.000000000000000000, -0.000000000000000000 ) ) ;
#1422 = ORIENTED_EDGE ( 'NONE', *, *, #10339, .F. ) ;
#1423 = VERTEX_POINT ( 'NONE', #33566 ) ;
#1424 = DIRECTION ( 'NONE',  ( -1.000000000000000000, 0.000000000000000000, -0.000000000000000000 ) ) ;
#1425 = DIRECTION ( 'NONE',  ( -0.000000000000000000, -0.9135454576426004225, -0.4067366430758009854 ) ) ;
#1426 = ORIENTED_EDGE ( 'NONE', *, *, #26746, .F. ) ;
#1427 = AXIS2_PLACEMENT_3D ( 'NONE', #7158, #290, #22077 ) ;
#1428 = CARTESIAN_POINT ( 'NONE',  ( -10.00000000000000000, 0.000000000000000000, 0.000000000000000000 ) ) ;
#1429 = DIRECTION ( 'NONE',  ( -1.000000000000000000, -0.000000000000000000, -0.000000000000000000 ) ) ;
#1430 = CARTESIAN_POINT ( 'NONE',  ( 10.00000000000000000, -29.01471420065507090, -76.69515212746047439 ) ) ;
#1431 = CIRCLE ( 'NONE', #28779, 37.49900000000000233 ) ;
#1432 = ORIENTED_EDGE ( 'NONE', *, *, #14859, .T. ) ;
#1433 = ORIENTED_EDGE ( 'NONE', *, *, #32119, .T. ) ;
#1434 = ADVANCED_FACE ( 'NONE', ( #44580 ), #3461, .T. ) ;
#1435 = DIRECTION ( 'NONE',  ( 1.000000000000000000, 0.000000000000000000, -0.000000000000000000 ) ) ;
#1436 = DIRECTION ( 'NONE',  ( -1.000000000000000000, -0.000000000000000000, 0.000000000000000000 ) ) ;
#1437 = EDGE_CURVE ( 'NONE', #45989, #31737, #23, .T. ) ;
#1438 = ORIENTED_EDGE ( 'NONE', *, *, #17894, .T. ) ;
#1439 = DIRECTION ( 'NONE',  ( 1.000000000000000000, 0.000000000000000000, -0.000000000000000000 ) ) ;
#1440 = ORIENTED_EDGE ( 'NONE', *, *, #24709, .T. ) ;
#1441 = EDGE_CURVE ( 'NONE', #44170, #42578, #43955, .T. ) ;
#1442 = CARTESIAN_POINT ( 'NONE',  ( 10.00000000000000000, 0.000000000000000000, 77.49899999999999523 ) ) ;
#1443 = LINE ( 'NONE', #16366, #8344 ) ;
#1444 = DIRECTION ( 'NONE',  ( 0.4796670183876317051, -0.8774505977381971134, 0.000000000000000000 ) ) ;
#1445 = CARTESIAN_POINT ( 'NONE',  ( 5.000000000000002665, -39.47590169984793818, -71.87247863392457248 ) ) ;
#1446 = EDGE_CURVE ( 'NONE', #11961, #15589, #10350, .T. ) ;
#1447 = CARTESIAN_POINT ( 'NONE',  ( 0.000000000000000000, -10.45096189432314837, -21.10159698893440350 ) ) ;
#1448 = AXIS2_PLACEMENT_3D ( 'NONE', #40226, #48276, #37264 ) ;
#1449 = DIRECTION ( 'NONE',  ( -1.000000000000000000, 0.000000000000000000, 0.000000000000000000 ) ) ;
#1450 = DIRECTION ( 'NONE',  ( 0.000000000000000000, 0.7604059656000322631, -0.6494480483301821039 ) ) ;
#1451 = DIRECTION ( 'NONE',  ( 0.2867529058022035837, -0.9580045777625452175, 0.000000000000000000 ) ) ;
#1452 = ORIENTED_EDGE ( 'NONE', *, *, #17838, .T. ) ;
#1453 = LINE ( 'NONE', #23715, #23723 ) ;
#1454 = SURFACE_STYLE_FILL_AREA ( #43295 ) ;
#1455 = EDGE_CURVE ( 'NONE', #34210, #38706, #2977, .T. ) ;
#1456 = EDGE_CURVE ( 'NONE', #36858, #6225, #7138, .T. ) ;
#1457 = ORIENTED_EDGE ( 'NONE', *, *, #5577, .T. ) ;
#1458 = CARTESIAN_POINT ( 'NONE',  ( 4.250000000000000000, -13.95926121303099343, -1.199999999999999956 ) ) ;
#1459 = VERTEX_POINT ( 'NONE', #18397 ) ;
#1460 = AXIS2_PLACEMENT_3D ( 'NONE', #27869, #27135, #4849 ) ;
#1461 = ORIENTED_EDGE ( 'NONE', *, *, #27036, .T. ) ;
#1462 = CARTESIAN_POINT ( 'NONE',  ( 5.000000000000002665, 68.55367621811205936, -44.99326035065983120 ) ) ;
#1463 = LINE ( 'NONE', #24697, #23786 ) ;
#1464 = EDGE_LOOP ( 'NONE', ( #6655, #44629, #28449, #47036 ) ) ;
#1465 = ADVANCED_FACE ( 'NONE', ( #22057 ), #36988, .T. ) ;
#1466 = ORIENTED_EDGE ( 'NONE', *, *, #41177, .F. ) ;
#1467 = CARTESIAN_POINT ( 'NONE',  ( 6.938893903907228378E-15, 0.000000000000000000, 0.000000000000000000 ) ) ;
#1468 = VERTEX_POINT ( 'NONE', #36512 ) ;
#1469 = VERTEX_POINT ( 'NONE', #21595 ) ;
#1470 = VERTEX_POINT ( 'NONE', #33793 ) ;
#1471 = ORIENTED_EDGE ( 'NONE', *, *, #23150, .F. ) ;
#1472 = COLOUR_RGB ( '', 0.72549020, 0.75294118, 0.79215686) ;
#1473 = LINE ( 'NONE', #39401, #40711 ) ;
#1474 = VERTEX_POINT ( 'NONE', #33330 ) ;
#1475 = ORIENTED_EDGE ( 'NONE', *, *, #34688, .F. ) ;
#1476 = CARTESIAN_POINT ( 'NONE',  ( 11.99999999999999822, -46.11716303203233736, 67.80270845531873647 ) ) ;
#1477 = ORIENTED_EDGE ( 'NONE', *, *, #25577, .F. ) ;
#1478 = FACE_OUTER_BOUND ( 'NONE', #8267, .T. ) ;
#1479 = LINE ( 'NONE', #43078, #28583 ) ;
#1480 = CARTESIAN_POINT ( 'NONE',  ( 0.000000000000000000, 75.16055320797030959, 18.89407956138283851 ) ) ;
#1481 = ORIENTED_EDGE ( 'NONE', *, *, #42174, .F. ) ;
#1482 = FACE_OUTER_BOUND ( 'NONE', #12691, .T. ) ;
#1483 = ORIENTED_EDGE ( 'NONE', *, *, #6543, .F. ) ;
#1484 = CARTESIAN_POINT ( 'NONE',  ( 11.99999999999999822, 0.000000000000000000, 0.000000000000000000 ) ) ;
#1485 = DIRECTION ( 'NONE',  ( -1.000000000000000000, 0.000000000000000000, -0.000000000000000000 ) ) ;
#1486 = ORIENTED_EDGE ( 'NONE', *, *, #41177, .T. ) ;
#1487 = DIRECTION ( 'NONE',  ( -0.000000000000000000, 0.4067366430758000417, -0.9135454576426009776 ) ) ;
#1488 = VERTEX_POINT ( 'NONE', #48258 ) ;
#1489 = AXIS2_PLACEMENT_3D ( 'NONE', #7046, #21739, #18554 ) ;
#1490 = ORIENTED_EDGE ( 'NONE', *, *, #34399, .T. ) ;
#1491 = CARTESIAN_POINT ( 'NONE',  ( -10.00000000000000000, 0.000000000000000000, 0.000000000000000000 ) ) ;
#1492 = DIRECTION ( 'NONE',  ( -1.000000000000000000, -0.000000000000000000, -0.000000000000000000 ) ) ;
#1493 = VERTEX_POINT ( 'NONE', #267 ) ;
#1495 = EDGE_CURVE ( 'NONE', #34977, #6185, #20515, .T. ) ;
#1494 = AXIS2_PLACEMENT_3D ( 'NONE', #35712, #39142, #34979 ) ;
#1496 = DIRECTION ( 'NONE',  ( -0.7273375899149802093, 0.6862798483830544471, 0.000000000000000000 ) ) ;
#1497 = CARTESIAN_POINT ( 'NONE',  ( 10.00000000000000000, -16.65972982744878195, -80.28980883073774066 ) ) ;
#1498 = CARTESIAN_POINT ( 'NONE',  ( 10.00000000000000000, 0.000000000000000000, 0.000000000000000000 ) ) ;
#1499 = VECTOR ( 'NONE', #43191, 1000.000000000000114 ) ;
#1500 = CYLINDRICAL_SURFACE ( 'NONE', #28134, 16.00000000000000000 ) ;
#1501 = EDGE_CURVE ( 'NONE', #36444, #36385, #34584, .T. ) ;
#1502 = LINE ( 'NONE', #45547, #9467 ) ;
#1503 = FACE_OUTER_BOUND ( 'NONE', #6233, .T. ) ;
#1504 = DIRECTION ( 'NONE',  ( 1.000000000000000000, -0.000000000000000000, 0.000000000000000000 ) ) ;
#1505 = EDGE_CURVE ( 'NONE', #15600, #25099, #3710, .T. ) ;
#1506 = DIRECTION ( 'NONE',  ( -1.000000000000000000, 0.000000000000000000, 0.000000000000000000 ) ) ;
#1507 = LINE ( 'NONE', #16430, #41941 ) ;
#1508 = CARTESIAN_POINT ( 'NONE',  ( 15.00000000000000000, 16.83928648764922542, -16.46020748918050458 ) ) ;
#1509 = CARTESIAN_POINT ( 'NONE',  ( 10.00000000000000000, 0.000000000000000000, 0.000000000000000000 ) ) ;
#1510 = PRESENTATION_STYLE_ASSIGNMENT (( #42637 ) ) ;
#1511 = FACE_OUTER_BOUND ( 'NONE', #21140, .T. ) ;
#1512 = ORIENTED_EDGE ( 'NONE', *, *, #36370, .F. ) ;
#1513 = EDGE_CURVE ( 'NONE', #42302, #20404, #44101, .T. ) ;
#1514 = MECHANICAL_DESIGN_GEOMETRIC_PRESENTATION_REPRESENTATION (  '', ( #11679 ), #32024 ) ;
#1515 = ORIENTED_EDGE ( 'NONE', *, *, #41664, .F. ) ;
#1516 = CARTESIAN_POINT ( 'NONE',  ( -10.00000000000000000, 0.000000000000000000, 0.000000000000000000 ) ) ;
#1517 = ADVANCED_FACE ( 'NONE', ( #32830 ), #36744, .F. ) ;
#1518 = DIRECTION ( 'NONE',  ( 0.000000000000000000, -0.9969173337331287410, 0.07845909572783489605 ) ) ;
#1519 = APPLICATION_PROTOCOL_DEFINITION ( 'draft international standard', 'automotive_design', 1998, #10722 ) ;
#1520 = DIRECTION ( 'NONE',  ( 0.9435911131814398445, -0.3311129884571295534, 0.000000000000000000 ) ) ;
#1521 = VERTEX_POINT ( 'NONE', #10583 ) ;
#1522 = ADVANCED_FACE ( 'NONE', ( #25494 ), #45076, .T. ) ;
#1523 = AXIS2_PLACEMENT_3D ( 'NONE', #5903, #35506, #46780 ) ;
#1524 = CIRCLE ( 'NONE', #7768, 77.49899999999999523 ) ;
#1525 = DIRECTION ( 'NONE',  ( -1.000000000000000000, 0.000000000000000000, 0.000000000000000000 ) ) ;
#1526 = CIRCLE ( 'NONE', #9309, 16.00000000000000000 ) ;
#1527 = ORIENTED_EDGE ( 'NONE', *, *, #6422, .T. ) ;
#1528 = CARTESIAN_POINT ( 'NONE',  ( 5.000000000000000000, -46.11716303203234446, 67.80270845531873647 ) ) ;
#1529 = ORIENTED_EDGE ( 'NONE', *, *, #38033, .F. ) ;
#1530 = EDGE_CURVE ( 'NONE', #31484, #24326, #4202, .T. ) ;
#1531 = CARTESIAN_POINT ( 'NONE',  ( -43.60332556124591719, -117.0000000000000000, -2.500000000000002220 ) ) ;
#1532 = AXIS2_PLACEMENT_3D ( 'NONE', #14785, #17293, #3517 ) ;
#1533 = CARTESIAN_POINT ( 'NONE',  ( 11.99999999999999822, -75.54627589209955829, 17.28742895386058009 ) ) ;
#1534 = VERTEX_POINT ( 'NONE', #45540 ) ;
#1536 = EDGE_LOOP ( 'NONE', ( #37594, #47216, #37658, #17831 ) ) ;
#1535 = CARTESIAN_POINT ( 'NONE',  ( 0.000000000000000000, 0.000000000000000000, 0.000000000000000000 ) ) ;
#1537 = VERTEX_POINT ( 'NONE', #38212 ) ;
#1538 = ORIENTED_EDGE ( 'NONE', *, *, #4386, .F. ) ;
#1539 = CARTESIAN_POINT ( 'NONE',  ( 11.99999999999999822, -68.26794271651239399, -31.47745569255214093 ) ) ;
#1540 = LINE ( 'NONE', #9354, #44111 ) ;
#1541 = FACE_OUTER_BOUND ( 'NONE', #34357, .T. ) ;
#1542 = LINE ( 'NONE', #45859, #18896 ) ;
#1543 = CARTESIAN_POINT ( 'NONE',  ( 11.99999999999999822, -59.03342792756231461, -46.54456581323868392 ) ) ;
#1544 = VERTEX_POINT ( 'NONE', #38711 ) ;
#1545 = CARTESIAN_POINT ( 'NONE',  ( 5.000000000000000000, -56.15606465355001120, 59.75363087400055662 ) ) ;
#1546 = VERTEX_POINT ( 'NONE', #22792 ) ;
#1547 = ORIENTED_EDGE ( 'NONE', *, *, #8949, .T. ) ;
#1548 = EDGE_CURVE ( 'NONE', #1534, #18192, #5173, .T. ) ;
#1549 = DIRECTION ( 'NONE',  ( -1.000000000000000000, 0.000000000000000000, 0.000000000000000000 ) ) ;
#1550 = EDGE_LOOP ( 'NONE', ( #26578, #45657, #31473, #2667 ) ) ;
#1551 = EDGE_CURVE ( 'NONE', #4753, #40406, #3307, .T. ) ;
#1552 = DIRECTION ( 'NONE',  ( -1.000000000000000000, 0.000000000000000000, 0.000000000000000000 ) ) ;
#1553 = CARTESIAN_POINT ( 'NONE',  ( 11.99999999999999822, 0.000000000000000000, 0.000000000000000000 ) ) ;
#1554 = CARTESIAN_POINT ( 'NONE',  ( 0.000000000000000000, -72.35160999960831418, 20.41045688087797672 ) ) ;
#1555 = ORIENTED_EDGE ( 'NONE', *, *, #6304, .T. ) ;
#1556 = DIRECTION ( 'NONE',  ( 0.000000000000000000, 0.000000000000000000, 1.000000000000000000 ) ) ;
#1557 = DIRECTION ( 'NONE',  ( 0.000000000000000000, 0.000000000000000000, 1.000000000000000000 ) ) ;
#1558 = EDGE_CURVE ( 'NONE', #26085, #27526, #13495, .T. ) ;
#1559 = DIRECTION ( 'NONE',  ( 1.000000000000000000, 0.000000000000000000, 0.000000000000000000 ) ) ;
#1560 = FACE_OUTER_BOUND ( 'NONE', #42288, .T. ) ;
#1562 = CIRCLE ( 'NONE', #16394, 31.99999999999999289 ) ;
#1561 = CARTESIAN_POINT ( 'NONE',  ( 11.99999999999999822, 62.50329211542435104, 41.76937507738811917 ) ) ;
#1563 = CIRCLE ( 'NONE', #25780, 82.00000000000000000 ) ;
#1564 = DIRECTION ( 'NONE',  ( -1.000000000000000000, 0.000000000000000000, 0.000000000000000000 ) ) ;
#1566 = ADVANCED_FACE ( 'NONE', ( #42125 ), #20087, .T. ) ;
#1565 = CARTESIAN_POINT ( 'NONE',  ( 11.99999999999999822, 55.16347631943131091, -60.67117009219074930 ) ) ;
#1567 = CARTESIAN_POINT ( 'NONE',  ( 23.49916127795269460, -121.5130826919798039, 5.500000000000000000 ) ) ;
#1568 = CIRCLE ( 'NONE', #21072, 31.99999999999999289 ) ;
#1569 = DIRECTION ( 'NONE',  ( -1.000000000000000000, 0.000000000000000000, -0.000000000000000000 ) ) ;
#1570 = CARTESIAN_POINT ( 'NONE',  ( 10.00000000000000000, 0.000000000000000000, 0.000000000000000000 ) ) ;
#1571 = ORIENTED_EDGE ( 'NONE', *, *, #40112, .F. ) ;
#1572 = ORIENTED_EDGE ( 'NONE', *, *, #1287, .T. ) ;
#1573 = DIRECTION ( 'NONE',  ( 0.000000000000000000, 0.000000000000000000, -1.000000000000000000 ) ) ;
#1574 = AXIS2_PLACEMENT_3D ( 'NONE', #29415, #29645, #40915 ) ;
#1575 = ORIENTED_EDGE ( 'NONE', *, *, #31688, .T. ) ;
#1576 = CARTESIAN_POINT ( 'NONE',  ( 0.000000000000000000, -55.20638768913724448, -51.02545421589383068 ) ) ;
#1577 = DIRECTION ( 'NONE',  ( -1.000000000000000000, -0.000000000000000000, -0.000000000000000000 ) ) ;
#1578 = ORIENTED_EDGE ( 'NONE', *, *, #36315, .T. ) ;
#1579 = ADVANCED_FACE ( 'NONE', ( #12512 ), #750, .T. ) ;
#1580 = CARTESIAN_POINT ( 'NONE',  ( 0.000000000000000000, 0.000000000000000000, 0.000000000000000000 ) ) ;
#1581 = ORIENTED_EDGE ( 'NONE', *, *, #48014, .T. ) ;
#1582 = VERTEX_POINT ( 'NONE', #19115 ) ;
#1583 = EDGE_CURVE ( 'NONE', #43969, #15443, #27442, .T. ) ;
#1584 = ORIENTED_EDGE ( 'NONE', *, *, #39871, .T. ) ;
#1585 = AXIS2_PLACEMENT_3D ( 'NONE', #24108, #20417, #5273 ) ;
#1586 = PLANE ( 'NONE',  #32321 ) ;
#1587 = AXIS2_PLACEMENT_3D ( 'NONE', #8614, #27971, #34553 ) ;
#1588 = CYLINDRICAL_SURFACE ( 'NONE', #18763, 82.00000000000000000 ) ;
#1589 = DIRECTION ( 'NONE',  ( -0.000000000000000000, 0.000000000000000000, -1.000000000000000000 ) ) ;
#1590 = AXIS2_PLACEMENT_3D ( 'NONE', #37542, #8169, #88 ) ;
#1591 = AXIS2_PLACEMENT_3D ( 'NONE', #38926, #967, #19806 ) ;
#1592 = ORIENTED_EDGE ( 'NONE', *, *, #16957, .T. ) ;
#1593 = CARTESIAN_POINT ( 'NONE',  ( 10.00000000000000000, -37.48860685352291711, 0.8828120875899322373 ) ) ;
#1594 = VERTEX_POINT ( 'NONE', #19355 ) ;
#1595 = DIRECTION ( 'NONE',  ( 0.000000000000000000, 0.000000000000000000, 1.000000000000000000 ) ) ;
#1596 = CARTESIAN_POINT ( 'NONE',  ( -1.355716935723729089, -119.3581031311870362, 2.500000000000000000 ) ) ;
#1597 = VECTOR ( 'NONE', #34107, 1000.000000000000114 ) ;
#1598 = CARTESIAN_POINT ( 'NONE',  ( 0.000000000000000000, 67.80270845531887858, 46.11716303203210288 ) ) ;
#1599 = EDGE_LOOP ( 'NONE', ( #11213, #20244, #8248, #7101 ) ) ;
#1600 = ORIENTED_EDGE ( 'NONE', *, *, #21124, .F. ) ;
#1601 = VECTOR ( 'NONE', #12028, 1000.000000000000000 ) ;
#1602 = CARTESIAN_POINT ( 'NONE',  ( -3.000000000000000000, 18.84667830672605859, -18.68964196561243796 ) ) ;
#1603 = ORIENTED_EDGE ( 'NONE', *, *, #35461, .T. ) ;
#1604 = EDGE_CURVE ( 'NONE', #10011, #41264, #23755, .T. ) ;
#1605 = CARTESIAN_POINT ( 'NONE',  ( -18.12185313557660038, -104.9634299478706794, -5.500000000000000000 ) ) ;
#1606 = CARTESIAN_POINT ( 'NONE',  ( 0.000000000000000000, -21.60688246758642705, 79.10210256391358996 ) ) ;
#1607 = DIRECTION ( 'NONE',  ( -1.000000000000000000, 0.000000000000000000, -0.000000000000000000 ) ) ;
#1608 = CARTESIAN_POINT ( 'NONE',  ( 0.000000000000000000, 76.66974797899835892, 11.30684508768368346 ) ) ;
#1609 = DIRECTION ( 'NONE',  ( 0.000000000000000000, 0.000000000000000000, 1.000000000000000000 ) ) ;
#1610 = EDGE_CURVE ( 'NONE', #42762, #16099, #26471, .T. ) ;
#1611 = LINE ( 'NONE', #38095, #1017 ) ;
#1612 = DIRECTION ( 'NONE',  ( -1.000000000000000000, -0.000000000000000000, -0.000000000000000000 ) ) ;
#1613 = VERTEX_POINT ( 'NONE', #12036 ) ;
#1614 = DIRECTION ( 'NONE',  ( -1.000000000000000000, -0.000000000000000000, -0.000000000000000000 ) ) ;
#1615 = LINE ( 'NONE', #40025, #7212 ) ;
#1616 = DIRECTION ( 'NONE',  ( -1.000000000000000000, 0.000000000000000000, -0.000000000000000000 ) ) ;
#1617 = EDGE_LOOP ( 'NONE', ( #30678, #1433, #17533, #44944 ) ) ;
#1618 = VERTEX_POINT ( 'NONE', #30392 ) ;
#1619 = EDGE_CURVE ( 'NONE', #31548, #15804, #18193, .T. ) ;
#1620 = EDGE_CURVE ( 'NONE', #25900, #44934, #41405, .T. ) ;
#1621 = CARTESIAN_POINT ( 'NONE',  ( -18.24502636017239965, -100.7225776329765665, 2.500000000000000000 ) ) ;
#1622 = CARTESIAN_POINT ( 'NONE',  ( 11.99999999999999822, 24.73286445877808148, -73.44644590900034586 ) ) ;
#1623 = DIRECTION ( 'NONE',  ( 0.000000000000000000, 0.9510565162951544194, -0.3090169943749446757 ) ) ;
#1624 = DIRECTION ( 'NONE',  ( 0.000000000000000000, 0.000000000000000000, 1.000000000000000000 ) ) ;
#1625 = CIRCLE ( 'NONE', #10207, 31.99999999999998579 ) ;
#1626 = CARTESIAN_POINT ( 'NONE',  ( 6.377742925735834234, -145.7647898336708181, 5.500000000000000000 ) ) ;
#1627 = DIRECTION ( 'NONE',  ( 0.000000000000000000, 0.000000000000000000, 1.000000000000000000 ) ) ;
#1628 = VECTOR ( 'NONE', #43967, 1000.000000000000000 ) ;
#1629 = ORIENTED_EDGE ( 'NONE', *, *, #48081, .T. ) ;
#1630 = CARTESIAN_POINT ( 'NONE',  ( 10.00000000000000000, 31.52238457039599595, 27.75498641678753842 ) ) ;
#1631 = AXIS2_PLACEMENT_3D ( 'NONE', #31183, #2047, #31675 ) ;
#1632 = VECTOR ( 'NONE', #39657, 1000.000000000000114 ) ;
#1633 = EDGE_LOOP ( 'NONE', ( #23619, #28994, #2601, #45353 ) ) ;
#1634 = CARTESIAN_POINT ( 'NONE',  ( 15.00000000000000000, -26.23277895567245466, 4.042438405570107918 ) ) ;
#1635 = AXIS2_PLACEMENT_3D ( 'NONE', #22052, #14967, #14730 ) ;
#1636 = EDGE_LOOP ( 'NONE', ( #13747, #42938, #25740, #19750 ) ) ;
#1637 = CIRCLE ( 'NONE', #28223, 77.49899999999998101 ) ;
#1638 = ORIENTED_EDGE ( 'NONE', *, *, #26386, .T. ) ;
#1639 = LINE ( 'NONE', #5552, #36656 ) ;
#1640 = ORIENTED_EDGE ( 'NONE', *, *, #44773, .T. ) ;
#1641 = ORIENTED_EDGE ( 'NONE', *, *, #16747, .F. ) ;
#1642 = LINE ( 'NONE', #12423, #39045 ) ;
#1643 = DIRECTION ( 'NONE',  ( -0.8541291221503265474, 0.5200609990133007177, 0.000000000000000000 ) ) ;
#1644 = EDGE_CURVE ( 'NONE', #4498, #6663, #15876, .T. ) ;
#1645 = VERTEX_POINT ( 'NONE', #45806 ) ;
#1646 = ORIENTED_EDGE ( 'NONE', *, *, #2526, .T. ) ;
#1647 = ORIENTED_EDGE ( 'NONE', *, *, #19926, .F. ) ;
#1648 = CARTESIAN_POINT ( 'NONE',  ( 1.384174031800307736, -119.4220188154534981, 2.500000000000000000 ) ) ;
#1650 = ORIENTED_EDGE ( 'NONE', *, *, #46870, .F. ) ;
#1649 = CARTESIAN_POINT ( 'NONE',  ( 0.000000000000000000, -62.50884508063453637, 41.76106447765467777 ) ) ;
#1651 = VECTOR ( 'NONE', #29901, 1000.000000000000000 ) ;
#1652 = FACE_OUTER_BOUND ( 'NONE', #20298, .T. ) ;
#1654 = ORIENTED_EDGE ( 'NONE', *, *, #12136, .T. ) ;
#1653 = AXIS2_PLACEMENT_3D ( 'NONE', #47358, #43911, #29225 ) ;
#1655 = CARTESIAN_POINT ( 'NONE',  ( 0.000000000000000000, -21.53537804866058991, -30.80686688397033635 ) ) ;
#1656 = ORIENTED_EDGE ( 'NONE', *, *, #27421, .F. ) ;
#1657 = ORIENTED_EDGE ( 'NONE', *, *, #34367, .T. ) ;
#1658 = CARTESIAN_POINT ( 'NONE',  ( 10.00000000000000000, 17.28742895386084655, 75.54627589209950145 ) ) ;
#1659 = AXIS2_PLACEMENT_3D ( 'NONE', #42605, #5164, #30612 ) ;
#1660 = VECTOR ( 'NONE', #41275, 1000.000000000000000 ) ;
#1661 = DIRECTION ( 'NONE',  ( 0.000000000000000000, 0.9945218953682744001, -0.1045284632676436454 ) ) ;
#1662 = ORIENTED_EDGE ( 'NONE', *, *, #13722, .T. ) ;
#1663 = DIRECTION ( 'NONE',  ( 0.000000000000000000, 0.000000000000000000, 1.000000000000000000 ) ) ;
#1664 = DIRECTION ( 'NONE',  ( -1.000000000000000000, -0.000000000000000000, 0.000000000000000000 ) ) ;
#1665 = EDGE_CURVE ( 'NONE', #24652, #39658, #43998, .T. ) ;
#1666 = DIRECTION ( 'NONE',  ( -1.000000000000000000, 0.000000000000000000, 0.000000000000000000 ) ) ;
#1667 = ORIENTED_EDGE ( 'NONE', *, *, #7528, .F. ) ;
#1668 = AXIS2_PLACEMENT_3D ( 'NONE', #30817, #1188, #34704 ) ;
#1669 = EDGE_CURVE ( 'NONE', #17158, #45189, #41661, .T. ) ;
#1670 = EDGE_CURVE ( 'NONE', #20033, #47513, #16189, .T. ) ;
#1671 = ORIENTED_EDGE ( 'NONE', *, *, #29612, .F. ) ;
#1672 = CIRCLE ( 'NONE', #25867, 82.00000000000000000 ) ;
#1673 = DIRECTION ( 'NONE',  ( 0.3853207896976523772, -0.9227826878668550226, 0.000000000000000000 ) ) ;
#1674 = DIRECTION ( 'NONE',  ( -1.000000000000000000, 0.000000000000000000, 0.000000000000000000 ) ) ;
#1675 = ORIENTED_EDGE ( 'NONE', *, *, #13205, .T. ) ;
#1676 = AXIS2_PLACEMENT_3D ( 'NONE', #45673, #4560, #7516 ) ;
#1678 = EDGE_CURVE ( 'NONE', #33852, #20108, #3351, .T. ) ;
#1677 = CARTESIAN_POINT ( 'NONE',  ( 0.000000000000000000, 39.78640506895604290, 66.50666863322015843 ) ) ;
#1679 = ORIENTED_EDGE ( 'NONE', *, *, #45056, .T. ) ;
#1680 = DIRECTION ( 'NONE',  ( -1.000000000000000000, 0.000000000000000000, 0.000000000000000000 ) ) ;
#1681 = DIRECTION ( 'NONE',  ( -0.6516173805718079581, 0.7585478161175704948, 0.000000000000000000 ) ) ;
#1682 = CARTESIAN_POINT ( 'NONE',  ( -3.000000000000000000, 14.60985201121729737, -18.46759930825687945 ) ) ;
#1683 = ADVANCED_FACE ( 'NONE', ( #6128 ), #28642, .F. ) ;
#1684 = VERTEX_POINT ( 'NONE', #2434 ) ;
#1685 = CARTESIAN_POINT ( 'NONE',  ( -10.90473778262209414, 0.000000000000000000, -13.71319123046128752 ) ) ;
#1686 = CARTESIAN_POINT ( 'NONE',  ( 10.00000000000000000, -72.35160999960801576, -20.41045688087902121 ) ) ;
#1687 = DIRECTION ( 'NONE',  ( 0.000000000000000000, 0.000000000000000000, 1.000000000000000000 ) ) ;
#1688 = CIRCLE ( 'NONE', #18076, 31.99999999999998934 ) ;
#1689 = CARTESIAN_POINT ( 'NONE',  ( 5.000000000000002665, -76.69515212745996280, -29.01471420065644580 ) ) ;
#1690 = FACE_OUTER_BOUND ( 'NONE', #21535, .T. ) ;
#1691 = CARTESIAN_POINT ( 'NONE',  ( 10.00000000000000000, 31.47745569255237896, -68.26794271651228030 ) ) ;
#1692 = VERTEX_POINT ( 'NONE', #46999 ) ;
#1693 = LINE ( 'NONE', #24202, #22926 ) ;
#1694 = FILL_AREA_STYLE_COLOUR ( '', #30434 ) ;
#1695 = ORIENTED_EDGE ( 'NONE', *, *, #7105, .F. ) ;
#1696 = VECTOR ( 'NONE', #7755, 1000.000000000000000 ) ;
#1697 = AXIS2_PLACEMENT_3D ( 'NONE', #19227, #34623, #41753 ) ;
#1698 = AXIS2_PLACEMENT_3D ( 'NONE', #26577, #30262, #37106 ) ;
#1699 = FACE_OUTER_BOUND ( 'NONE', #14844, .T. ) ;
#1700 = CARTESIAN_POINT ( 'NONE',  ( 10.00000000000000000, -75.54627589209955829, 17.28742895386058009 ) ) ;
#1701 = ORIENTED_EDGE ( 'NONE', *, *, #25743, .F. ) ;
#1702 = AXIS2_PLACEMENT_3D ( 'NONE', #33685, #3339, #4084 ) ;
#1703 = EDGE_CURVE ( 'NONE', #37836, #30905, #10029, .T. ) ;
#1704 = EDGE_CURVE ( 'NONE', #3678, #34848, #8034, .T. ) ;
#1705 = DIRECTION ( 'NONE',  ( 1.000000000000000000, -0.000000000000000000, -0.000000000000000000 ) ) ;
#1706 = VERTEX_POINT ( 'NONE', #20558 ) ;
#1707 = VECTOR ( 'NONE', #12986, 1000.000000000000000 ) ;
#1708 = EDGE_CURVE ( 'NONE', #41727, #22790, #24953, .T. ) ;
#1709 = ORIENTED_EDGE ( 'NONE', *, *, #13515, .T. ) ;
#1710 = ORIENTED_EDGE ( 'NONE', *, *, #26861, .T. ) ;
#1711 = VERTEX_POINT ( 'NONE', #6368 ) ;
#1712 = ADVANCED_FACE ( 'NONE', ( #9790 ), #1731, .T. ) ;
#1713 = DIRECTION ( 'NONE',  ( 1.000000000000000000, 0.000000000000000000, 0.000000000000000000 ) ) ;
#1714 = ORIENTED_EDGE ( 'NONE', *, *, #46087, .F. ) ;
#1715 = CARTESIAN_POINT ( 'NONE',  ( -3.000000000000000000, -4.261787119645322974, 26.19803753235774835 ) ) ;
#1716 = ORIENTED_EDGE ( 'NONE', *, *, #22153, .T. ) ;
#1717 = FACE_OUTER_BOUND ( 'NONE', #44692, .T. ) ;
#1718 = DIRECTION ( 'NONE',  ( -1.000000000000000000, 0.000000000000000000, -0.000000000000000000 ) ) ;
#1719 = PLANE ( 'NONE',  #41597 ) ;
#1720 = ORIENTED_EDGE ( 'NONE', *, *, #16957, .F. ) ;
#1721 = EDGE_CURVE ( 'NONE', #18546, #11579, #43233, .T. ) ;
#1722 = CYLINDRICAL_SURFACE ( 'NONE', #21208, 16.00000000000000000 ) ;
#1723 = EDGE_CURVE ( 'NONE', #2146, #23354, #22117, .T. ) ;
#1724 = ORIENTED_EDGE ( 'NONE', *, *, #15522, .T. ) ;
#1725 = AXIS2_PLACEMENT_3D ( 'NONE', #28770, #29250, #43217 ) ;
#1726 = DIRECTION ( 'NONE',  ( -1.000000000000000000, 0.000000000000000000, 0.000000000000000000 ) ) ;
#1727 = DIRECTION ( 'NONE',  ( -1.000000000000000000, 0.000000000000000000, 0.000000000000000000 ) ) ;
#1728 = CARTESIAN_POINT ( 'NONE',  ( 10.00000000000000000, 0.000000000000000000, 0.000000000000000000 ) ) ;
#1729 = VERTEX_POINT ( 'NONE', #36213 ) ;
#1730 = ORIENTED_EDGE ( 'NONE', *, *, #27119, .T. ) ;
#1731 = PLANE ( 'NONE',  #26803 ) ;
#1732 = CARTESIAN_POINT ( 'NONE',  ( 11.99999999999999822, -55.38113227695745167, -54.21277698773732823 ) ) ;
#1733 = AXIS2_PLACEMENT_3D ( 'NONE', #14357, #44219, #25602 ) ;
#1734 = FACE_OUTER_BOUND ( 'NONE', #37102, .T. ) ;
#1735 = CARTESIAN_POINT ( 'NONE',  ( 10.00000000000000000, 75.54627589209943039, 17.28742895386112721 ) ) ;
#1736 = LINE ( 'NONE', #16663, #47197 ) ;
#1737 = CARTESIAN_POINT ( 'NONE',  ( 11.99999999999999822, 0.000000000000000000, 0.000000000000000000 ) ) ;
#1738 = VECTOR ( 'NONE', #7203, 1000.000000000000227 ) ;
#1739 = DIRECTION ( 'NONE',  ( 0.000000000000000000, -6.938893903907228378E-15, 1.000000000000000000 ) ) ;
#1740 = EDGE_CURVE ( 'NONE', #17387, #44456, #31511, .T. ) ;
#1741 = DIRECTION ( 'NONE',  ( 1.000000000000000000, 0.000000000000000000, 0.000000000000000000 ) ) ;
#1742 = VERTEX_POINT ( 'NONE', #16657 ) ;
#1743 = CYLINDRICAL_SURFACE ( 'NONE', #46601, 42.00000000000000000 ) ;
#1744 = CYLINDRICAL_SURFACE ( 'NONE', #9183, 16.00000000000000000 ) ;
#1745 = DIRECTION ( 'NONE',  ( 0.000000000000000000, -0.8910065241883626808, -0.4539904997395568520 ) ) ;
#1746 = VECTOR ( 'NONE', #40375, 1000.000000000000000 ) ;
#1747 = EDGE_LOOP ( 'NONE', ( #24600, #3735, #14159, #36604 ) ) ;
#1748 = CYLINDRICAL_SURFACE ( 'NONE', #28369, 16.00000000000000000 ) ;
#1749 = DIRECTION ( 'NONE',  ( 0.000000000000000000, -0.4539904997395350916, -0.8910065241883738940 ) ) ;
#1750 = CARTESIAN_POINT ( 'NONE',  ( 11.99999999999999822, -76.66974797899844418, 11.30684508768314522 ) ) ;
#1751 = VERTEX_POINT ( 'NONE', #31607 ) ;
#1752 = ORIENTED_EDGE ( 'NONE', *, *, #5598, .F. ) ;
#1753 = CARTESIAN_POINT ( 'NONE',  ( 2.117611129180199558, -93.54218975225703048, 5.500000000000000000 ) ) ;
#1754 = DIRECTION ( 'NONE',  ( 0.000000000000000000, 0.000000000000000000, 1.000000000000000000 ) ) ;
#1755 = CARTESIAN_POINT ( 'NONE',  ( -20.30386590532152979, -102.9045904027214959, 5.500000000000000000 ) ) ;
#1756 = ORIENTED_EDGE ( 'NONE', *, *, #43410, .T. ) ;
#1757 = VECTOR ( 'NONE', #32623, 1000.000000000000000 ) ;
#1758 = VECTOR ( 'NONE', #2740, 1000.000000000000000 ) ;
#1759 = EDGE_CURVE ( 'NONE', #4190, #39318, #42854, .T. ) ;
#1760 = CARTESIAN_POINT ( 'NONE',  ( 0.000000000000000000, -40.68715046381937128, 10.41901085202062660 ) ) ;
#1761 = AXIS2_PLACEMENT_3D ( 'NONE', #9295, #16890, #17120 ) ;
#1762 = ORIENTED_EDGE ( 'NONE', *, *, #41288, .F. ) ;
#1763 = PLANE ( 'NONE',  #44849 ) ;
#1764 = EDGE_CURVE ( 'NONE', #6185, #36907, #24011, .T. ) ;
#1765 = ORIENTED_EDGE ( 'NONE', *, *, #45721, .F. ) ;
#1766 = DIRECTION ( 'NONE',  ( 0.000000000000000000, 0.000000000000000000, 1.000000000000000000 ) ) ;
#1767 = EDGE_CURVE ( 'NONE', #29872, #44170, #46774, .T. ) ;
#1768 = VECTOR ( 'NONE', #29838, 1000.000000000000000 ) ;
#1769 = DIRECTION ( 'NONE',  ( -1.000000000000000000, -0.000000000000000000, -0.000000000000000000 ) ) ;
#1770 = LINE ( 'NONE', #12079, #42258 ) ;
#1771 = ORIENTED_EDGE ( 'NONE', *, *, #7716, .T. ) ;
#1772 = DIRECTION ( 'NONE',  ( -1.000000000000000000, 0.000000000000000000, -0.000000000000000000 ) ) ;
#1773 = VECTOR ( 'NONE', #23912, 1000.000000000000000 ) ;
#1774 = ORIENTED_EDGE ( 'NONE', *, *, #47202, .F. ) ;
#1775 = DIRECTION ( 'NONE',  ( 0.000000000000000000, 0.000000000000000000, -1.000000000000000000 ) ) ;
#1776 = EDGE_CURVE ( 'NONE', #34549, #42227, #192, .T. ) ;
#1777 = CARTESIAN_POINT ( 'NONE',  ( 0.000000000000000000, -65.59268652807237743, 36.72794159290217664 ) ) ;
#1778 = PLANE ( 'NONE',  #23131 ) ;
#1779 = EDGE_CURVE ( 'NONE', #22321, #38425, #24729, .T. ) ;
#1780 = DIRECTION ( 'NONE',  ( -1.000000000000000000, -0.000000000000000000, 0.000000000000000000 ) ) ;
#1781 = DIRECTION ( 'NONE',  ( -1.000000000000000000, -0.000000000000000000, -0.000000000000000000 ) ) ;
#1782 = ORIENTED_EDGE ( 'NONE', *, *, #1344, .T. ) ;
#1783 = CARTESIAN_POINT ( 'NONE',  ( 10.00000000000000000, 0.000000000000000000, 0.000000000000000000 ) ) ;
#1784 = VERTEX_POINT ( 'NONE', #39674 ) ;
#1785 = ORIENTED_EDGE ( 'NONE', *, *, #39352, .F. ) ;
#1786 = EDGE_CURVE ( 'NONE', #32422, #1423, #2532, .T. ) ;
#1787 = CARTESIAN_POINT ( 'NONE',  ( 0.000000000000000000, 80.28980883073781172, -16.65972982744850128 ) ) ;
#1788 = AXIS2_PLACEMENT_3D ( 'NONE', #48428, #29831, #36457 ) ;
#1789 = CARTESIAN_POINT ( 'NONE',  ( 11.99999999999999822, 74.65374052328660071, -8.840884882374309583 ) ) ;
#1790 = CARTESIAN_POINT ( 'NONE',  ( 0.000000000000000000, 70.52718814184260054, 26.02418014898334420 ) ) ;
#1791 = CARTESIAN_POINT ( 'NONE',  ( 0.000000000000000000, 4.992566952385522505, -37.16516213103271582 ) ) ;
#1792 = VERTEX_POINT ( 'NONE', #13714 ) ;
#1793 = CARTESIAN_POINT ( 'NONE',  ( 5.000000000000000000, 50.23322058963442061, -64.81221759200289512 ) ) ;
#1794 = CIRCLE ( 'NONE', #27579, 31.99999999999999289 ) ;
#1795 = CARTESIAN_POINT ( 'NONE',  ( -3.000000000000000000, 16.83928648764923253, 16.46020748918050458 ) ) ;
#1796 = LINE ( 'NONE', #4740, #39146 ) ;
#1797 = VECTOR ( 'NONE', #7586, 1000.000000000000000 ) ;
#1798 = DIRECTION ( 'NONE',  ( 0.000000000000000000, 0.000000000000000000, -1.000000000000000000 ) ) ;
#1799 = EDGE_CURVE ( 'NONE', #45678, #897, #16417, .T. ) ;
#1800 = CARTESIAN_POINT ( 'NONE',  ( 0.000000000000000000, 30.41916302227216562, -71.27951684757994144 ) ) ;
#1801 = VECTOR ( 'NONE', #34768, 1000.000000000000114 ) ;
#1802 = DIRECTION ( 'NONE',  ( 0.000000000000000000, 0.000000000000000000, 1.000000000000000000 ) ) ;
#1803 = DIRECTION ( 'NONE',  ( -1.000000000000000000, 0.000000000000000000, 0.000000000000000000 ) ) ;
#1804 = CARTESIAN_POINT ( 'NONE',  ( 0.000000000000000000, 23.50000000000000000, 1.499999999999997780 ) ) ;
#1805 = AXIS2_PLACEMENT_3D ( 'NONE', #22965, #30552, #11713 ) ;
#1806 = VECTOR ( 'NONE', #9245, 1000.000000000000000 ) ;
#1807 = DIRECTION ( 'NONE',  ( 0.000000000000000000, 0.000000000000000000, 1.000000000000000000 ) ) ;
#1808 = CARTESIAN_POINT ( 'NONE',  ( 0.000000000000000000, 0.000000000000000000, 0.000000000000000000 ) ) ;
#1809 = AXIS2_PLACEMENT_3D ( 'NONE', #37378, #7267, #415 ) ;
#1810 = ORIENTED_EDGE ( 'NONE', *, *, #23986, .F. ) ;
#1811 = ORIENTED_EDGE ( 'NONE', *, *, #489, .T. ) ;
#1812 = CARTESIAN_POINT ( 'NONE',  ( -9.332068499558253905, 6.890028847512361665, -54.99999999999998579 ) ) ;
#1813 = AXIS2_PLACEMENT_3D ( 'NONE', #37062, #30219, #37788 ) ;
#1814 = ORIENTED_EDGE ( 'NONE', *, *, #30206, .T. ) ;
#1815 = CARTESIAN_POINT ( 'NONE',  ( 10.00000000000000000, -35.95386929396248377, -10.96151621346525751 ) ) ;
#1816 = CARTESIAN_POINT ( 'NONE',  ( 6.000000000000000000, -81.34940948281328588, -10.30890764327469000 ) ) ;
#1817 = VERTEX_POINT ( 'NONE', #9078 ) ;
#1818 = DIRECTION ( 'NONE',  ( 0.9918136447140101231, -0.1276937514489694114, 0.000000000000000000 ) ) ;
#1819 = EDGE_CURVE ( 'NONE', #30895, #38290, #37737, .T. ) ;
#1821 = EDGE_LOOP ( 'NONE', ( #25451, #11030, #4966, #38289 ) ) ;
#1820 = ADVANCED_BREP_SHAPE_REPRESENTATION ( '', ( #35626, #11636 ), #3848 ) ;
#1822 = ORIENTED_EDGE ( 'NONE', *, *, #3672, .T. ) ;
#1823 = ADVANCED_FACE ( 'NONE', ( #24238 ), #47696, .F. ) ;
#1824 = ORIENTED_EDGE ( 'NONE', *, *, #18288, .F. ) ;
#1825 = EDGE_CURVE ( 'NONE', #1345, #9341, #2672, .T. ) ;
#1826 = CIRCLE ( 'NONE', #29174, 21.00000000000000000 ) ;
#1827 = EDGE_CURVE ( 'NONE', #41993, #44214, #21996, .T. ) ;
#1828 = LINE ( 'NONE', #2299, #19025 ) ;
#1829 = EDGE_CURVE ( 'NONE', #15099, #17725, #35389, .T. ) ;
#1830 = EDGE_CURVE ( 'NONE', #25492, #2837, #21300, .T. ) ;
#1831 = LINE ( 'NONE', #35347, #4699 ) ;
#1832 = CIRCLE ( 'NONE', #47928, 16.00000000000000000 ) ;
#1833 = VECTOR ( 'NONE', #41395, 1000.000000000000000 ) ;
#1834 = FACE_OUTER_BOUND ( 'NONE', #20477, .T. ) ;
#1835 = ORIENTED_EDGE ( 'NONE', *, *, #33379, .F. ) ;
#1836 = DIRECTION ( 'NONE',  ( 0.000000000000000000, 0.8660254037844432595, 0.4999999999999919509 ) ) ;
#1837 = ORIENTED_EDGE ( 'NONE', *, *, #62, .T. ) ;
#1838 = AXIS2_PLACEMENT_3D ( 'NONE', #30287, #25863, #18035 ) ;
#1839 = VERTEX_POINT ( 'NONE', #13944 ) ;
#1840 = CARTESIAN_POINT ( 'NONE',  ( 15.00000000000000000, -19.89357724624986545, 12.59942793731086219 ) ) ;
#1841 = DIRECTION ( 'NONE',  ( -1.000000000000000000, 0.000000000000000000, 0.000000000000000000 ) ) ;
#1842 = DIRECTION ( 'NONE',  ( 0.000000000000000000, -0.8090169943749403458, -0.5877852522924830181 ) ) ;
#1843 = EDGE_LOOP ( 'NONE', ( #25317, #43109, #16471, #20186 ) ) ;
#1844 = VECTOR ( 'NONE', #3542, 1000.000000000000000 ) ;
#1845 = ORIENTED_EDGE ( 'NONE', *, *, #9064, .F. ) ;
#1846 = VERTEX_POINT ( 'NONE', #47474 ) ;
#1847 = DIRECTION ( 'NONE',  ( 0.000000000000000000, -0.5877852522924802425, 0.8090169943749422332 ) ) ;
#1848 = EDGE_LOOP ( 'NONE', ( #21536, #11227, #33537, #5622, #47988 ) ) ;
#1849 = ADVANCED_FACE ( 'NONE', ( #10516 ), #28864, .T. ) ;
#1850 = AXIS2_PLACEMENT_3D ( 'NONE', #5902, #43341, #47005 ) ;
#1851 = DIRECTION ( 'NONE',  ( 0.000000000000000000, 0.000000000000000000, 1.000000000000000000 ) ) ;
#1852 = VECTOR ( 'NONE', #4476, 1000.000000000000000 ) ;
#1853 = LINE ( 'NONE', #35851, #18307 ) ;
#1854 = DIRECTION ( 'NONE',  ( 0.000000000000000000, 0.000000000000000000, 1.000000000000000000 ) ) ;
#1855 = DIRECTION ( 'NONE',  ( -1.000000000000000000, -0.000000000000000000, 0.000000000000000000 ) ) ;
#1856 = CARTESIAN_POINT ( 'NONE',  ( 11.99999999999999822, -21.60688246758531150, -79.10210256391390260 ) ) ;
#1857 = DIRECTION ( 'NONE',  ( -1.000000000000000000, -0.000000000000000000, 0.000000000000000000 ) ) ;
#1858 = LINE ( 'NONE', #35625, #14279 ) ;
#1859 = EDGE_LOOP ( 'NONE', ( #45005, #46756, #29798, #31221 ) ) ;
#1860 = CARTESIAN_POINT ( 'NONE',  ( -42.50000000000000000, 0.000000000000000000, 0.000000000000000000 ) ) ;
#1861 = CARTESIAN_POINT ( 'NONE',  ( 8.700667342345820288, -98.11853780484867116, -5.500000000000000000 ) ) ;
#1862 = CARTESIAN_POINT ( 'NONE',  ( 11.99999999999999822, 21.60688246758586573, 79.10210256391376049 ) ) ;
#1863 = EDGE_CURVE ( 'NONE', #14446, #12027, #33270, .T. ) ;
#1864 = CARTESIAN_POINT ( 'NONE',  ( 10.00000000000000000, 75.16055320797030959, 18.89407956138283851 ) ) ;
#1865 = ORIENTED_EDGE ( 'NONE', *, *, #2991, .F. ) ;
#1866 = EDGE_LOOP ( 'NONE', ( #30052, #32484, #35977, #12365 ) ) ;
#1867 = DIRECTION ( 'NONE',  ( -1.000000000000000000, 0.000000000000000000, 0.000000000000000000 ) ) ;
#1868 = FACE_OUTER_BOUND ( 'NONE', #28081, .T. ) ;
#1869 = CARTESIAN_POINT ( 'NONE',  ( 11.99999999999999822, 8.840884882376133902, -74.65374052328640175 ) ) ;
#1870 = CARTESIAN_POINT ( 'NONE',  ( -0.2999999999999964362, 1.567547902908612184E-15, 12.80000000000000071 ) ) ;
#1872 = VECTOR ( 'NONE', #43652, 1000.000000000000000 ) ;
#1871 = CARTESIAN_POINT ( 'NONE',  ( 10.00000000000000000, -26.02418014898260878, -70.52718814184285634 ) ) ;
#1873 = EDGE_CURVE ( 'NONE', #20499, #29866, #31502, .T. ) ;
#1874 = VERTEX_POINT ( 'NONE', #10997 ) ;
#1875 = CARTESIAN_POINT ( 'NONE',  ( 0.000000000000000000, 2.956366410620650420, 75.11725578898469280 ) ) ;
#1876 = DIRECTION ( 'NONE',  ( -1.000000000000000000, -0.000000000000000000, -0.000000000000000000 ) ) ;
#1877 = ORIENTED_EDGE ( 'NONE', *, *, #40436, .T. ) ;
#1878 = CIRCLE ( 'NONE', #33094, 15.99999999999999822 ) ;
#1880 = AXIS2_PLACEMENT_3D ( 'NONE', #27810, #9662, #31479 ) ;
#1879 = DIRECTION ( 'NONE',  ( 0.000000000000000000, -0.1045284632676578285, 0.9945218953682729568 ) ) ;
#1881 = VECTOR ( 'NONE', #24375, 1000.000000000000227 ) ;
#1882 = ORIENTED_EDGE ( 'NONE', *, *, #31239, .T. ) ;
#1883 = PRODUCT ( 'CIRCLIP DIN 471 - 25 \X2\00d7\X0\ 1.2_GB_CONNECTING_PIECE_RING_RRA 25', 'CIRCLIP DIN 471 - 25 \X2\00d7\X0\ 1.2_GB_CONNECTING_PIECE_RING_RRA 25', '', ( #9214 ) ) ;
#1884 = LINE ( 'NONE', #40044, #20526 ) ;
#1885 = ORIENTED_EDGE ( 'NONE', *, *, #34338, .T. ) ;
#1886 = ORIENTED_EDGE ( 'NONE', *, *, #24377, .F. ) ;
#1887 = ADVANCED_FACE ( 'NONE', ( #10760 ), #40854, .T. ) ;
#1888 = VECTOR ( 'NONE', #1643, 1000.000000000000227 ) ;
#1889 = CIRCLE ( 'NONE', #13614, 21.00000000000000000 ) ;
#1890 = VECTOR ( 'NONE', #41590, 1000.000000000000000 ) ;
#1891 = ADVANCED_FACE ( 'NONE', ( #7074 ), #33502, .T. ) ;
#1892 = ORIENTED_EDGE ( 'NONE', *, *, #43418, .T. ) ;
#1893 = AXIS2_PLACEMENT_3D ( 'NONE', #47498, #23248, #38180 ) ;
#1894 = VECTOR ( 'NONE', #10151, 1000.000000000000000 ) ;
#1895 = CARTESIAN_POINT ( 'NONE',  ( 0.000000000000000000, -34.94270380257585629, -74.18225833017926618 ) ) ;
#1896 = ADVANCED_FACE ( 'NONE', ( #40607 ), #3651, .T. ) ;
#1897 = EDGE_LOOP ( 'NONE', ( #30604, #10445, #36560, #36897 ) ) ;
#1898 = AXIS2_PLACEMENT_3D ( 'NONE', #39465, #19867, #39214 ) ;
#1899 = ADVANCED_FACE ( 'NONE', ( #44762 ), #41113, .T. ) ;
#1900 = EDGE_CURVE ( 'NONE', #39824, #2611, #6462, .T. ) ;
#1901 = DIRECTION ( 'NONE',  ( -1.000000000000000000, 0.000000000000000000, -0.000000000000000000 ) ) ;
#1902 = DIRECTION ( 'NONE',  ( -1.000000000000000000, -0.000000000000000000, -0.000000000000000000 ) ) ;
#1903 = ORIENTED_EDGE ( 'NONE', *, *, #27770, .T. ) ;
#1904 = VERTEX_POINT ( 'NONE', #32771 ) ;
#1905 = DIRECTION ( 'NONE',  ( -1.000000000000000000, 0.000000000000000000, -0.000000000000000000 ) ) ;
#1907 = ORIENTED_EDGE ( 'NONE', *, *, #20842, .F. ) ;
#1906 = CARTESIAN_POINT ( 'NONE',  ( 0.000000000000000000, -50.95692526931372157, 58.39081064771733054 ) ) ;
#1909 = DIRECTION ( 'NONE',  ( -1.000000000000000000, 0.000000000000000000, -0.000000000000000000 ) ) ;
#1908 = CIRCLE ( 'NONE', #26143, 16.00000000000000000 ) ;
#1910 = VERTEX_POINT ( 'NONE', #29103 ) ;
#1911 = ORIENTED_EDGE ( 'NONE', *, *, #13116, .F. ) ;
#1912 = CARTESIAN_POINT ( 'NONE',  ( 0.000000000000000000, 23.59884966291521380, 12.14883922797262805 ) ) ;
#1913 = ORIENTED_EDGE ( 'NONE', *, *, #40170, .T. ) ;
#1914 = VERTEX_POINT ( 'NONE', #44043 ) ;
#1915 = CARTESIAN_POINT ( 'NONE',  ( 10.00000000000000000, -51.02545421589363883, 55.20638768913742922 ) ) ;
#1916 = AXIS2_PLACEMENT_3D ( 'NONE', #11727, #30565, #26658 ) ;
#1917 = DIRECTION ( 'NONE',  ( -1.000000000000000000, 0.000000000000000000, 0.000000000000000000 ) ) ;
#1918 = CARTESIAN_POINT ( 'NONE',  ( 10.00000000000000000, -73.72996012237429397, -14.67089635893794508 ) ) ;
#1919 = CARTESIAN_POINT ( 'NONE',  ( 10.00000000000000000, -21.40280677340398441, 36.13751322684410638 ) ) ;
#1920 = VECTOR ( 'NONE', #32364, 1000.000000000000114 ) ;
#1921 = CARTESIAN_POINT ( 'NONE',  ( 0.000000000000000000, -60.67117009219175827, 55.16347631943019536 ) ) ;
#1922 = EDGE_LOOP ( 'NONE', ( #3443, #46352, #1671, #43044 ) ) ;
#1923 = ORIENTED_EDGE ( 'NONE', *, *, #37157, .T. ) ;
#1924 = CARTESIAN_POINT ( 'NONE',  ( 5.999999999999999112, -74.74816331893404708, -33.71516098798818462 ) ) ;
#1925 = LINE ( 'NONE', #47175, #20453 ) ;
#1926 = AXIS2_PLACEMENT_3D ( 'NONE', #26451, #44800, #31277 ) ;
#1927 = CIRCLE ( 'NONE', #8159, 42.00000000000000000 ) ;
#1928 = EDGE_LOOP ( 'NONE', ( #23263, #17480, #3567, #17108 ) ) ;
#1929 = VECTOR ( 'NONE', #19712, 1000.000000000000000 ) ;
#1930 = FACE_OUTER_BOUND ( 'NONE', #36547, .T. ) ;
#1931 = ORIENTED_EDGE ( 'NONE', *, *, #7229, .F. ) ;
#1932 = AXIS2_PLACEMENT_3D ( 'NONE', #20050, #1218, #9275 ) ;
#1933 = DIRECTION ( 'NONE',  ( 0.000000000000000000, 0.5877852522924684742, 0.8090169943749506709 ) ) ;
#1934 = DIRECTION ( 'NONE',  ( -1.000000000000000000, -0.000000000000000000, 0.000000000000000000 ) ) ;
#1935 = CARTESIAN_POINT ( 'NONE',  ( 0.000000000000000000, -120.0000000000000000, 2.500000000000000000 ) ) ;
#1936 = LINE ( 'NONE', #5848, #22129 ) ;
#1937 = CIRCLE ( 'NONE', #17524, 31.99999999999998579 ) ;
#1938 = CARTESIAN_POINT ( 'NONE',  ( 0.000000000000000000, -38.55633173626998911, -16.65560815589452304 ) ) ;
#1939 = EDGE_LOOP ( 'NONE', ( #28039, #5808, #34501, #32987 ) ) ;
#1940 = LINE ( 'NONE', #46483, #2114 ) ;
#1941 = CARTESIAN_POINT ( 'NONE',  ( -0.2999999999999964362, 0.000000000000000000, 0.000000000000000000 ) ) ;
#1942 = DIRECTION ( 'NONE',  ( -1.000000000000000000, -0.000000000000000000, 0.000000000000000000 ) ) ;
#1943 = ORIENTED_EDGE ( 'NONE', *, *, #20789, .F. ) ;
#1944 = CARTESIAN_POINT ( 'NONE',  ( 15.00000000000000000, 20.85821328998741109, -10.92862929874522671 ) ) ;
#1945 =( NAMED_UNIT ( * ) SI_UNIT ( $, .STERADIAN. ) SOLID_ANGLE_UNIT ( ) );
#1946 = ORIENTED_EDGE ( 'NONE', *, *, #26607, .T. ) ;
#1947 = EDGE_LOOP ( 'NONE', ( #17212, #46442, #44132, #37392 ) ) ;
#1948 = VECTOR ( 'NONE', #470, 1000.000000000000000 ) ;
#1949 = ADVANCED_FACE ( 'NONE', ( #25429 ), #21761, .F. ) ;
#1950 = AXIS2_PLACEMENT_3D ( 'NONE', #23134, #30982, #41990 ) ;
#1951 = AXIS2_PLACEMENT_3D ( 'NONE', #27045, #8427, #23352 ) ;
#1952 = ORIENTED_EDGE ( 'NONE', *, *, #6865, .F. ) ;
#1953 = DIRECTION ( 'NONE',  ( -1.000000000000000000, 0.000000000000000000, 0.000000000000000000 ) ) ;
#1954 = ADVANCED_FACE ( 'NONE', ( #47944 ), #33013, .T. ) ;
#1955 = DIRECTION ( 'NONE',  ( 0.000000000000000000, 0.000000000000000000, 1.000000000000000000 ) ) ;
#1956 = ORIENTED_EDGE ( 'NONE', *, *, #26185, .F. ) ;
#1957 = EDGE_CURVE ( 'NONE', #13671, #29705, #10340, .T. ) ;
#1958 = CIRCLE ( 'NONE', #9853, 77.49899999999999523 ) ;
#1959 = EDGE_CURVE ( 'NONE', #26190, #34606, #34224, .T. ) ;
#1960 = DIRECTION ( 'NONE',  ( -1.000000000000000000, 0.000000000000000000, 0.000000000000000000 ) ) ;
#1961 = VERTEX_POINT ( 'NONE', #932 ) ;
#1962 = VERTEX_POINT ( 'NONE', #1191 ) ;
#1963 = AXIS2_PLACEMENT_3D ( 'NONE', #22793, #1255, #19356 ) ;
#1964 = ADVANCED_FACE ( 'NONE', ( #4617 ), #8037, .T. ) ;
#1965 = ORIENTED_EDGE ( 'NONE', *, *, #17987, .F. ) ;
#1966 = CIRCLE ( 'NONE', #37133, 31.99999999999999289 ) ;
#1967 = VECTOR ( 'NONE', #41625, 1000.000000000000000 ) ;
#1968 = LINE ( 'NONE', #24219, #46948 ) ;
#1969 = ORIENTED_EDGE ( 'NONE', *, *, #8697, .F. ) ;
#1970 = DIRECTION ( 'NONE',  ( -1.000000000000000000, -0.000000000000000000, -0.000000000000000000 ) ) ;
#1971 = ORIENTED_EDGE ( 'NONE', *, *, #16873, .T. ) ;
#1972 = CYLINDRICAL_SURFACE ( 'NONE', #889, 42.00000000000000000 ) ;
#1973 = EDGE_CURVE ( 'NONE', #39311, #37697, #47850, .T. ) ;
#1974 = CARTESIAN_POINT ( 'NONE',  ( 11.99999999999999822, 0.000000000000000000, 0.000000000000000000 ) ) ;
#1975 = DIRECTION ( 'NONE',  ( -1.000000000000000000, -0.000000000000000000, 0.000000000000000000 ) ) ;
#1976 = ORIENTED_EDGE ( 'NONE', *, *, #17064, .T. ) ;
#1977 = CARTESIAN_POINT ( 'NONE',  ( 11.99999999999999822, 81.50828551894241514, -8.966570791699814080 ) ) ;
#1978 = EDGE_LOOP ( 'NONE', ( #2482, #32004, #25639, #44345 ) ) ;
#1979 = DIRECTION ( 'NONE',  ( -1.000000000000000000, 0.000000000000000000, 0.000000000000000000 ) ) ;
#1980 = VECTOR ( 'NONE', #28472, 1000.000000000000000 ) ;
#1981 = CARTESIAN_POINT ( 'NONE',  ( 0.000000000000000000, 0.000000000000000000, 0.000000000000000000 ) ) ;
#1982 = DIRECTION ( 'NONE',  ( 0.000000000000000000, 0.000000000000000000, 1.000000000000000000 ) ) ;
#1983 = ORIENTED_EDGE ( 'NONE', *, *, #26393, .F. ) ;
#1984 = ORIENTED_EDGE ( 'NONE', *, *, #25087, .T. ) ;
#1985 = CARTESIAN_POINT ( 'NONE',  ( 9.984461079971730157, -95.40710393340120277, 5.500000000000000000 ) ) ;
#1986 = AXIS2_PLACEMENT_3D ( 'NONE', #35367, #35122, #42732 ) ;
#1987 = CARTESIAN_POINT ( 'NONE',  ( 5.999999999999999112, -33.71516098798685590, -74.74816331893465815 ) ) ;
#1988 = EDGE_LOOP ( 'NONE', ( #33319, #21691, #38064, #12586 ) ) ;
#1989 = CARTESIAN_POINT ( 'NONE',  ( 10.00000000000000000, -17.80606268964563554, 33.00180498840040855 ) ) ;
#1990 = DIRECTION ( 'NONE',  ( 0.000000000000000000, 0.000000000000000000, 1.000000000000000000 ) ) ;
#1991 = CARTESIAN_POINT ( 'NONE',  ( 11.99999999999999822, 59.46389618802034960, -49.70050353004825894 ) ) ;
#1992 = PLANE ( 'NONE',  #5433 ) ;
#1993 = DIRECTION ( 'NONE',  ( 0.000000000000000000, 0.8910065241883691201, -0.4539904997395446951 ) ) ;
#1994 = LINE ( 'NONE', #5413, #17703 ) ;
#1995 = ADVANCED_FACE ( 'NONE', ( #12454 ), #16136, .T. ) ;
#1996 = AXIS2_PLACEMENT_3D ( 'NONE', #20917, #27789, #43669 ) ;
#1997 = AXIS2_PLACEMENT_3D ( 'NONE', #26021, #36558, #2785 ) ;
#1998 = DIRECTION ( 'NONE',  ( -0.6516173805718079581, 0.7585478161175704948, 0.000000000000000000 ) ) ;
#1999 = DIRECTION ( 'NONE',  ( -1.000000000000000000, -0.000000000000000000, 0.000000000000000000 ) ) ;
#2000 = ADVANCED_FACE ( 'NONE', ( #34460 ), #34709, .T. ) ;
#2001 = VECTOR ( 'NONE', #38334, 1000.000000000000000 ) ;
#2002 = DIRECTION ( 'NONE',  ( 0.000000000000000000, -0.3090169943749349613, -0.9510565162951576390 ) ) ;
#2003 = CARTESIAN_POINT ( 'NONE',  ( 11.99999999999999822, -65.58780272294048075, -36.73666225445966660 ) ) ;
#2004 = DIRECTION ( 'NONE',  ( -1.000000000000000000, -0.000000000000000000, -0.000000000000000000 ) ) ;
#2005 = EDGE_CURVE ( 'NONE', #9517, #21969, #467, .T. ) ;
#2006 = VECTOR ( 'NONE', #36863, 1000.000000000000114 ) ;
#2007 = DIRECTION ( 'NONE',  ( -1.000000000000000000, 0.000000000000000000, 0.000000000000000000 ) ) ;
#2008 = ORIENTED_EDGE ( 'NONE', *, *, #18559, .F. ) ;
#2009 = ORIENTED_EDGE ( 'NONE', *, *, #27242, .F. ) ;
#2010 = LINE ( 'NONE', #12532, #5745 ) ;
#2011 = DIRECTION ( 'NONE',  ( -1.000000000000000000, 0.000000000000000000, 0.000000000000000000 ) ) ;
#2012 = AXIS2_PLACEMENT_3D ( 'NONE', #16866, #5362, #42317 ) ;
#2013 = EDGE_CURVE ( 'NONE', #44271, #47351, #45253, .T. ) ;
#2014 = DIRECTION ( 'NONE',  ( 0.000000000000000000, 0.000000000000000000, -1.000000000000000000 ) ) ;
#2015 = ORIENTED_EDGE ( 'NONE', *, *, #11271, .F. ) ;
#2016 = EDGE_CURVE ( 'NONE', #4600, #9305, #29864, .T. ) ;
#2017 = ADVANCED_FACE ( 'NONE', ( #22732 ), #27148, .T. ) ;
#2018 = AXIS2_PLACEMENT_3D ( 'NONE', #12822, #43161, #20387 ) ;
#2019 = ORIENTED_EDGE ( 'NONE', *, *, #40436, .F. ) ;
#2020 = DIRECTION ( 'NONE',  ( 1.000000000000000000, 0.000000000000000000, 0.000000000000000000 ) ) ;
#2021 = ORIENTED_EDGE ( 'NONE', *, *, #1620, .F. ) ;
#2022 = DIRECTION ( 'NONE',  ( 0.000000000000000000, 0.8526401643540897357, 0.5224985647159527957 ) ) ;
#2023 = VERTEX_POINT ( 'NONE', #37663 ) ;
#2024 = DIRECTION ( 'NONE',  ( 1.000000000000000000, 0.000000000000000000, 0.000000000000000000 ) ) ;
#2025 = ADVANCED_FACE ( 'NONE', ( #4861 ), #41585, .T. ) ;
#2026 = AXIS2_PLACEMENT_3D ( 'NONE', #35725, #43556, #46755 ) ;
#2027 = CARTESIAN_POINT ( 'NONE',  ( 11.99999999999999822, 0.000000000000000000, 0.000000000000000000 ) ) ;
#2028 = CARTESIAN_POINT ( 'NONE',  ( 4.999999999999999112, -10.41901085202107247, 40.68715046381925049 ) ) ;
#2029 = ORIENTED_EDGE ( 'NONE', *, *, #26470, .T. ) ;
#2031 = VERTEX_POINT ( 'NONE', #30821 ) ;
#2030 = DIRECTION ( 'NONE',  ( 0.000000000000000000, -0.8090169943749508930, 0.5877852522924683631 ) ) ;
#2032 = ORIENTED_EDGE ( 'NONE', *, *, #9725, .T. ) ;
#2033 = AXIS2_PLACEMENT_3D ( 'NONE', #43690, #3045, #14072 ) ;
#2034 = CARTESIAN_POINT ( 'NONE',  ( 3.429551818649054340, -146.3199197248623875, 5.500000000000000000 ) ) ;
#2035 = AXIS2_PLACEMENT_3D ( 'NONE', #17180, #16719, #6424 ) ;
#2036 = CARTESIAN_POINT ( 'NONE',  ( 10.00000000000000000, 33.17418723428333749, -17.67226234102790272 ) ) ;
#2037 = CARTESIAN_POINT ( 'NONE',  ( 9.984461079971730157, -95.40710393340121698, -2.500000000000000000 ) ) ;
#2038 = CARTESIAN_POINT ( 'NONE',  ( 0.000000000000000000, 0.000000000000000000, 0.000000000000000000 ) ) ;
#2039 = ORIENTED_EDGE ( 'NONE', *, *, #21155, .F. ) ;
#2040 = VECTOR ( 'NONE', #22629, 1000.000000000000000 ) ;
#2041 = DIRECTION ( 'NONE',  ( 0.000000000000000000, -0.7431448254773862505, 0.6691306063588671194 ) ) ;
#2042 = ORIENTED_EDGE ( 'NONE', *, *, #31128, .T. ) ;
#2043 = DIRECTION ( 'NONE',  ( 0.000000000000000000, 0.000000000000000000, 1.000000000000000000 ) ) ;
#2044 = CYLINDRICAL_SURFACE ( 'NONE', #15258, 31.99999999999998579 ) ;
#2045 = AXIS2_PLACEMENT_3D ( 'NONE', #19784, #8532, #23462 ) ;
#2046 = FACE_OUTER_BOUND ( 'NONE', #41884, .T. ) ;
#2047 = DIRECTION ( 'NONE',  ( -1.000000000000000000, 0.000000000000000000, 0.000000000000000000 ) ) ;
#2048 = ORIENTED_EDGE ( 'NONE', *, *, #26203, .T. ) ;
#2049 = FACE_OUTER_BOUND ( 'NONE', #13559, .T. ) ;
#2050 = CIRCLE ( 'NONE', #16130, 82.00000000000000000 ) ;
#2051 = CARTESIAN_POINT ( 'NONE',  ( -3.000000000000000000, 18.84667830672579925, 18.68964196561269020 ) ) ;
#2052 = LINE ( 'NONE', #32147, #7095 ) ;
#2053 = DIRECTION ( 'NONE',  ( 0.9038112904824853189, -0.4279312458752977388, 0.000000000000000000 ) ) ;
#2054 = DIRECTION ( 'NONE',  ( -1.000000000000000000, -0.000000000000000000, 0.000000000000000000 ) ) ;
#2055 = EDGE_CURVE ( 'NONE', #15936, #23071, #9562, .T. ) ;
#2056 = CARTESIAN_POINT ( 'NONE',  ( 11.99999999999999822, 77.49459641780886443, 0.8261519478433866359 ) ) ;
#2057 = CARTESIAN_POINT ( 'NONE',  ( 10.00000000000000000, -37.16516213103280108, 4.992566952384862589 ) ) ;
#2058 = DIRECTION ( 'NONE',  ( -0.000000000000000000, -0.000000000000000000, -1.000000000000000000 ) ) ;
#2059 = EDGE_CURVE ( 'NONE', #47361, #20756, #22975, .T. ) ;
#2060 = CARTESIAN_POINT ( 'NONE',  ( 10.00000000000000000, 35.95386929396256903, -10.96151621346501237 ) ) ;
#2061 = CARTESIAN_POINT ( 'NONE',  ( 6.000000000000000000, 44.99326035066052043, 68.55367621811159040 ) ) ;
#2062 = EDGE_CURVE ( 'NONE', #11314, #27936, #42308, .T. ) ;
#2063 = ORIENTED_EDGE ( 'NONE', *, *, #40414, .F. ) ;
#2064 = AXIS2_PLACEMENT_3D ( 'NONE', #38629, #12677, #912 ) ;
#2065 = CARTESIAN_POINT ( 'NONE',  ( 26.09152095774781799, -124.8716048804687375, 5.500000000000000000 ) ) ;
#2066 = ORIENTED_EDGE ( 'NONE', *, *, #3140, .T. ) ;
#2067 = CARTESIAN_POINT ( 'NONE',  ( -0.1219594728601508804, -118.5049662589159567, 2.500000000000000000 ) ) ;
#2068 = AXIS2_PLACEMENT_3D ( 'NONE', #1561, #16489, #31682 ) ;
#2069 = DIRECTION ( 'NONE',  ( 1.000000000000000000, 0.000000000000000000, 0.000000000000000000 ) ) ;
#2070 = ORIENTED_EDGE ( 'NONE', *, *, #39079, .T. ) ;
#2071 = ADVANCED_FACE ( 'NONE', ( #19298 ), #30563, .F. ) ;
#2072 = EDGE_CURVE ( 'NONE', #31321, #23779, #959, .T. ) ;
#2073 = CYLINDRICAL_SURFACE ( 'NONE', #15126, 77.49899999999999523 ) ;
#2074 = CIRCLE ( 'NONE', #28621, 42.00000000000000000 ) ;
#2075 = EDGE_LOOP ( 'NONE', ( #48356, #46035, #47019, #47935 ) ) ;
#2076 = AXIS2_PLACEMENT_3D ( 'NONE', #14, #29642, #36736 ) ;
#2077 = ORIENTED_EDGE ( 'NONE', *, *, #40519, .F. ) ;
#2078 = EDGE_CURVE ( 'NONE', #20399, #7360, #12694, .T. ) ;
#2079 = DIRECTION ( 'NONE',  ( -1.000000000000000000, 0.000000000000000000, 0.000000000000000000 ) ) ;
#2080 = CARTESIAN_POINT ( 'NONE',  ( 15.00000000000000000, -14.54903810567644484, 22.19967320028775504 ) ) ;
#2081 = DIRECTION ( 'NONE',  ( -0.7585478161175706058, -0.6516173805718078471, 0.000000000000000000 ) ) ;
#2082 = VERTEX_POINT ( 'NONE', #28589 ) ;
#2083 = CARTESIAN_POINT ( 'NONE',  ( 0.000000000000000000, 39.78640506895700213, -66.50666863321957578 ) ) ;
#2084 = ORIENTED_EDGE ( 'NONE', *, *, #957, .F. ) ;
#2085 = LINE ( 'NONE', #35354, #31942 ) ;
#2086 = CARTESIAN_POINT ( 'NONE',  ( 2.117611129180199558, -93.54218975225703048, -5.500000000000000000 ) ) ;
#2087 = DIRECTION ( 'NONE',  ( 0.000000000000000000, 0.000000000000000000, 1.000000000000000000 ) ) ;
#2089 = ORIENTED_EDGE ( 'NONE', *, *, #6752, .F. ) ;
#2088 = VECTOR ( 'NONE', #12618, 1000.000000000000000 ) ;
#2090 = ORIENTED_EDGE ( 'NONE', *, *, #4080, .T. ) ;
#2091 = ORIENTED_EDGE ( 'NONE', *, *, #42948, .T. ) ;
#2092 = DIRECTION ( 'NONE',  ( -0.9730327541852497042, 0.2306669878475623159, 0.000000000000000000 ) ) ;
#2093 = VERTEX_POINT ( 'NONE', #13411 ) ;
#2094 = FACE_BOUND ( 'NONE', #47440, .T. ) ;
#2095 = DIRECTION ( 'NONE',  ( -1.000000000000000000, 0.000000000000000000, -0.000000000000000000 ) ) ;
#2096 = CARTESIAN_POINT ( 'NONE',  ( 10.00000000000000000, -30.80686688397025108, 21.53537804866070715 ) ) ;
#2097 = CARTESIAN_POINT ( 'NONE',  ( 15.00000000000000000, -22.32062822937489344, -14.36278369418800160 ) ) ;
#2098 = LINE ( 'NONE', #6019, #1048 ) ;
#2099 = FACE_OUTER_BOUND ( 'NONE', #23007, .T. ) ;
#2100 = CARTESIAN_POINT ( 'NONE',  ( 10.00000000000000000, 0.000000000000000000, 0.000000000000000000 ) ) ;
#2101 = CARTESIAN_POINT ( 'NONE',  ( 10.00000000000000000, -65.64334221924882229, -41.19522573413803457 ) ) ;
#2102 = CARTESIAN_POINT ( 'NONE',  ( -6.112675177960399608, -145.7853679859090903, -2.500000000000000000 ) ) ;
#2103 = DIRECTION ( 'NONE',  ( 0.000000000000000000, 0.000000000000000000, 1.000000000000000000 ) ) ;
#2104 = VERTEX_POINT ( 'NONE', #39619 ) ;
#2105 = VECTOR ( 'NONE', #1681, 1000.000000000000114 ) ;
#2106 = CARTESIAN_POINT ( 'NONE',  ( 0.000000000000000000, 0.000000000000000000, 125.0000000000000000 ) ) ;
#2107 = EDGE_CURVE ( 'NONE', #16993, #41512, #32227, .T. ) ;
#2108 = LINE ( 'NONE', #34649, #27543 ) ;
#2109 = LINE ( 'NONE', #47126, #34666 ) ;
#2110 = AXIS2_PLACEMENT_3D ( 'NONE', #11919, #4574, #19255 ) ;
#2111 = ADVANCED_FACE ( 'NONE', ( #9021 ), #46224, .T. ) ;
#2112 = LINE ( 'NONE', #39305, #31826 ) ;
#2113 = CARTESIAN_POINT ( 'NONE',  ( -4.653126046682595884, -146.1313684676804314, -5.500000000000000000 ) ) ;
#2114 = VECTOR ( 'NONE', #9265, 1000.000000000000000 ) ;
#2115 = CARTESIAN_POINT ( 'NONE',  ( 0.000000000000000000, -46.53671651293907274, -59.03961581697448935 ) ) ;
#2116 = LINE ( 'NONE', #39072, #20623 ) ;
#2118 = EDGE_CURVE ( 'NONE', #25700, #6361, #23957, .T. ) ;
#2117 = ORIENTED_EDGE ( 'NONE', *, *, #18529, .T. ) ;
#2119 = CARTESIAN_POINT ( 'NONE',  ( 12.00000000000000000, -0.9646360437375370855, -23.52805723605590060 ) ) ;
#2120 = VERTEX_POINT ( 'NONE', #35436 ) ;
#2121 = DIRECTION ( 'NONE',  ( 0.000000000000000000, 0.000000000000000000, 1.000000000000000000 ) ) ;
#2122 = ORIENTED_EDGE ( 'NONE', *, *, #13428, .T. ) ;
#2123 = AXIS2_PLACEMENT_3D ( 'NONE', #48325, #30225, #33404 ) ;
#2124 = ORIENTED_EDGE ( 'NONE', *, *, #31457, .T. ) ;
#2125 = EDGE_CURVE ( 'NONE', #5981, #2920, #28332, .T. ) ;
#2126 = CIRCLE ( 'NONE', #38111, 77.49900000000000944 ) ;
#2127 = EDGE_CURVE ( 'NONE', #43486, #44937, #20266, .T. ) ;
#2128 = VERTEX_POINT ( 'NONE', #9255 ) ;
#2129 = CIRCLE ( 'NONE', #38078, 31.99999999999999289 ) ;
#2130 = DIRECTION ( 'NONE',  ( 0.000000000000000000, 0.9135454576426058626, 0.4067366430757889950 ) ) ;
#2131 = ORIENTED_EDGE ( 'NONE', *, *, #23541, .F. ) ;
#2132 = ORIENTED_EDGE ( 'NONE', *, *, #6063, .T. ) ;
#2133 = EDGE_CURVE ( 'NONE', #2398, #10384, #20991, .T. ) ;
#2134 = AXIS2_PLACEMENT_3D ( 'NONE', #6917, #39980, #24801 ) ;
#2135 = FACE_OUTER_BOUND ( 'NONE', #25396, .T. ) ;
#2136 = DIRECTION ( 'NONE',  ( 0.000000000000000000, 0.000000000000000000, 1.000000000000000000 ) ) ;
#2137 = VERTEX_POINT ( 'NONE', #32257 ) ;
#2138 = ORIENTED_EDGE ( 'NONE', *, *, #47345, .F. ) ;
#2139 = ORIENTED_EDGE ( 'NONE', *, *, #37424, .T. ) ;
#2140 = DIRECTION ( 'NONE',  ( 0.000000000000000000, 0.000000000000000000, 1.000000000000000000 ) ) ;
#2142 = EDGE_LOOP ( 'NONE', ( #41342, #41173, #35536, #577 ) ) ;
#2141 = CYLINDRICAL_SURFACE ( 'NONE', #33688, 31.99999999999999289 ) ;
#2143 = VECTOR ( 'NONE', #6266, 1000.000000000000000 ) ;
#2144 = EDGE_CURVE ( 'NONE', #18005, #9046, #43272, .T. ) ;
#2145 = DIRECTION ( 'NONE',  ( -1.000000000000000000, -0.000000000000000000, -0.000000000000000000 ) ) ;
#2146 = VERTEX_POINT ( 'NONE', #42802 ) ;
#2147 = ORIENTED_EDGE ( 'NONE', *, *, #24145, .F. ) ;
#2148 = DIRECTION ( 'NONE',  ( -1.000000000000000000, 0.000000000000000000, 0.000000000000000000 ) ) ;
#2149 = VERTEX_POINT ( 'NONE', #47178 ) ;
#2150 = LINE ( 'NONE', #35423, #18106 ) ;
#2151 = DIRECTION ( 'NONE',  ( -1.000000000000000000, 0.000000000000000000, 0.000000000000000000 ) ) ;
#2152 = DIRECTION ( 'NONE',  ( -1.000000000000000000, 0.000000000000000000, 0.000000000000000000 ) ) ;
#2153 = CARTESIAN_POINT ( 'NONE',  ( 0.000000000000000000, 0.000000000000000000, 0.000000000000000000 ) ) ;
#2154 = CARTESIAN_POINT ( 'NONE',  ( 10.00000000000000000, 0.000000000000000000, 0.000000000000000000 ) ) ;
#2155 = ORIENTED_EDGE ( 'NONE', *, *, #14480, .T. ) ;
#2156 = CARTESIAN_POINT ( 'NONE',  ( 11.99999999999999822, 0.000000000000000000, 0.000000000000000000 ) ) ;
#2157 = DIRECTION ( 'NONE',  ( 0.000000000000000000, 0.4999999999999920064, 0.8660254037844432595 ) ) ;
#2158 = VERTEX_POINT ( 'NONE', #16363 ) ;
#2159 = EDGE_CURVE ( 'NONE', #12132, #38104, #28102, .T. ) ;
#2160 = DIRECTION ( 'NONE',  ( 0.000000000000000000, 1.000000000000000000, -9.787530781167596740E-16 ) ) ;
#2161 = VERTEX_POINT ( 'NONE', #13656 ) ;
#2162 = CARTESIAN_POINT ( 'NONE',  ( 10.00000000000000000, 44.99326035066052754, 68.55367621811160461 ) ) ;
#2164 = EDGE_CURVE ( 'NONE', #27718, #6779, #24673, .T. ) ;
#2163 = CIRCLE ( 'NONE', #3726, 16.00000000000000000 ) ;
#2165 = CYLINDRICAL_SURFACE ( 'NONE', #14614, 82.00000000000000000 ) ;
#2166 = CARTESIAN_POINT ( 'NONE',  ( 0.000000000000000000, -30.80686688397025108, 21.53537804866070715 ) ) ;
#2167 = CARTESIAN_POINT ( 'NONE',  ( 11.99999999999999822, 0.000000000000000000, 0.000000000000000000 ) ) ;
#2168 = EDGE_CURVE ( 'NONE', #30556, #30938, #7704, .T. ) ;
#2169 = DIRECTION ( 'NONE',  ( -0.000000000000000000, -2.312964634635746211E-15, 1.000000000000000000 ) ) ;
#2170 = ORIENTED_EDGE ( 'NONE', *, *, #24897, .F. ) ;
#2171 = DIRECTION ( 'NONE',  ( 0.000000000000000000, 0.000000000000000000, 1.000000000000000000 ) ) ;
#2172 = DIRECTION ( 'NONE',  ( 1.000000000000000000, 0.000000000000000000, 0.000000000000000000 ) ) ;
#2173 = CARTESIAN_POINT ( 'NONE',  ( 0.000000000000000000, 18.84667830672579925, 18.68964196561269020 ) ) ;
#2174 = EDGE_CURVE ( 'NONE', #19451, #30139, #42559, .T. ) ;
#2175 = DIRECTION ( 'NONE',  ( -1.000000000000000000, -0.000000000000000000, -0.000000000000000000 ) ) ;
#2176 = ORIENTED_EDGE ( 'NONE', *, *, #18779, .T. ) ;
#2177 = VERTEX_POINT ( 'NONE', #5589 ) ;
#2178 = AXIS2_PLACEMENT_3D ( 'NONE', #33411, #33880, #14811 ) ;
#2179 = ORIENTED_EDGE ( 'NONE', *, *, #915, .T. ) ;
#2180 = CARTESIAN_POINT ( 'NONE',  ( 0.000000000000000000, -67.80270845531855173, -46.11716303203260736 ) ) ;
#2181 = CARTESIAN_POINT ( 'NONE',  ( 10.00000000000000000, 0.000000000000000000, 0.000000000000000000 ) ) ;
#2182 = EDGE_LOOP ( 'NONE', ( #36448, #41682, #39832, #45012 ) ) ;
#2183 = VERTEX_POINT ( 'NONE', #6081 ) ;
#2184 = AXIS2_PLACEMENT_3D ( 'NONE', #20555, #23751, #27935 ) ;
#2185 = ADVANCED_FACE ( 'NONE', ( #1930 ), #23696, .T. ) ;
#2186 = CARTESIAN_POINT ( 'NONE',  ( 0.000000000000000000, -23.29833615347109443, 3.418703333116492438 ) ) ;
#2187 = VECTOR ( 'NONE', #3487, 1000.000000000000000 ) ;
#2188 = VERTEX_POINT ( 'NONE', #9487 ) ;
#2189 = VERTEX_POINT ( 'NONE', #38892 ) ;
#2190 = ORIENTED_EDGE ( 'NONE', *, *, #13426, .F. ) ;
#2191 = AXIS2_PLACEMENT_3D ( 'NONE', #17774, #25113, #43966 ) ;
#2192 = CARTESIAN_POINT ( 'NONE',  ( 0.000000000000000000, 0.000000000000000000, 53.20000000000001705 ) ) ;
#2193 = ORIENTED_EDGE ( 'NONE', *, *, #28126, .F. ) ;
#2194 = DIRECTION ( 'NONE',  ( -1.000000000000000000, -0.000000000000000000, -0.000000000000000000 ) ) ;
#2195 = ORIENTED_EDGE ( 'NONE', *, *, #33335, .F. ) ;
#2196 = DIRECTION ( 'NONE',  ( 0.000000000000000000, 0.000000000000000000, 1.000000000000000000 ) ) ;
#2197 = CARTESIAN_POINT ( 'NONE',  ( 11.99999999999999822, -50.23322058963300663, -64.81221759200398935 ) ) ;
#2198 = PRODUCT_DEFINITION_FORMATION_WITH_SPECIFIED_SOURCE ( 'ANY', '', #2652, .NOT_KNOWN. ) ;
#2199 = DIRECTION ( 'NONE',  ( 0.000000000000000000, 0.000000000000000000, 1.000000000000000000 ) ) ;
#2200 = VERTEX_POINT ( 'NONE', #1677 ) ;
#2201 = CARTESIAN_POINT ( 'NONE',  ( 11.99999999999999822, -26.01480285779785362, -70.53064760720343429 ) ) ;
#2202 = ORIENTED_EDGE ( 'NONE', *, *, #6000, .F. ) ;
#2203 = DIRECTION ( 'NONE',  ( -1.000000000000000000, 0.000000000000000000, 0.000000000000000000 ) ) ;
#2204 = DIRECTION ( 'NONE',  ( 0.000000000000000000, -0.5877852522924689183, 0.8090169943749504489 ) ) ;
#2205 = DIRECTION ( 'NONE',  ( 0.000000000000000000, -0.8660254037844432595, 0.4999999999999919509 ) ) ;
#2206 = ORIENTED_EDGE ( 'NONE', *, *, #36006, .F. ) ;
#2207 = ORIENTED_EDGE ( 'NONE', *, *, #11104, .F. ) ;
#2208 = EDGE_CURVE ( 'NONE', #5642, #32047, #20760, .T. ) ;
#2209 = DIRECTION ( 'NONE',  ( 0.6691306063588671194, -0.7431448254773862505, 0.000000000000000000 ) ) ;
#2210 = FACE_OUTER_BOUND ( 'NONE', #6578, .T. ) ;
#2211 = VERTEX_POINT ( 'NONE', #46473 ) ;
#2212 = CARTESIAN_POINT ( 'NONE',  ( 10.00000000000000000, -25.88420570971381807, -27.13269053701123212 ) ) ;
#2213 = DIRECTION ( 'NONE',  ( 0.000000000000000000, 0.000000000000000000, 1.000000000000000000 ) ) ;
#2214 = DIRECTION ( 'NONE',  ( -1.000000000000000000, -0.000000000000000000, -0.000000000000000000 ) ) ;
#2215 = EDGE_CURVE ( 'NONE', #10144, #29882, #21222, .T. ) ;
#2216 = DIRECTION ( 'NONE',  ( -1.000000000000000000, 0.000000000000000000, -0.000000000000000000 ) ) ;
#2217 = DIRECTION ( 'NONE',  ( -1.000000000000000000, 0.000000000000000000, -0.000000000000000000 ) ) ;
#2218 = FACE_OUTER_BOUND ( 'NONE', #45782, .T. ) ;
#2219 = CARTESIAN_POINT ( 'NONE',  ( 0.000000000000000000, -62.20884554314051940, 46.21855187248608132 ) ) ;
#2220 = EDGE_CURVE ( 'NONE', #2211, #48416, #47889, .T. ) ;
#2221 = VECTOR ( 'NONE', #35904, 1000.000000000000000 ) ;
#2222 = ADVANCED_FACE ( 'NONE', ( #43748 ), #47424, .T. ) ;
#2223 = CARTESIAN_POINT ( 'NONE',  ( -8.826826895187510402, -94.96827758698185562, 5.500000000000000000 ) ) ;
#2224 = CARTESIAN_POINT ( 'NONE',  ( 0.000000000000000000, -50.23322058963393744, 64.81221759200325039 ) ) ;
#2225 = DIRECTION ( 'NONE',  ( 0.000000000000000000, 0.6494480483301793283, 0.7604059656000345946 ) ) ;
#2226 = CARTESIAN_POINT ( 'NONE',  ( 0.000000000000000000, 74.65491531819105830, 8.830959090343693418 ) ) ;
#2227 = ORIENTED_EDGE ( 'NONE', *, *, #48094, .F. ) ;
#2228 = FACE_OUTER_BOUND ( 'NONE', #42464, .T. ) ;
#2229 = DIRECTION ( 'NONE',  ( -1.000000000000000000, 0.000000000000000000, 0.000000000000000000 ) ) ;
#2230 = EDGE_CURVE ( 'NONE', #20992, #23445, #26478, .T. ) ;
#2231 = DIRECTION ( 'NONE',  ( -1.000000000000000000, 0.000000000000000000, -0.000000000000000000 ) ) ;
#2232 = ORIENTED_EDGE ( 'NONE', *, *, #18522, .T. ) ;
#2233 = AXIS2_PLACEMENT_3D ( 'NONE', #23529, #8371, #1010 ) ;
#2234 = ORIENTED_EDGE ( 'NONE', *, *, #5363, .F. ) ;
#2235 = LINE ( 'NONE', #32114, #33592 ) ;
#2236 = FACE_OUTER_BOUND ( 'NONE', #34205, .T. ) ;
#2237 = VERTEX_POINT ( 'NONE', #47646 ) ;
#2238 = DIRECTION ( 'NONE',  ( 0.000000000000000000, 1.000000000000000000, 3.491481338843133355E-15 ) ) ;
#2239 = ADVANCED_FACE ( 'NONE', ( #18028 ), #14134, .T. ) ;
#2240 = DIRECTION ( 'NONE',  ( -1.000000000000000000, 0.000000000000000000, -0.000000000000000000 ) ) ;
#2241 = LINE ( 'NONE', #47040, #17217 ) ;
#2242 = EDGE_LOOP ( 'NONE', ( #20469, #42787, #38973, #38945 ) ) ;
#2244 = ORIENTED_EDGE ( 'NONE', *, *, #43733, .F. ) ;
#2243 = CARTESIAN_POINT ( 'NONE',  ( 0.000000000000000000, -37.58145647212455032, 16.68533520207890319 ) ) ;
#2245 = EDGE_CURVE ( 'NONE', #28305, #45131, #18530, .T. ) ;
#2246 = EDGE_LOOP ( 'NONE', ( #47863, #36567, #44691, #17829 ) ) ;
#2247 = AXIS2_PLACEMENT_3D ( 'NONE', #27407, #16623, #38675 ) ;
#2248 = AXIS2_PLACEMENT_3D ( 'NONE', #29311, #40801, #25137 ) ;
#2249 = AXIS2_PLACEMENT_3D ( 'NONE', #29811, #906, #18783 ) ;
#2250 = DIRECTION ( 'NONE',  ( 0.000000000000000000, 0.000000000000000000, 1.000000000000000000 ) ) ;
#2251 = EDGE_CURVE ( 'NONE', #46736, #9579, #39845, .T. ) ;
#2252 = DIRECTION ( 'NONE',  ( 1.000000000000000000, -0.000000000000000000, -0.000000000000000000 ) ) ;
#2253 = CARTESIAN_POINT ( 'NONE',  ( 10.00000000000000000, 0.000000000000000000, 0.000000000000000000 ) ) ;
#2254 = DIRECTION ( 'NONE',  ( 0.000000000000000000, 0.000000000000000000, 1.000000000000000000 ) ) ;
#2255 = FACE_OUTER_BOUND ( 'NONE', #46402, .T. ) ;
#2256 = ORIENTED_EDGE ( 'NONE', *, *, #33435, .T. ) ;
#2257 = DIRECTION ( 'NONE',  ( 1.000000000000000000, -0.000000000000000000, 0.000000000000000000 ) ) ;
#2258 = ORIENTED_EDGE ( 'NONE', *, *, #39282, .T. ) ;
#2259 = ORIENTED_EDGE ( 'NONE', *, *, #8192, .F. ) ;
#2260 = DIRECTION ( 'NONE',  ( 0.000000000000000000, 0.000000000000000000, -1.000000000000000000 ) ) ;
#2261 = CYLINDRICAL_SURFACE ( 'NONE', #40278, 31.99999999999999289 ) ;
#2262 = DIRECTION ( 'NONE',  ( 0.000000000000000000, 0.000000000000000000, 1.000000000000000000 ) ) ;
#2263 = LINE ( 'NONE', #6429, #35223 ) ;
#2264 = ORIENTED_EDGE ( 'NONE', *, *, #13477, .T. ) ;
#2265 = LINE ( 'NONE', #1793, #10486 ) ;
#2266 = PRODUCT_DEFINITION_SHAPE ( 'NONE', 'NONE',  #10069 ) ;
#2267 = ADVANCED_FACE ( 'NONE', ( #6546 ), #14630, .F. ) ;
#2268 = CARTESIAN_POINT ( 'NONE',  ( 10.00000000000000000, 31.52238457039638320, -27.75498641678709788 ) ) ;
#2269 = ADVANCED_FACE ( 'NONE', ( #6312 ), #43989, .T. ) ;
#2270 = EDGE_CURVE ( 'NONE', #28609, #13398, #31979, .T. ) ;
#2271 = CARTESIAN_POINT ( 'NONE',  ( 10.00000000000000000, 16.65972982745046238, -80.28980883073739960 ) ) ;
#2272 = CARTESIAN_POINT ( 'NONE',  ( 0.000000000000000000, 21.53537804866126137, -30.80686688396986028 ) ) ;
#2273 = CARTESIAN_POINT ( 'NONE',  ( 10.00000000000000000, -35.95386929396264009, 10.96151621346475658 ) ) ;
#2274 = CARTESIAN_POINT ( 'NONE',  ( 4.999999999999999112, 40.68715046381943523, -10.41901085202036370 ) ) ;
#2275 = CARTESIAN_POINT ( 'NONE',  ( 5.000000000000000000, -64.81221759200379040, 50.23322058963324110 ) ) ;
#2276 = CARTESIAN_POINT ( 'NONE',  ( 10.00000000000000000, 11.30684508768339569, 76.66974797899841576 ) ) ;
#2277 = CARTESIAN_POINT ( 'NONE',  ( 10.00000000000000000, -81.34940948281328588, -10.30890764327469711 ) ) ;
#2278 = ORIENTED_EDGE ( 'NONE', *, *, #16209, .F. ) ;
#2279 = ADVANCED_FACE ( 'NONE', ( #14861 ), #28817, .T. ) ;
#2280 = DIRECTION ( 'NONE',  ( -0.000000000000000000, -0.3090169943749572767, -0.9510565162951503115 ) ) ;
#2281 = DIRECTION ( 'NONE',  ( -1.000000000000000000, 0.000000000000000000, 0.000000000000000000 ) ) ;
#2282 = ORIENTED_EDGE ( 'NONE', *, *, #36480, .F. ) ;
#2283 = FACE_OUTER_BOUND ( 'NONE', #46818, .T. ) ;
#2284 = AXIS2_PLACEMENT_3D ( 'NONE', #15606, #674, #37395 ) ;
#2285 = ORIENTED_EDGE ( 'NONE', *, *, #17271, .F. ) ;
#2286 = DIRECTION ( 'NONE',  ( 1.000000000000000000, 0.000000000000000000, 0.000000000000000000 ) ) ;
#2287 = CIRCLE ( 'NONE', #14031, 16.00000000000000000 ) ;
#2288 = EDGE_CURVE ( 'NONE', #27398, #10618, #27243, .T. ) ;
#2289 = LINE ( 'NONE', #43425, #13510 ) ;
#2290 = VERTEX_POINT ( 'NONE', #36874 ) ;
#2291 = AXIS2_PLACEMENT_3D ( 'NONE', #3760, #29701, #13640 ) ;
#2292 = DIRECTION ( 'NONE',  ( -1.000000000000000000, 0.000000000000000000, 0.000000000000000000 ) ) ;
#2293 = ORIENTED_EDGE ( 'NONE', *, *, #24648, .F. ) ;
#2294 = ORIENTED_EDGE ( 'NONE', *, *, #27474, .F. ) ;
#2295 = VERTEX_POINT ( 'NONE', #29544 ) ;
#2296 = ORIENTED_EDGE ( 'NONE', *, *, #3696, .F. ) ;
#2297 = EDGE_CURVE ( 'NONE', #28640, #13942, #29779, .T. ) ;
#2298 = EDGE_CURVE ( 'NONE', #34199, #30446, #21715, .T. ) ;
#2299 = CARTESIAN_POINT ( 'NONE',  ( 10.00000000000000000, -63.18004540533059554, 44.88180994100355292 ) ) ;
#2300 = ORIENTED_EDGE ( 'NONE', *, *, #35031, .F. ) ;
#2301 = DIRECTION ( 'NONE',  ( 0.6862798483830554463, 0.7273375899149793211, -0.000000000000000000 ) ) ;
#2302 = LINE ( 'NONE', #9897, #9762 ) ;
#2303 = EDGE_CURVE ( 'NONE', #42424, #20927, #48337, .T. ) ;
#2304 = VERTEX_POINT ( 'NONE', #14378 ) ;
#2305 = DIRECTION ( 'NONE',  ( -1.000000000000000000, -0.000000000000000000, -0.000000000000000000 ) ) ;
#2306 = EDGE_CURVE ( 'NONE', #18510, #27706, #10044, .T. ) ;
#2307 = EDGE_LOOP ( 'NONE', ( #44490, #15744, #34396, #3995 ) ) ;
#2308 = EDGE_LOOP ( 'NONE', ( #5853, #44401, #47795, #2658 ) ) ;
#2309 = DIRECTION ( 'NONE',  ( -1.000000000000000000, -0.000000000000000000, -0.000000000000000000 ) ) ;
#2310 = CARTESIAN_POINT ( 'NONE',  ( -2.500000000000000000, 16.00000000000000000, 0.000000000000000000 ) ) ;
#2311 = CARTESIAN_POINT ( 'NONE',  ( 10.00000000000000000, 0.000000000000000000, 0.000000000000000000 ) ) ;
#2312 = VECTOR ( 'NONE', #45083, 1000.000000000000000 ) ;
#2313 = ORIENTED_EDGE ( 'NONE', *, *, #46643, .T. ) ;
#2314 = CARTESIAN_POINT ( 'NONE',  ( 0.000000000000000000, -51.03279382321048985, -55.19960302592120627 ) ) ;
#2315 = ORIENTED_EDGE ( 'NONE', *, *, #38930, .T. ) ;
#2316 = DIRECTION ( 'NONE',  ( 1.000000000000000000, 0.000000000000000000, 0.000000000000000000 ) ) ;
#2317 = VECTOR ( 'NONE', #42886, 999.9999999999998863 ) ;
#2318 = LINE ( 'NONE', #46395, #15226 ) ;
#2319 = CARTESIAN_POINT ( 'NONE',  ( 10.00000000000000000, -71.91182617369207719, 28.89263327155721228 ) ) ;
#2320 = DIRECTION ( 'NONE',  ( -1.000000000000000000, 0.000000000000000000, 0.000000000000000000 ) ) ;
#2321 = CARTESIAN_POINT ( 'NONE',  ( 0.000000000000000000, -20.40083707022829174, -72.35432306680507963 ) ) ;
#2322 = PLANE ( 'NONE',  #39410 ) ;
#2323 = ADVANCED_FACE ( 'NONE', ( #40083 ), #2870, .T. ) ;
#2324 = EDGE_CURVE ( 'NONE', #8879, #35187, #37372, .T. ) ;
#2325 = CYLINDRICAL_SURFACE ( 'NONE', #3932, 31.99999999999998579 ) ;
#2326 = CARTESIAN_POINT ( 'NONE',  ( 10.00000000000000000, 17.80606268964585226, -33.00180498840028775 ) ) ;
#2327 = LINE ( 'NONE', #13354, #3287 ) ;
#2328 = DIRECTION ( 'NONE',  ( 0.000000000000000000, 0.000000000000000000, -1.000000000000000000 ) ) ;
#2329 = ORIENTED_EDGE ( 'NONE', *, *, #13700, .T. ) ;
#2330 = AXIS2_PLACEMENT_3D ( 'NONE', #6415, #14236, #21331 ) ;
#2331 = DIRECTION ( 'NONE',  ( -1.000000000000000000, 0.000000000000000000, -0.000000000000000000 ) ) ;
#2332 = DIRECTION ( 'NONE',  ( -1.000000000000000000, -0.000000000000000000, 0.000000000000000000 ) ) ;
#2333 = LINE ( 'NONE', #21415, #40946 ) ;
#2334 = CARTESIAN_POINT ( 'NONE',  ( 10.00000000000000000, -0.8828120875898013420, -37.48860685352291711 ) ) ;
#2335 = EDGE_CURVE ( 'NONE', #27708, #2670, #24164, .T. ) ;
#2336 = ORIENTED_EDGE ( 'NONE', *, *, #22217, .T. ) ;
#2337 = DIRECTION ( 'NONE',  ( 1.000000000000000000, 0.000000000000000000, 0.000000000000000000 ) ) ;
#2338 = CARTESIAN_POINT ( 'NONE',  ( 15.00000000000000000, -13.04903810567646971, 19.60159698893442481 ) ) ;
#2339 = VERTEX_POINT ( 'NONE', #34177 ) ;
#2340 = DIRECTION ( 'NONE',  ( -1.000000000000000000, 0.000000000000000000, 0.000000000000000000 ) ) ;
#2341 = ORIENTED_EDGE ( 'NONE', *, *, #2355, .T. ) ;
#2342 = FACE_OUTER_BOUND ( 'NONE', #17769, .T. ) ;
#2343 = ORIENTED_EDGE ( 'NONE', *, *, #9334, .T. ) ;
#2344 = ORIENTED_EDGE ( 'NONE', *, *, #17071, .F. ) ;
#2345 = VECTOR ( 'NONE', #11005, 1000.000000000000000 ) ;
#2346 = AXIS2_PLACEMENT_3D ( 'NONE', #28253, #47349, #2530 ) ;
#2347 = CARTESIAN_POINT ( 'NONE',  ( -10.90473778262209414, 1.679381574647996852E-15, 13.71319123046128752 ) ) ;
#2348 = EDGE_LOOP ( 'NONE', ( #46876, #24503, #36334, #14177 ) ) ;
#2349 = AXIS2_PLACEMENT_3D ( 'NONE', #29628, #14221, #36491 ) ;
#2350 = CIRCLE ( 'NONE', #6283, 82.00000000000000000 ) ;
#2351 = AXIS2_PLACEMENT_3D ( 'NONE', #28384, #6124, #24724 ) ;
#2352 = FACE_OUTER_BOUND ( 'NONE', #44491, .T. ) ;
#2354 = EDGE_LOOP ( 'NONE', ( #23080, #740, #45841, #45075 ) ) ;
#2353 = DIRECTION ( 'NONE',  ( -0.9435911131814395114, 0.3311129884571304971, 0.000000000000000000 ) ) ;
#2355 = EDGE_CURVE ( 'NONE', #14655, #4757, #32743, .T. ) ;
#2356 = EDGE_LOOP ( 'NONE', ( #8, #42729, #13824, #11043 ) ) ;
#2357 = ORIENTED_EDGE ( 'NONE', *, *, #2930, .T. ) ;
#2358 = ORIENTED_EDGE ( 'NONE', *, *, #26413, .T. ) ;
#2359 = EDGE_CURVE ( 'NONE', #32670, #21593, #17889, .T. ) ;
#2360 = CARTESIAN_POINT ( 'NONE',  ( 25.81725066941077884, -113.8380548628854854, 2.500000000000000000 ) ) ;
#2361 = DIRECTION ( 'NONE',  ( -0.9918136447140101231, 0.1276937514489694114, 0.000000000000000000 ) ) ;
#2362 = CARTESIAN_POINT ( 'NONE',  ( -10.00000000000000000, 0.000000000000000000, 0.000000000000000000 ) ) ;
#2363 = VERTEX_POINT ( 'NONE', #15579 ) ;
#2364 = ORIENTED_EDGE ( 'NONE', *, *, #18495, .F. ) ;
#2365 = DIRECTION ( 'NONE',  ( 0.000000000000000000, 0.1564344650402311743, -0.9876883405951377704 ) ) ;
#2366 = EDGE_LOOP ( 'NONE', ( #3065, #34999, #25909, #24829 ) ) ;
#2367 = DIRECTION ( 'NONE',  ( -1.000000000000000000, -0.000000000000000000, -0.000000000000000000 ) ) ;
#2368 = LINE ( 'NONE', #43975, #11627 ) ;
#2369 = LINE ( 'NONE', #29046, #9614 ) ;
#2370 = CARTESIAN_POINT ( 'NONE',  ( 0.000000000000000000, -75.11764819372145041, 29.05362095685286050 ) ) ;
#2371 = FACE_OUTER_BOUND ( 'NONE', #22591, .T. ) ;
#2372 = ADVANCED_FACE ( 'NONE', ( #30511 ), #30031, .F. ) ;
#2373 = EDGE_CURVE ( 'NONE', #47251, #10794, #24929, .T. ) ;
#2374 = DIRECTION ( 'NONE',  ( -1.000000000000000000, 0.000000000000000000, -0.000000000000000000 ) ) ;
#2375 = CIRCLE ( 'NONE', #44593, 42.00000000000000000 ) ;
#2376 = DIRECTION ( 'NONE',  ( 0.000000000000000000, 0.9876883405951372152, 0.1564344650402347547 ) ) ;
#2377 = ORIENTED_EDGE ( 'NONE', *, *, #24833, .T. ) ;
#2378 = VECTOR ( 'NONE', #21321, 999.9999999999998863 ) ;
#2379 = EDGE_CURVE ( 'NONE', #22588, #38490, #22453, .T. ) ;
#2380 = DIRECTION ( 'NONE',  ( -1.000000000000000000, 0.000000000000000000, -0.000000000000000000 ) ) ;
#2381 = ORIENTED_EDGE ( 'NONE', *, *, #17686, .T. ) ;
#2382 = CIRCLE ( 'NONE', #8631, 42.00000000000000000 ) ;
#2383 = CARTESIAN_POINT ( 'NONE',  ( -3.000000000000000000, -3.948201729842348850, 23.21447184625293048 ) ) ;
#2384 = CARTESIAN_POINT ( 'NONE',  ( 10.00000000000000000, 0.000000000000000000, 0.000000000000000000 ) ) ;
#2385 = CARTESIAN_POINT ( 'NONE',  ( 10.00000000000000000, 33.17418723428307459, 17.67226234102837878 ) ) ;
#2386 = DIRECTION ( 'NONE',  ( 0.000000000000000000, -1.000000000000000000, -1.040834085586084730E-14 ) ) ;
#2387 = ORIENTED_EDGE ( 'NONE', *, *, #14321, .F. ) ;
#2388 = DIRECTION ( 'NONE',  ( 0.000000000000000000, -0.8910065241883626808, -0.4539904997395569075 ) ) ;
#2389 = DIRECTION ( 'NONE',  ( 0.000000000000000000, 0.000000000000000000, 1.000000000000000000 ) ) ;
#2390 = EDGE_CURVE ( 'NONE', #40544, #30527, #3829, .T. ) ;
#2391 = ORIENTED_EDGE ( 'NONE', *, *, #33210, .F. ) ;
#2392 = LINE ( 'NONE', #17316, #41983 ) ;
#2393 = AXIS2_PLACEMENT_3D ( 'NONE', #2429, #31848, #46521 ) ;
#2394 = CARTESIAN_POINT ( 'NONE',  ( -3.000000000000000000, 26.50000000000000000, -1.500000000000001332 ) ) ;
#2395 = DIRECTION ( 'NONE',  ( 0.000000000000000000, -0.8910065241883722287, 0.4539904997395382558 ) ) ;
#2396 = CARTESIAN_POINT ( 'NONE',  ( 10.00000000000000000, 20.41045688087930898, -72.35160999960793049 ) ) ;
#2397 = ORIENTED_EDGE ( 'NONE', *, *, #36484, .T. ) ;
#2398 = VERTEX_POINT ( 'NONE', #22677 ) ;
#2399 = ORIENTED_EDGE ( 'NONE', *, *, #18220, .T. ) ;
#2400 = DIRECTION ( 'NONE',  ( -1.000000000000000000, 0.000000000000000000, 0.000000000000000000 ) ) ;
#2401 = LINE ( 'NONE', #25400, #23012 ) ;
#2402 = ORIENTED_EDGE ( 'NONE', *, *, #29275, .F. ) ;
#2403 = VECTOR ( 'NONE', #44413, 999.9999999999998863 ) ;
#2404 = CONICAL_SURFACE ( 'NONE', #37611, 15.39727592608509177, 1.361356816555577609 ) ;
#2405 = EDGE_CURVE ( 'NONE', #20033, #27870, #28836, .T. ) ;
#2406 = LINE ( 'NONE', #23985, #37436 ) ;
#2407 = VECTOR ( 'NONE', #1316, 1000.000000000000000 ) ;
#2408 = CIRCLE ( 'NONE', #35224, 42.00000000000000000 ) ;
#2409 = EDGE_CURVE ( 'NONE', #3237, #37330, #13988, .T. ) ;
#2410 = VERTEX_POINT ( 'NONE', #12172 ) ;
#2411 = ORIENTED_EDGE ( 'NONE', *, *, #13766, .F. ) ;
#2412 = ORIENTED_EDGE ( 'NONE', *, *, #34145, .F. ) ;
#2413 = ADVANCED_FACE ( 'NONE', ( #41775 ), #411, .F. ) ;
#2414 = EDGE_CURVE ( 'NONE', #2183, #8188, #12230, .T. ) ;
#2415 = CIRCLE ( 'NONE', #25101, 31.99999999999999289 ) ;
#2416 = ADVANCED_FACE ( 'NONE', ( #41298 ), #4567, .T. ) ;
#2417 = DIRECTION ( 'NONE',  ( -1.000000000000000000, -0.000000000000000000, -0.000000000000000000 ) ) ;
#2418 = EDGE_CURVE ( 'NONE', #12188, #11742, #2803, .T. ) ;
#2419 = AXIS2_PLACEMENT_3D ( 'NONE', #11238, #15624, #19764 ) ;
#2420 = ORIENTED_EDGE ( 'NONE', *, *, #13114, .F. ) ;
#2421 = DIRECTION ( 'NONE',  ( 0.000000000000000000, 0.07845909572784530439, -0.9969173337331279638 ) ) ;
#2422 = EDGE_CURVE ( 'NONE', #18553, #25783, #42693, .T. ) ;
#2423 = VERTEX_POINT ( 'NONE', #16075 ) ;
#2424 = CARTESIAN_POINT ( 'NONE',  ( 10.00000000000000000, -30.41916302227164337, 71.27951684758015460 ) ) ;
#2425 = CARTESIAN_POINT ( 'NONE',  ( 0.000000000000000000, -73.44644590900043113, -24.73286445877782924 ) ) ;
#2426 = DIRECTION ( 'NONE',  ( 0.000000000000000000, 0.000000000000000000, 1.000000000000000000 ) ) ;
#2427 = DIRECTION ( 'NONE',  ( 0.000000000000000000, 0.000000000000000000, -1.000000000000000000 ) ) ;
#2428 = ORIENTED_EDGE ( 'NONE', *, *, #17993, .F. ) ;
#2429 = CARTESIAN_POINT ( 'NONE',  ( 10.00000000000000000, 26.08949754953024325, 27.05870788708241648 ) ) ;
#2430 = CARTESIAN_POINT ( 'NONE',  ( 10.00000000000000000, 0.000000000000000000, 0.000000000000000000 ) ) ;
#2431 = ORIENTED_EDGE ( 'NONE', *, *, #6410, .T. ) ;
#2432 = EDGE_LOOP ( 'NONE', ( #42071, #36793, #3083, #5232 ) ) ;
#2433 = ADVANCED_FACE ( 'NONE', ( #11187 ), #26113, .T. ) ;
#2434 = CARTESIAN_POINT ( 'NONE',  ( 11.99999999999999822, -71.91182617369207719, 28.89263327155721228 ) ) ;
#2435 = CARTESIAN_POINT ( 'NONE',  ( 10.00000000000000000, 37.58145647212453611, 0.6853352020791767529 ) ) ;
#2436 = ORIENTED_EDGE ( 'NONE', *, *, #42893, .T. ) ;
#2437 = LINE ( 'NONE', #21045, #35509 ) ;
#2438 = DIRECTION ( 'NONE',  ( -1.000000000000000000, 0.000000000000000000, 0.000000000000000000 ) ) ;
#2439 = LINE ( 'NONE', #17138, #19019 ) ;
#2440 = VERTEX_POINT ( 'NONE', #38587 ) ;
#2441 = CARTESIAN_POINT ( 'NONE',  ( -10.00000000000000000, 0.000000000000000000, 0.000000000000000000 ) ) ;
#2442 = MANIFOLD_SOLID_BREP ( 'Cut-Extrude-Thin1', #16878 ) ;
#2444 = AXIS2_PLACEMENT_3D ( 'NONE', #43405, #2751, #17684 ) ;
#2443 = DIRECTION ( 'NONE',  ( 0.000000000000000000, -0.8090169943749402348, -0.5877852522924830181 ) ) ;
#2445 = EDGE_CURVE ( 'NONE', #36248, #6463, #16891, .T. ) ;
#2446 = CIRCLE ( 'NONE', #40750, 82.00000000000000000 ) ;
#2447 = CARTESIAN_POINT ( 'NONE',  ( 10.00000000000000000, 22.64427369931169309, 30.00120703465213623 ) ) ;
#2448 = DIRECTION ( 'NONE',  ( 0.000000000000000000, 0.7071067811865436870, 0.7071067811865513475 ) ) ;
#2449 = AXIS2_PLACEMENT_3D ( 'NONE', #22440, #23156, #15812 ) ;
#2450 = AXIS2_PLACEMENT_3D ( 'NONE', #30011, #22429, #7501 ) ;
#2451 = CARTESIAN_POINT ( 'NONE',  ( -10.00000000000000000, 0.000000000000000000, 0.000000000000000000 ) ) ;
#2452 = DIRECTION ( 'NONE',  ( -1.000000000000000000, 0.000000000000000000, 0.000000000000000000 ) ) ;
#2453 = EDGE_CURVE ( 'NONE', #13341, #27075, #29400, .T. ) ;
#2454 = DIRECTION ( 'NONE',  ( 0.000000000000000000, 0.000000000000000000, 1.000000000000000000 ) ) ;
#2455 = DIRECTION ( 'NONE',  ( 1.000000000000000000, 0.000000000000000000, 0.000000000000000000 ) ) ;
#2456 = VECTOR ( 'NONE', #28329, 1000.000000000000000 ) ;
#2457 = VERTEX_POINT ( 'NONE', #16795 ) ;
#2458 = ORIENTED_EDGE ( 'NONE', *, *, #31194, .F. ) ;
#2459 = ADVANCED_FACE ( 'NONE', ( #1383 ), #16309, .F. ) ;
#2460 = DIRECTION ( 'NONE',  ( 0.000000000000000000, -0.4539904997395540764, 0.8910065241883642351 ) ) ;
#2461 = AXIS2_PLACEMENT_3D ( 'NONE', #3445, #47737, #22306 ) ;
#2462 = ITEM_DEFINED_TRANSFORMATION ( 'NONE', 'NONE', #38188,  #11636 ) ;
#2463 = DIRECTION ( 'NONE',  ( 0.000000000000000000, -0.9723699203976740035, -0.2334453638559160216 ) ) ;
#2464 = ORIENTED_EDGE ( 'NONE', *, *, #25636, .F. ) ;
#2465 = ADVANCED_FACE ( 'NONE', ( #5778 ), #12882, .T. ) ;
#2466 = EDGE_CURVE ( 'NONE', #17380, #7163, #17650, .T. ) ;
#2467 = DIRECTION ( 'NONE',  ( -1.000000000000000000, 0.000000000000000000, 0.000000000000000000 ) ) ;
#2468 = ORIENTED_EDGE ( 'NONE', *, *, #48139, .T. ) ;
#2469 = DIRECTION ( 'NONE',  ( 0.000000000000000000, 0.8090169943749426773, 0.5877852522924797984 ) ) ;
#2470 = ORIENTED_EDGE ( 'NONE', *, *, #12597, .T. ) ;
#2472 = EDGE_CURVE ( 'NONE', #22056, #34741, #12989, .T. ) ;
#2471 = SURFACE_SIDE_STYLE ('',( #25214 ) ) ;
#2473 = AXIS2_PLACEMENT_3D ( 'NONE', #37858, #22920, #26119 ) ;
#2474 = ORIENTED_EDGE ( 'NONE', *, *, #22154, .F. ) ;
#2475 = CARTESIAN_POINT ( 'NONE',  ( -3.000000000000000000, 9.615535125378775305, 24.73947219025917121 ) ) ;
#2476 = AXIS2_PLACEMENT_3D ( 'NONE', #31661, #35304, #46580 ) ;
#2477 = EDGE_CURVE ( 'NONE', #24169, #36004, #27329, .T. ) ;
#2478 = PLANE ( 'NONE',  #10175 ) ;
#2479 = ORIENTED_EDGE ( 'NONE', *, *, #34455, .F. ) ;
#2480 = CARTESIAN_POINT ( 'NONE',  ( 0.000000000000000000, -19.89357724625003598, 12.59942793731059574 ) ) ;
#2481 = CIRCLE ( 'NONE', #35292, 31.99999999999999645 ) ;
#2482 = ORIENTED_EDGE ( 'NONE', *, *, #21255, .F. ) ;
#2483 = ORIENTED_EDGE ( 'NONE', *, *, #34708, .F. ) ;
#2484 = DIRECTION ( 'NONE',  ( -1.000000000000000000, -0.000000000000000000, -0.000000000000000000 ) ) ;
#2485 = AXIS2_PLACEMENT_3D ( 'NONE', #19707, #871, #42490 ) ;
#2486 = DIRECTION ( 'NONE',  ( 0.000000000000000000, -0.5224985647159560154, 0.8526401643540879594 ) ) ;
#2487 = LINE ( 'NONE', #36503, #14585 ) ;
#2489 = VERTEX_POINT ( 'NONE', #5298 ) ;
#2488 = CARTESIAN_POINT ( 'NONE',  ( 0.000000000000000000, 0.000000000000000000, 42.00000000000001421 ) ) ;
#2490 = CARTESIAN_POINT ( 'NONE',  ( 12.69589495141918611, -96.69089767102708777, 2.500000000000000000 ) ) ;
#2491 = ORIENTED_EDGE ( 'NONE', *, *, #25375, .F. ) ;
#2492 = CARTESIAN_POINT ( 'NONE',  ( 15.00000000000000000, 0.000000000000000000, 0.000000000000000000 ) ) ;
#2493 = ORIENTED_EDGE ( 'NONE', *, *, #41737, .T. ) ;
#2494 = ORIENTED_EDGE ( 'NONE', *, *, #6929, .F. ) ;
#2495 = CARTESIAN_POINT ( 'NONE',  ( -24.50849501662245800, -109.8101191361138831, 5.500000000000000000 ) ) ;
#2496 = ORIENTED_EDGE ( 'NONE', *, *, #17939, .T. ) ;
#2497 = VECTOR ( 'NONE', #6117, 1000.000000000000000 ) ;
#2498 = DIRECTION ( 'NONE',  ( 0.000000000000000000, -0.3090169943749349613, -0.9510565162951576390 ) ) ;
#2499 = CARTESIAN_POINT ( 'NONE',  ( 0.000000000000000000, -40.65526001592565564, -71.21200624218839437 ) ) ;
#2500 = DIRECTION ( 'NONE',  ( 1.000000000000000000, 0.000000000000000000, 0.000000000000000000 ) ) ;
#2501 = ORIENTED_EDGE ( 'NONE', *, *, #9994, .T. ) ;
#2502 = DIRECTION ( 'NONE',  ( 0.000000000000000000, 0.000000000000000000, -1.000000000000000000 ) ) ;
#2503 = CARTESIAN_POINT ( 'NONE',  ( 10.00000000000000000, 76.41127070299292257, -12.93880638057232346 ) ) ;
#2504 = CYLINDRICAL_SURFACE ( 'NONE', #39950, 82.00000000000000000 ) ;
#2505 = CARTESIAN_POINT ( 'NONE',  ( 10.00000000000000000, -10.30890764327324227, -81.34940948281347062 ) ) ;
#2506 = DIRECTION ( 'NONE',  ( 0.000000000000000000, -0.7431448254773878048, 0.6691306063588654540 ) ) ;
#2507 = CARTESIAN_POINT ( 'NONE',  ( 10.00000000000000000, 37.22597642581158084, 10.79786254984347593 ) ) ;
#2508 = DIRECTION ( 'NONE',  ( -1.000000000000000000, 0.000000000000000000, 0.000000000000000000 ) ) ;
#2509 = CARTESIAN_POINT ( 'NONE',  ( 10.00000000000000000, 33.79645857604513992, 16.45098606841138178 ) ) ;
#2510 = CARTESIAN_POINT ( 'NONE',  ( 12.50000000000000000, -107.5000000000000000, -2.500000000000000000 ) ) ;
#2511 = CARTESIAN_POINT ( 'NONE',  ( 10.00000000000000000, 3.925862922256160736, 41.81611651403863306 ) ) ;
#2512 = VECTOR ( 'NONE', #14808, 1000.000000000000000 ) ;
#2513 = EDGE_LOOP ( 'NONE', ( #8170, #45977, #18123, #18074 ) ) ;
#2514 = DIRECTION ( 'NONE',  ( -1.000000000000000000, -0.000000000000000000, -0.000000000000000000 ) ) ;
#2515 = ORIENTED_EDGE ( 'NONE', *, *, #24090, .T. ) ;
#2516 = DIRECTION ( 'NONE',  ( 0.000000000000000000, 0.000000000000000000, -1.000000000000000000 ) ) ;
#2517 = AXIS2_PLACEMENT_3D ( 'NONE', #12737, #12498, #39162 ) ;
#2518 = CARTESIAN_POINT ( 'NONE',  ( 10.00000000000000000, -0.8261519478425671803, -77.49459641780887864 ) ) ;
#2519 = CIRCLE ( 'NONE', #5680, 77.49900000000000944 ) ;
#2520 = ORIENTED_EDGE ( 'NONE', *, *, #23929, .T. ) ;
#2521 = AXIS2_PLACEMENT_3D ( 'NONE', #9215, #36117, #31761 ) ;
#2522 = DIRECTION ( 'NONE',  ( 1.000000000000000000, 0.000000000000000000, 0.000000000000000000 ) ) ;
#2523 = ORIENTED_EDGE ( 'NONE', *, *, #26572, .F. ) ;
#2524 = ADVANCED_FACE ( 'NONE', ( #24363 ), #35863, .T. ) ;
#2525 = ORIENTED_EDGE ( 'NONE', *, *, #41936, .F. ) ;
#2526 = EDGE_CURVE ( 'NONE', #17865, #43495, #23141, .T. ) ;
#2527 = LINE ( 'NONE', #25282, #256 ) ;
#2528 = ORIENTED_EDGE ( 'NONE', *, *, #37622, .T. ) ;
#2529 = EDGE_CURVE ( 'NONE', #6477, #34129, #8299, .T. ) ;
#2530 = DIRECTION ( 'NONE',  ( 0.000000000000000000, 0.9510565162951544194, -0.3090169943749446757 ) ) ;
#2531 = DIRECTION ( 'NONE',  ( -1.000000000000000000, -0.000000000000000000, -0.000000000000000000 ) ) ;
#2532 = CIRCLE ( 'NONE', #47890, 37.49900000000000233 ) ;
#2533 = ORIENTED_EDGE ( 'NONE', *, *, #39317, .F. ) ;
#2534 = CARTESIAN_POINT ( 'NONE',  ( 10.00000000000000000, 0.8828120875905820508, -37.48860685352290290 ) ) ;
#2535 = EDGE_CURVE ( 'NONE', #1277, #21018, #31769, .T. ) ;
#2536 = VECTOR ( 'NONE', #33591, 1000.000000000000000 ) ;
#2537 = ORIENTED_EDGE ( 'NONE', *, *, #3962, .F. ) ;
#2538 = ORIENTED_EDGE ( 'NONE', *, *, #20611, .F. ) ;
#2539 = FACE_OUTER_BOUND ( 'NONE', #20569, .T. ) ;
#2540 = DIRECTION ( 'NONE',  ( 1.000000000000000000, 0.000000000000000000, 0.000000000000000000 ) ) ;
#2541 = CARTESIAN_POINT ( 'NONE',  ( 10.00000000000000000, 0.000000000000000000, 0.000000000000000000 ) ) ;
#2542 = VECTOR ( 'NONE', #33099, 1000.000000000000000 ) ;
#2543 = AXIS2_PLACEMENT_3D ( 'NONE', #46396, #34889, #31002 ) ;
#2544 = ORIENTED_EDGE ( 'NONE', *, *, #3300, .T. ) ;
#2545 = DIRECTION ( 'NONE',  ( -1.000000000000000000, 0.000000000000000000, -0.000000000000000000 ) ) ;
#2546 = EDGE_LOOP ( 'NONE', ( #7119, #30843, #11967, #43447, #31695, #20805, #22594, #33669 ) ) ;
#2547 = EDGE_LOOP ( 'NONE', ( #1396, #40468, #33772, #12585 ) ) ;
#2548 = CIRCLE ( 'NONE', #43200, 32.00000000000000000 ) ;
#2549 = CARTESIAN_POINT ( 'NONE',  ( 11.99999999999999822, -44.99326035066006568, -68.55367621811190304 ) ) ;
#2550 = ADVANCED_FACE ( 'NONE', ( #38839 ), #46660, .T. ) ;
#2551 = CARTESIAN_POINT ( 'NONE',  ( -22.67106064244953245, -113.6342314410295842, -5.500000000000000000 ) ) ;
#2552 = CARTESIAN_POINT ( 'NONE',  ( 10.00000000000000000, 0.000000000000000000, 0.000000000000000000 ) ) ;
#2553 = CARTESIAN_POINT ( 'NONE',  ( 10.00000000000000000, -0.8828120875903202602, 37.48860685352291000 ) ) ;
#2554 = DIRECTION ( 'NONE',  ( 0.000000000000000000, 0.6691306063588670083, 0.7431448254773863615 ) ) ;
#2555 = VECTOR ( 'NONE', #23229, 1000.000000000000000 ) ;
#2556 = LINE ( 'NONE', #12874, #11941 ) ;
#2557 = CARTESIAN_POINT ( 'NONE',  ( 11.99999999999999822, 41.76106447765489094, 62.50884508063442269 ) ) ;
#2558 = DIRECTION ( 'NONE',  ( -1.000000000000000000, -0.000000000000000000, -0.000000000000000000 ) ) ;
#2559 = CARTESIAN_POINT ( 'NONE',  ( 10.00000000000000000, 18.89407956138362010, -75.16055320797013906 ) ) ;
#2560 = DIRECTION ( 'NONE',  ( -0.000000000000000000, 0.9781476007338042455, 0.2079116908177664758 ) ) ;
#2561 = ORIENTED_EDGE ( 'NONE', *, *, #33033, .F. ) ;
#2562 = AXIS2_PLACEMENT_3D ( 'NONE', #13062, #28462, #42682 ) ;
#2563 = ORIENTED_EDGE ( 'NONE', *, *, #27214, .T. ) ;
#2564 = CARTESIAN_POINT ( 'NONE',  ( 10.00000000000000000, 62.50884508063487033, -41.76106447765422303 ) ) ;
#2565 = CIRCLE ( 'NONE', #219, 77.49899999999999523 ) ;
#2566 = FACE_OUTER_BOUND ( 'NONE', #29309, .T. ) ;
#2567 = DIRECTION ( 'NONE',  ( 0.000000000000000000, 0.9135454576426063067, -0.4067366430757881068 ) ) ;
#2568 = ADVANCED_FACE ( 'NONE', ( #17497 ), #17250, .T. ) ;
#2569 = DIRECTION ( 'NONE',  ( -1.000000000000000000, -0.000000000000000000, -0.000000000000000000 ) ) ;
#2570 = EDGE_CURVE ( 'NONE', #29511, #40610, #48160, .T. ) ;
#2571 = CARTESIAN_POINT ( 'NONE',  ( -3.000000000000000000, 20.85821328998741109, 10.92862929874522315 ) ) ;
#2572 = CARTESIAN_POINT ( 'NONE',  ( 5.999999999999999112, -63.97538442413463855, 51.29473840253199057 ) ) ;
#2573 = ORIENTED_EDGE ( 'NONE', *, *, #4080, .F. ) ;
#2574 = DIRECTION ( 'NONE',  ( 0.000000000000000000, 0.000000000000000000, 1.000000000000000000 ) ) ;
#2575 = EDGE_CURVE ( 'NONE', #39350, #13463, #33307, .T. ) ;
#2576 = ADVANCED_FACE ( 'NONE', ( #13593 ), #47829, .T. ) ;
#2577 = CARTESIAN_POINT ( 'NONE',  ( 11.99999999999999822, 0.000000000000000000, 0.000000000000000000 ) ) ;
#2578 = ORIENTED_EDGE ( 'NONE', *, *, #27544, .F. ) ;
#2579 = ORIENTED_EDGE ( 'NONE', *, *, #14247, .F. ) ;
#2580 = AXIS2_PLACEMENT_3D ( 'NONE', #18650, #14996, #11331 ) ;
#2581 = AXIS2_PLACEMENT_3D ( 'NONE', #14854, #3833, #29770 ) ;
#2582 = CIRCLE ( 'NONE', #41696, 12.49999999999999645 ) ;
#2583 = AXIS2_PLACEMENT_3D ( 'NONE', #17786, #32717, #40551 ) ;
#2584 = LINE ( 'NONE', #13378, #41429 ) ;
#2585 = VERTEX_POINT ( 'NONE', #36819 ) ;
#2586 = ADVANCED_FACE ( 'NONE', ( #14317 ), #33161, .F. ) ;
#2587 = ADVANCED_FACE ( 'NONE', ( #32447 ), #25318, .T. ) ;
#2588 = VECTOR ( 'NONE', #17187, 1000.000000000000000 ) ;
#2589 = DIRECTION ( 'NONE',  ( -1.000000000000000000, 0.000000000000000000, 0.000000000000000000 ) ) ;
#2590 = AXIS2_PLACEMENT_3D ( 'NONE', #34307, #26996, #27229 ) ;
#2591 = LINE ( 'NONE', #32234, #17552 ) ;
#2592 = VERTEX_POINT ( 'NONE', #14572 ) ;
#2593 = ORIENTED_EDGE ( 'NONE', *, *, #20633, .F. ) ;
#2594 = FACE_OUTER_BOUND ( 'NONE', #19789, .T. ) ;
#2595 = ADVANCED_FACE ( 'NONE', ( #17747 ), #36348, .F. ) ;
#2596 = CARTESIAN_POINT ( 'NONE',  ( 10.00000000000000000, 65.64334221924966073, -41.19522573413664190 ) ) ;
#2597 = DIRECTION ( 'NONE',  ( 0.000000000000000000, -0.9510565162951543083, -0.3090169943749448977 ) ) ;
#2598 = ORIENTED_EDGE ( 'NONE', *, *, #19428, .F. ) ;
#2599 = ORIENTED_EDGE ( 'NONE', *, *, #12044, .F. ) ;
#2600 = CARTESIAN_POINT ( 'NONE',  ( 12.00000000000000000, 24.81905959214275370, 9.408202855044498492 ) ) ;
#2601 = ORIENTED_EDGE ( 'NONE', *, *, #2409, .T. ) ;
#2602 = DIRECTION ( 'NONE',  ( 0.000000000000000000, 0.000000000000000000, 1.000000000000000000 ) ) ;
#2603 = PLANE ( 'NONE',  #12776 ) ;
#2604 = DIRECTION ( 'NONE',  ( 0.000000000000000000, 0.000000000000000000, -1.000000000000000000 ) ) ;
#2605 = DIRECTION ( 'NONE',  ( -1.000000000000000000, 0.000000000000000000, 0.000000000000000000 ) ) ;
#2606 = VECTOR ( 'NONE', #3164, 1000.000000000000000 ) ;
#2607 = DIRECTION ( 'NONE',  ( 0.000000000000000000, 0.1564344650402242354, 0.9876883405951387696 ) ) ;
#2608 = LINE ( 'NONE', #27884, #25894 ) ;
#2609 = VERTEX_POINT ( 'NONE', #43469 ) ;
#2610 = CARTESIAN_POINT ( 'NONE',  ( 0.000000000000000000, 0.000000000000000000, 0.000000000000000000 ) ) ;
#2611 = VERTEX_POINT ( 'NONE', #28995 ) ;
#2612 = VECTOR ( 'NONE', #19901, 1000.000000000000000 ) ;
#2613 = CIRCLE ( 'NONE', #29989, 82.00000000000000000 ) ;
#2614 = CARTESIAN_POINT ( 'NONE',  ( 0.000000000000000000, 63.97538442413426907, 51.29473840253246664 ) ) ;
#2615 = CYLINDRICAL_SURFACE ( 'NONE', #15241, 31.99999999999998579 ) ;
#2616 = VERTEX_POINT ( 'NONE', #13850 ) ;
#2617 = CARTESIAN_POINT ( 'NONE',  ( -1.066668064568189757E-15, -1.540743955509788682E-30, -10.00000000000000178 ) ) ;
#2618 = CARTESIAN_POINT ( 'NONE',  ( 0.000000000000000000, 2.956366410621684260, -75.11725578898465017 ) ) ;
#2619 = DIRECTION ( 'NONE',  ( 0.000000000000000000, 0.000000000000000000, 1.000000000000000000 ) ) ;
#2620 = ADVANCED_FACE ( 'NONE', ( #28769 ), #6972, .T. ) ;
#2621 = AXIS2_PLACEMENT_3D ( 'NONE', #10793, #14709, #7109 ) ;
#2622 = AXIS2_PLACEMENT_3D ( 'NONE', #18703, #29726, #25804 ) ;
#2623 = DIRECTION ( 'NONE',  ( -1.000000000000000000, -0.000000000000000000, -0.000000000000000000 ) ) ;
#2624 = CARTESIAN_POINT ( 'NONE',  ( 21.07894319797337701, -103.8699611390234878, -5.500000000000000000 ) ) ;
#2625 = CYLINDRICAL_SURFACE ( 'NONE', #48107, 77.49899999999999523 ) ;
#2626 = EDGE_LOOP ( 'NONE', ( #1408, #20178, #23614, #17644 ) ) ;
#2627 = VECTOR ( 'NONE', #22286, 1000.000000000000000 ) ;
#2628 = EDGE_CURVE ( 'NONE', #3559, #40015, #37292, .T. ) ;
#2629 = DIRECTION ( 'NONE',  ( -1.000000000000000000, -0.000000000000000000, -0.000000000000000000 ) ) ;
#2630 =( LENGTH_UNIT ( ) NAMED_UNIT ( * ) SI_UNIT ( .MILLI., .METRE. ) );
#2631 = EDGE_CURVE ( 'NONE', #17516, #10088, #21678, .T. ) ;
#2632 = VECTOR ( 'NONE', #12078, 1000.000000000000114 ) ;
#2633 = EDGE_LOOP ( 'NONE', ( #10303, #21374, #31222, #38580 ) ) ;
#2634 = VERTEX_POINT ( 'NONE', #47122 ) ;
#2635 = ORIENTED_EDGE ( 'NONE', *, *, #20793, .T. ) ;
#2636 = EDGE_CURVE ( 'NONE', #38237, #4028, #32905, .T. ) ;
#2637 = CARTESIAN_POINT ( 'NONE',  ( 10.00000000000000000, -30.80686688397025108, 21.53537804866070715 ) ) ;
#2638 = CARTESIAN_POINT ( 'NONE',  ( 10.00000000000000000, 0.000000000000000000, 0.000000000000000000 ) ) ;
#2639 = ORIENTED_EDGE ( 'NONE', *, *, #39527, .F. ) ;
#2640 = EDGE_CURVE ( 'NONE', #2161, #12123, #11488, .T. ) ;
#2641 = EDGE_CURVE ( 'NONE', #5936, #21061, #40510, .T. ) ;
#2642 = VECTOR ( 'NONE', #33467, 1000.000000000000000 ) ;
#2643 = ORIENTED_EDGE ( 'NONE', *, *, #30412, .T. ) ;
#2644 = VECTOR ( 'NONE', #21822, 1000.000000000000000 ) ;
#2645 = DIRECTION ( 'NONE',  ( -1.000000000000000000, 0.000000000000000000, -0.000000000000000000 ) ) ;
#2646 = AXIS2_PLACEMENT_3D ( 'NONE', #23223, #37185, #38156 ) ;
#2647 = VECTOR ( 'NONE', #8690, 1000.000000000000000 ) ;
#2648 = AXIS2_PLACEMENT_3D ( 'NONE', #16804, #29731, #3056 ) ;
#2649 = EDGE_LOOP ( 'NONE', ( #42446, #25067, #30589, #41280 ) ) ;
#2650 = ORIENTED_EDGE ( 'NONE', *, *, #23966, .F. ) ;
#2651 = ORIENTED_EDGE ( 'NONE', *, *, #6841, .F. ) ;
#2652 = PRODUCT ( 'key', 'key', '', ( #29200 ) ) ;
#2653 = EDGE_CURVE ( 'NONE', #14712, #46727, #6043, .T. ) ;
#2654 = CARTESIAN_POINT ( 'NONE',  ( 10.00000000000000000, 38.55633173627010990, 16.65560815589424593 ) ) ;
#2655 = AXIS2_PLACEMENT_3D ( 'NONE', #21959, #10953, #11198 ) ;
#2656 = ORIENTED_EDGE ( 'NONE', *, *, #42878, .T. ) ;
#2657 = FACE_OUTER_BOUND ( 'NONE', #430, .T. ) ;
#2658 = ORIENTED_EDGE ( 'NONE', *, *, #10495, .T. ) ;
#2659 = CIRCLE ( 'NONE', #46472, 77.49899999999999523 ) ;
#2660 = CARTESIAN_POINT ( 'NONE',  ( 12.00000000000000000, 14.60985201121729737, 18.46759930825687235 ) ) ;
#2661 = VECTOR ( 'NONE', #11469, 1000.000000000000000 ) ;
#2662 = CARTESIAN_POINT ( 'NONE',  ( 0.000000000000000000, -35.38097989696520074, 12.42422080174625520 ) ) ;
#2663 = LINE ( 'NONE', #3382, #4109 ) ;
#2665 = ORIENTED_EDGE ( 'NONE', *, *, #27099, .F. ) ;
#2664 = CIRCLE ( 'NONE', #11287, 31.99999999999998579 ) ;
#2666 = DIRECTION ( 'NONE',  ( -1.000000000000000000, 0.000000000000000000, -0.000000000000000000 ) ) ;
#2667 = ORIENTED_EDGE ( 'NONE', *, *, #42164, .T. ) ;
#2668 = CARTESIAN_POINT ( 'NONE',  ( 10.00000000000000000, 40.65526001592612459, 71.21200624218811015 ) ) ;
#2669 = DIRECTION ( 'NONE',  ( -1.000000000000000000, -0.000000000000000000, 0.000000000000000000 ) ) ;
#2670 = VERTEX_POINT ( 'NONE', #21663 ) ;
#2671 = EDGE_LOOP ( 'NONE', ( #29337, #5818, #6491, #27847 ) ) ;
#2672 = LINE ( 'NONE', #10264, #36156 ) ;
#2673 = FACE_OUTER_BOUND ( 'NONE', #4889, .T. ) ;
#2674 = ORIENTED_EDGE ( 'NONE', *, *, #16344, .T. ) ;
#2675 = EDGE_LOOP ( 'NONE', ( #36426, #6545, #28197, #36081 ) ) ;
#2676 = DIRECTION ( 'NONE',  ( -1.000000000000000000, -0.000000000000000000, 0.000000000000000000 ) ) ;
#2677 = DIRECTION ( 'NONE',  ( 0.000000000000000000, 0.000000000000000000, 1.000000000000000000 ) ) ;
#2678 = DIRECTION ( 'NONE',  ( -1.000000000000000000, -0.000000000000000000, -0.000000000000000000 ) ) ;
#2679 = VECTOR ( 'NONE', #20035, 1000.000000000000000 ) ;
#2680 = FACE_OUTER_BOUND ( 'NONE', #8736, .T. ) ;
#2681 = CARTESIAN_POINT ( 'NONE',  ( -10.00000000000000000, 0.000000000000000000, 0.000000000000000000 ) ) ;
#2682 = ORIENTED_EDGE ( 'NONE', *, *, #17701, .T. ) ;
#2683 = CIRCLE ( 'NONE', #38671, 31.99999999999999289 ) ;
#2684 = FACE_OUTER_BOUND ( 'NONE', #23919, .T. ) ;
#2685 = CYLINDRICAL_SURFACE ( 'NONE', #30910, 82.00000000000000000 ) ;
#2686 = CIRCLE ( 'NONE', #17542, 82.00000000000000000 ) ;
#2687 = AXIS2_PLACEMENT_3D ( 'NONE', #20900, #35823, #31443 ) ;
#2688 = EDGE_CURVE ( 'NONE', #11204, #39764, #31063, .T. ) ;
#2689 = CARTESIAN_POINT ( 'NONE',  ( 11.99999999999999822, 35.91791733033476675, 68.67312586195008350 ) ) ;
#2690 = DIRECTION ( 'NONE',  ( 0.000000000000000000, 0.4539904997395413644, 0.8910065241883706744 ) ) ;
#2691 = DIRECTION ( 'NONE',  ( -1.000000000000000000, 0.000000000000000000, 0.000000000000000000 ) ) ;
#2692 = ADVANCED_FACE ( 'NONE', ( #18931 ), #41241, .T. ) ;
#2693 = CARTESIAN_POINT ( 'NONE',  ( 0.000000000000000000, 0.000000000000000000, 0.000000000000000000 ) ) ;
#2694 = EDGE_CURVE ( 'NONE', #14256, #13625, #27143, .T. ) ;
#2695 = ORIENTED_EDGE ( 'NONE', *, *, #36836, .F. ) ;
#2696 = ORIENTED_EDGE ( 'NONE', *, *, #38867, .T. ) ;
#2697 = ORIENTED_EDGE ( 'NONE', *, *, #37434, .F. ) ;
#2698 = ADVANCED_FACE ( 'NONE', ( #29722 ), #37553, .F. ) ;
#2699 = VECTOR ( 'NONE', #12916, 1000.000000000000000 ) ;
#2700 = AXIS2_PLACEMENT_3D ( 'NONE', #32093, #39688, #43351 ) ;
#2701 = EDGE_CURVE ( 'NONE', #14023, #37807, #3779, .T. ) ;
#2702 = VECTOR ( 'NONE', #44475, 1000.000000000000000 ) ;
#2703 = DIRECTION ( 'NONE',  ( 0.000000000000000000, -0.9135454576426059736, 0.4067366430757887730 ) ) ;
#2704 = AXIS2_PLACEMENT_3D ( 'NONE', #14531, #26271, #25277 ) ;
#2705 = ITEM_DEFINED_TRANSFORMATION ( 'NONE', 'NONE', #30372,  #11636 ) ;
#2706 = VECTOR ( 'NONE', #3711, 1000.000000000000227 ) ;
#2707 = DIRECTION ( 'NONE',  ( -1.000000000000000000, 0.000000000000000000, -0.000000000000000000 ) ) ;
#2708 = ORIENTED_EDGE ( 'NONE', *, *, #30296, .T. ) ;
#2709 = EDGE_CURVE ( 'NONE', #31959, #4498, #3538, .T. ) ;
#2710 = ADVANCED_FACE ( 'NONE', ( #15045 ), #26777, .T. ) ;
#2711 = LINE ( 'NONE', #14217, #21010 ) ;
#2712 = DIRECTION ( 'NONE',  ( 1.000000000000000000, 0.000000000000000000, -0.000000000000000000 ) ) ;
#2713 = VERTEX_POINT ( 'NONE', #7693 ) ;
#2714 = CARTESIAN_POINT ( 'NONE',  ( 0.000000000000000000, 0.000000000000000000, 0.000000000000000000 ) ) ;
#2715 = ORIENTED_EDGE ( 'NONE', *, *, #36049, .F. ) ;
#2716 = ADVANCED_FACE ( 'NONE', ( #44656 ), #29967, .F. ) ;
#2717 = AXIS2_PLACEMENT_3D ( 'NONE', #18469, #44899, #7692 ) ;
#2718 = ORIENTED_EDGE ( 'NONE', *, *, #36616, .T. ) ;
#2719 = DIRECTION ( 'NONE',  ( 1.000000000000000000, 0.000000000000000000, 0.000000000000000000 ) ) ;
#2720 = LINE ( 'NONE', #17652, #30522 ) ;
#2721 = ORIENTED_EDGE ( 'NONE', *, *, #10550, .T. ) ;
#2722 = AXIS2_PLACEMENT_3D ( 'NONE', #19407, #38267, #4502 ) ;
#2723 = CARTESIAN_POINT ( 'NONE',  ( 10.00000000000000000, 8.840884882376133902, -74.65374052328640175 ) ) ;
#2724 = ORIENTED_EDGE ( 'NONE', *, *, #22985, .F. ) ;
#2725 = CYLINDRICAL_SURFACE ( 'NONE', #26202, 16.00000000000000000 ) ;
#2726 = ORIENTED_EDGE ( 'NONE', *, *, #10122, .T. ) ;
#2727 = CARTESIAN_POINT ( 'NONE',  ( -12.49999999999999822, -120.0000000000000000, 125.0000000000000000 ) ) ;
#2728 = CARTESIAN_POINT ( 'NONE',  ( 11.99999999999999822, -58.39081064771713869, -50.95692526931392052 ) ) ;
#2729 = DIRECTION ( 'NONE',  ( 0.000000000000000000, 0.4539904997395479702, -0.8910065241883673437 ) ) ;
#2730 = ADVANCED_FACE ( 'NONE', ( #22392 ), #46678, .T. ) ;
#2732 = ORIENTED_EDGE ( 'NONE', *, *, #43881, .T. ) ;
#2731 = CARTESIAN_POINT ( 'NONE',  ( 0.000000000000000000, 0.000000000000000000, 0.000000000000000000 ) ) ;
#2733 = CARTESIAN_POINT ( 'NONE',  ( 10.00000000000000000, -17.28742895386031719, -75.54627589209962935 ) ) ;
#2734 = AXIS2_PLACEMENT_3D ( 'NONE', #20414, #24105, #43441 ) ;
#2735 = CIRCLE ( 'NONE', #30113, 31.99999999999998579 ) ;
#2736 = ORIENTED_EDGE ( 'NONE', *, *, #561, .T. ) ;
#2737 = DIRECTION ( 'NONE',  ( -1.000000000000000000, 0.000000000000000000, 0.000000000000000000 ) ) ;
#2738 = VERTEX_POINT ( 'NONE', #14804 ) ;
#2739 = ORIENTED_EDGE ( 'NONE', *, *, #29724, .T. ) ;
#2740 = DIRECTION ( 'NONE',  ( -1.000000000000000000, 0.000000000000000000, 0.000000000000000000 ) ) ;
#2741 = DIRECTION ( 'NONE',  ( -0.000000000000000000, -2.312964634635746211E-15, 1.000000000000000000 ) ) ;
#2742 = DIRECTION ( 'NONE',  ( -1.000000000000000000, -0.000000000000000000, 0.000000000000000000 ) ) ;
#2743 = VECTOR ( 'NONE', #20313, 1000.000000000000000 ) ;
#2744 = DIRECTION ( 'NONE',  ( 1.000000000000000000, 0.000000000000000000, 0.000000000000000000 ) ) ;
#2745 = DIRECTION ( 'NONE',  ( 0.000000000000000000, -0.7604059656000228262, -0.6494480483301932061 ) ) ;
#2746 = ORIENTED_EDGE ( 'NONE', *, *, #35828, .F. ) ;
#2747 = CARTESIAN_POINT ( 'NONE',  ( 0.000000000000000000, 0.000000000000000000, 0.000000000000000000 ) ) ;
#2748 = AXIS2_PLACEMENT_3D ( 'NONE', #24349, #21399, #39284 ) ;
#2749 = DIRECTION ( 'NONE',  ( 0.000000000000000000, 0.000000000000000000, 1.000000000000000000 ) ) ;
#2750 = AXIS2_PLACEMENT_3D ( 'NONE', #22542, #30379, #34756 ) ;
#2751 = DIRECTION ( 'NONE',  ( -1.000000000000000000, 0.000000000000000000, -0.000000000000000000 ) ) ;
#2752 = CARTESIAN_POINT ( 'NONE',  ( 15.00000000000000000, -13.04903810567646971, 19.60159698893442481 ) ) ;
#2753 = CIRCLE ( 'NONE', #23904, 15.99999999999999822 ) ;
#2754 = CARTESIAN_POINT ( 'NONE',  ( 10.00000000000000000, -37.58145647212455032, 16.68533520207890319 ) ) ;
#2755 = DIRECTION ( 'NONE',  ( 0.000000000000000000, -0.5877852522924802425, 0.8090169943749422332 ) ) ;
#2756 = FACE_OUTER_BOUND ( 'NONE', #8111, .T. ) ;
#2757 = CARTESIAN_POINT ( 'NONE',  ( 11.99999999999999822, 51.03279382321166224, -55.19960302592011914 ) ) ;
#2758 = EDGE_CURVE ( 'NONE', #14154, #4001, #11130, .T. ) ;
#2759 = EDGE_CURVE ( 'NONE', #26945, #5219, #37794, .T. ) ;
#2760 = VERTEX_POINT ( 'NONE', #44900 ) ;
#2761 = CIRCLE ( 'NONE', #36372, 32.00000000000000711 ) ;
#2762 = DIRECTION ( 'NONE',  ( 0.000000000000000000, 0.07845909572783797692, 0.9969173337331285190 ) ) ;
#2763 = CARTESIAN_POINT ( 'NONE',  ( 11.99999999999999822, 0.000000000000000000, 0.000000000000000000 ) ) ;
#2764 = EDGE_CURVE ( 'NONE', #19937, #13075, #48223, .T. ) ;
#2765 = ORIENTED_EDGE ( 'NONE', *, *, #7174, .F. ) ;
#2766 = AXIS2_PLACEMENT_3D ( 'NONE', #19416, #8645, #344 ) ;
#2767 = CARTESIAN_POINT ( 'NONE',  ( 0.000000000000000000, 12.26510123303308752, -35.53030884539072787 ) ) ;
#2768 = VERTEX_POINT ( 'NONE', #18700 ) ;
#2769 = EDGE_CURVE ( 'NONE', #28305, #27618, #28672, .T. ) ;
#2770 = FACE_OUTER_BOUND ( 'NONE', #42471, .T. ) ;
#2771 = CARTESIAN_POINT ( 'NONE',  ( -3.000000000000000000, 9.615535125378775305, 24.73947219025917121 ) ) ;
#2772 = EDGE_LOOP ( 'NONE', ( #27994, #34696 ) ) ;
#2773 = CIRCLE ( 'NONE', #12965, 37.49900000000000944 ) ;
#2774 = AXIS2_PLACEMENT_3D ( 'NONE', #43907, #28745, #36792 ) ;
#2775 = DIRECTION ( 'NONE',  ( -1.000000000000000000, 0.000000000000000000, 0.000000000000000000 ) ) ;
#2776 = CIRCLE ( 'NONE', #30158, 13.90444123027096879 ) ;
#2777 = ORIENTED_EDGE ( 'NONE', *, *, #7716, .F. ) ;
#2778 = VECTOR ( 'NONE', #46587, 1000.000000000000000 ) ;
#2779 = AXIS2_PLACEMENT_3D ( 'NONE', #32071, #13221, #27668 ) ;
#2780 = CARTESIAN_POINT ( 'NONE',  ( -70.53423027509626309, -217.0820393249940423, 5.500000000000000000 ) ) ;
#2781 = DIRECTION ( 'NONE',  ( 1.000000000000000000, 0.000000000000000000, 0.000000000000000000 ) ) ;
#2782 = SHAPE_REPRESENTATION ( 'Input Shaft', ( #11636 ), #3848 ) ;
#2783 = DIRECTION ( 'NONE',  ( 0.000000000000000000, 0.000000000000000000, 1.000000000000000000 ) ) ;
#2784 = ORIENTED_EDGE ( 'NONE', *, *, #42154, .F. ) ;
#2785 = DIRECTION ( 'NONE',  ( 0.000000000000000000, 0.000000000000000000, 1.000000000000000000 ) ) ;
#2786 = CIRCLE ( 'NONE', #39536, 42.00000000000000000 ) ;
#2787 = CIRCLE ( 'NONE', #9054, 31.99999999999999289 ) ;
#2788 = ORIENTED_EDGE ( 'NONE', *, *, #1819, .T. ) ;
#2789 = DIRECTION ( 'NONE',  ( 0.5687579148473743684, -0.8225049752423791993, 0.000000000000000000 ) ) ;
#2790 = CARTESIAN_POINT ( 'NONE',  ( 10.00000000000000000, 0.000000000000000000, 0.000000000000000000 ) ) ;
#2791 = LINE ( 'NONE', #47102, #30618 ) ;
#2792 = VECTOR ( 'NONE', #8362, 1000.000000000000000 ) ;
#2793 = VERTEX_POINT ( 'NONE', #33631 ) ;
#2794 = DIRECTION ( 'NONE',  ( 1.000000000000000000, 0.000000000000000000, 0.000000000000000000 ) ) ;
#2795 = VERTEX_POINT ( 'NONE', #12111 ) ;
#2796 = ORIENTED_EDGE ( 'NONE', *, *, #25243, .T. ) ;
#2797 = CARTESIAN_POINT ( 'NONE',  ( 11.99999999999999822, 0.000000000000000000, 0.000000000000000000 ) ) ;
#2798 = CARTESIAN_POINT ( 'NONE',  ( 0.000000000000000000, 3.925862922256769583, -41.81611651403857621 ) ) ;
#2799 = CARTESIAN_POINT ( 'NONE',  ( 11.99999999999999822, -41.19522573413689059, -65.64334221924951862 ) ) ;
#2800 = DIRECTION ( 'NONE',  ( 1.000000000000000000, 0.000000000000000000, 0.000000000000000000 ) ) ;
#2801 = ORIENTED_EDGE ( 'NONE', *, *, #34348, .T. ) ;
#2802 = DIRECTION ( 'NONE',  ( -1.000000000000000000, -0.000000000000000000, -0.000000000000000000 ) ) ;
#2803 = CIRCLE ( 'NONE', #40352, 32.00000000000000000 ) ;
#2804 = FACE_OUTER_BOUND ( 'NONE', #1197, .T. ) ;
#2805 = DIRECTION ( 'NONE',  ( 0.000000000000000000, 0.000000000000000000, -1.000000000000000000 ) ) ;
#2806 = DIRECTION ( 'NONE',  ( -0.000000000000000000, -0.000000000000000000, -1.000000000000000000 ) ) ;
#2807 = CARTESIAN_POINT ( 'NONE',  ( -3.000000000000002665, 0.000000000000000000, 0.000000000000000000 ) ) ;
#2808 = EDGE_CURVE ( 'NONE', #4369, #29100, #594, .T. ) ;
#2809 = LINE ( 'NONE', #28992, #28577 ) ;
#2810 = AXIS2_PLACEMENT_3D ( 'NONE', #35956, #6352, #39660 ) ;
#2811 = ORIENTED_EDGE ( 'NONE', *, *, #376, .T. ) ;
#2812 = DIRECTION ( 'NONE',  ( -1.000000000000000000, 0.000000000000000000, 0.000000000000000000 ) ) ;
#2813 = EDGE_CURVE ( 'NONE', #27530, #30209, #96, .T. ) ;
#2814 = CIRCLE ( 'NONE', #19999, 16.00000000000000355 ) ;
#2815 = DIRECTION ( 'NONE',  ( 0.000000000000000000, 0.000000000000000000, 1.000000000000000000 ) ) ;
#2816 = DIRECTION ( 'NONE',  ( 1.000000000000000000, -0.000000000000000000, -0.000000000000000000 ) ) ;
#2817 = EDGE_CURVE ( 'NONE', #8980, #19503, #8737, .T. ) ;
#2818 = CIRCLE ( 'NONE', #6630, 31.99999999999999289 ) ;
#2819 = DIRECTION ( 'NONE',  ( -1.000000000000000000, 0.000000000000000000, 0.000000000000000000 ) ) ;
#2820 = LINE ( 'NONE', #6033, #2143 ) ;
#2821 = CARTESIAN_POINT ( 'NONE',  ( 10.00000000000000000, 12.42422080174688404, -35.38097989696498047 ) ) ;
#2822 = AXIS2_PLACEMENT_3D ( 'NONE', #19203, #30233, #33413 ) ;
#2823 = VERTEX_POINT ( 'NONE', #41968 ) ;
#2824 = ADVANCED_FACE ( 'NONE', ( #8419 ), #23345, .F. ) ;
#2825 = DIRECTION ( 'NONE',  ( 0.000000000000000000, 0.000000000000000000, 1.000000000000000000 ) ) ;
#2826 = AXIS2_PLACEMENT_3D ( 'NONE', #6439, #14512, #29438 ) ;
#2827 = EDGE_CURVE ( 'NONE', #1961, #41810, #27273, .T. ) ;
#2828 = VECTOR ( 'NONE', #10809, 1000.000000000000114 ) ;
#2829 = DIRECTION ( 'NONE',  ( 1.000000000000000000, 0.000000000000000000, 0.000000000000000000 ) ) ;
#2830 = VERTEX_POINT ( 'NONE', #1066 ) ;
#2831 = ORIENTED_EDGE ( 'NONE', *, *, #14332, .F. ) ;
#2832 = AXIS2_PLACEMENT_3D ( 'NONE', #19530, #11257, #26182 ) ;
#2833 = ORIENTED_EDGE ( 'NONE', *, *, #35142, .T. ) ;
#2834 = ADVANCED_FACE ( 'NONE', ( #27764 ), #5244, .F. ) ;
#2835 = CARTESIAN_POINT ( 'NONE',  ( 0.000000000000000000, -75.11764819372149304, 2.946379043146075905 ) ) ;
#2836 = ORIENTED_EDGE ( 'NONE', *, *, #30067, .F. ) ;
#2837 = VERTEX_POINT ( 'NONE', #1565 ) ;
#2838 = AXIS2_PLACEMENT_3D ( 'NONE', #24658, #12927, #27865 ) ;
#2839 = LINE ( 'NONE', #37339, #27728 ) ;
#2840 = DIRECTION ( 'NONE',  ( 0.000000000000000000, 0.8090169943749447867, 0.5877852522924769119 ) ) ;
#2841 = CARTESIAN_POINT ( 'NONE',  ( 15.00000000000000000, 22.07842321921492612, 8.187992925817123790 ) ) ;
#2842 = ORIENTED_EDGE ( 'NONE', *, *, #20845, .T. ) ;
#2843 = AXIS2_PLACEMENT_3D ( 'NONE', #759, #37983, #23289 ) ;
#2844 = LINE ( 'NONE', #43728, #39877 ) ;
#2845 = VERTEX_POINT ( 'NONE', #23838 ) ;
#2846 = ORIENTED_EDGE ( 'NONE', *, *, #13321, .F. ) ;
#2847 = ORIENTED_EDGE ( 'NONE', *, *, #34455, .T. ) ;
#2848 = CARTESIAN_POINT ( 'NONE',  ( 10.00000000000000000, -40.98264845739755913, 9.188173127307164734 ) ) ;
#2849 = DIRECTION ( 'NONE',  ( 1.000000000000000000, 0.000000000000000000, 0.000000000000000000 ) ) ;
#2850 = LINE ( 'NONE', #18010, #40754 ) ;
#2851 = ADVANCED_FACE ( 'NONE', ( #1325 ), #13070, .T. ) ;
#2852 = EDGE_LOOP ( 'NONE', ( #39309, #23407, #28239, #34567 ) ) ;
#2853 = AXIS2_PLACEMENT_3D ( 'NONE', #19303, #34713, #5118 ) ;
#2854 = EDGE_LOOP ( 'NONE', ( #45653, #17468, #34764, #23893 ) ) ;
#2855 = CARTESIAN_POINT ( 'NONE',  ( 10.00000000000000000, 35.91791733033570466, -68.67312586194960033 ) ) ;
#2856 = ORIENTED_EDGE ( 'NONE', *, *, #3753, .F. ) ;
#2857 = DIRECTION ( 'NONE',  ( 0.000000000000000000, -0.5224985647159380298, -0.8526401643540988395 ) ) ;
#2858 = EDGE_CURVE ( 'NONE', #37895, #45965, #23595, .T. ) ;
#2859 = CYLINDRICAL_SURFACE ( 'NONE', #6123, 16.00000000000000000 ) ;
#2860 = DIRECTION ( 'NONE',  ( 1.000000000000000000, 0.000000000000000000, -0.000000000000000000 ) ) ;
#2861 = VERTEX_POINT ( 'NONE', #16260 ) ;
#2862 = FACE_OUTER_BOUND ( 'NONE', #40045, .T. ) ;
#2863 = PLANE ( 'NONE',  #8071 ) ;
#2864 = AXIS2_PLACEMENT_3D ( 'NONE', #3347, #33226, #48152 ) ;
#2865 = ADVANCED_FACE ( 'NONE', ( #16013 ), #19655, .T. ) ;
#2866 = DIRECTION ( 'NONE',  ( 0.000000000000000000, -0.4067366430757887730, -0.9135454576426059736 ) ) ;
#2867 = AXIS2_PLACEMENT_3D ( 'NONE', #5065, #19980, #20708 ) ;
#2868 = FACE_OUTER_BOUND ( 'NONE', #43775, .T. ) ;
#2869 = ORIENTED_EDGE ( 'NONE', *, *, #14040, .F. ) ;
#2870 = CYLINDRICAL_SURFACE ( 'NONE', #37400, 31.99999999999998579 ) ;
#2871 = DIRECTION ( 'NONE',  ( -1.000000000000000000, -0.000000000000000000, 0.000000000000000000 ) ) ;
#2872 = CARTESIAN_POINT ( 'NONE',  ( 10.00000000000000000, 0.000000000000000000, 0.000000000000000000 ) ) ;
#2873 = LINE ( 'NONE', #24680, #8806 ) ;
#2874 = EDGE_CURVE ( 'NONE', #35343, #1265, #18099, .T. ) ;
#2875 = EDGE_CURVE ( 'NONE', #2760, #26919, #28001, .T. ) ;
#2876 = EDGE_LOOP ( 'NONE', ( #10804, #35963, #16596, #630 ) ) ;
#2877 = EDGE_CURVE ( 'NONE', #9073, #20085, #12580, .T. ) ;
#2878 = AXIS2_PLACEMENT_3D ( 'NONE', #44419, #6736, #25800 ) ;
#2879 = LINE ( 'NONE', #32510, #33367 ) ;
#2880 = DIRECTION ( 'NONE',  ( 0.9918136447140100120, -0.1276937514489704939, 0.000000000000000000 ) ) ;
#2881 = VECTOR ( 'NONE', #36860, 1000.000000000000000 ) ;
#2882 = LINE ( 'NONE', #17807, #32572 ) ;
#2883 = CARTESIAN_POINT ( 'NONE',  ( 0.000000000000000000, -80.55351364060578589, -15.33399622253568673 ) ) ;
#2884 = CARTESIAN_POINT ( 'NONE',  ( -24.50849501662245800, -109.8101191361138831, 5.500000000000000000 ) ) ;
#2885 = AXIS2_PLACEMENT_3D ( 'NONE', #23459, #1449, #38402 ) ;
#2886 = DIRECTION ( 'NONE',  ( 0.000000000000000000, 0.5877852522924684742, 0.8090169943749506709 ) ) ;
#2887 = ORIENTED_EDGE ( 'NONE', *, *, #8363, .F. ) ;
#2888 = ORIENTED_EDGE ( 'NONE', *, *, #35460, .T. ) ;
#2889 = VERTEX_POINT ( 'NONE', #8897 ) ;
#2890 = AXIS2_PLACEMENT_3D ( 'NONE', #21353, #22072, #32391 ) ;
#2891 = CARTESIAN_POINT ( 'NONE',  ( 5.999999999999999112, -67.80270845531855173, -46.11716303203260736 ) ) ;
#2892 = AXIS2_PLACEMENT_3D ( 'NONE', #43474, #46666, #28058 ) ;
#2893 = CARTESIAN_POINT ( 'NONE',  ( -0.2999999999999947153, 1.530808498934191521E-15, 12.50000000000000000 ) ) ;
#2894 = ORIENTED_EDGE ( 'NONE', *, *, #22285, .F. ) ;
#2895 = VECTOR ( 'NONE', #11394, 1000.000000000000000 ) ;
#2896 = CARTESIAN_POINT ( 'NONE',  ( 5.999999999999999112, 55.16347631943042984, 60.67117009219155932 ) ) ;
#2897 = ORIENTED_EDGE ( 'NONE', *, *, #43439, .T. ) ;
#2898 = EDGE_LOOP ( 'NONE', ( #26263, #38088, #25427, #15314 ) ) ;
#2899 = ORIENTED_EDGE ( 'NONE', *, *, #33085, .T. ) ;
#2900 = AXIS2_PLACEMENT_3D ( 'NONE', #17973, #43693, #32208 ) ;
#2901 = VECTOR ( 'NONE', #25301, 1000.000000000000000 ) ;
#2902 = DIRECTION ( 'NONE',  ( 1.000000000000000000, 0.000000000000000000, 0.000000000000000000 ) ) ;
#2903 = EDGE_CURVE ( 'NONE', #35831, #42467, #7939, .T. ) ;
#2904 = ORIENTED_EDGE ( 'NONE', *, *, #42276, .F. ) ;
#2905 = EDGE_LOOP ( 'NONE', ( #41176, #10231, #43765, #2842, #45733, #45707, #47300, #38447 ) ) ;
#2906 = CARTESIAN_POINT ( 'NONE',  ( -10.00000000000000000, 0.000000000000000000, 0.000000000000000000 ) ) ;
#2907 = EDGE_LOOP ( 'NONE', ( #43189, #29272, #16232, #46805 ) ) ;
#2908 = DIRECTION ( 'NONE',  ( 0.000000000000000000, 0.000000000000000000, 1.000000000000000000 ) ) ;
#2909 = EDGE_CURVE ( 'NONE', #15376, #46446, #40794, .T. ) ;
#2910 = CIRCLE ( 'NONE', #37334, 42.00000000000000000 ) ;
#2911 = CARTESIAN_POINT ( 'NONE',  ( 0.000000000000000000, 0.000000000000000000, 0.000000000000000000 ) ) ;
#2912 = CARTESIAN_POINT ( 'NONE',  ( 10.00000000000000000, 17.80606268964540462, 33.00180498840053644 ) ) ;
#2913 = EDGE_CURVE ( 'NONE', #19886, #28052, #34586, .T. ) ;
#2914 = ORIENTED_EDGE ( 'NONE', *, *, #21131, .F. ) ;
#2915 = DIRECTION ( 'NONE',  ( -1.000000000000000000, -0.000000000000000000, -0.000000000000000000 ) ) ;
#2916 = ORIENTED_EDGE ( 'NONE', *, *, #38071, .T. ) ;
#2917 = DIRECTION ( 'NONE',  ( 1.000000000000000000, 0.000000000000000000, 0.000000000000000000 ) ) ;
#2918 = DIRECTION ( 'NONE',  ( -1.000000000000000000, 0.000000000000000000, -0.000000000000000000 ) ) ;
#2919 = VECTOR ( 'NONE', #4815, 1000.000000000000000 ) ;
#2920 = VERTEX_POINT ( 'NONE', #9375 ) ;
#2921 = ORIENTED_EDGE ( 'NONE', *, *, #34868, .T. ) ;
#2922 = DIRECTION ( 'NONE',  ( 0.000000000000000000, 0.000000000000000000, 1.000000000000000000 ) ) ;
#2923 = DIRECTION ( 'NONE',  ( -1.000000000000000000, 0.000000000000000000, -0.000000000000000000 ) ) ;
#2924 = VERTEX_POINT ( 'NONE', #13303 ) ;
#2925 = ORIENTED_EDGE ( 'NONE', *, *, #45711, .T. ) ;
#2926 = DIRECTION ( 'NONE',  ( -1.000000000000000000, 0.000000000000000000, 0.000000000000000000 ) ) ;
#2927 = CARTESIAN_POINT ( 'NONE',  ( 35.50000000000000711, -120.0000000000000000, 5.500000000000000000 ) ) ;
#2928 = CARTESIAN_POINT ( 'NONE',  ( 10.00000000000000000, -25.88420570971419821, 27.13269053701087330 ) ) ;
#2929 = CARTESIAN_POINT ( 'NONE',  ( 0.000000000000000000, 68.27212725128275395, -31.46837873495001503 ) ) ;
#2931 = MANIFOLD_SOLID_BREP ( 'CirPattern1', #42702 ) ;
#2930 = EDGE_CURVE ( 'NONE', #14333, #29462, #24313, .T. ) ;
#2932 = EDGE_CURVE ( 'NONE', #28331, #22374, #13740, .T. ) ;
#2933 = AXIS2_PLACEMENT_3D ( 'NONE', #25449, #40403, #6862 ) ;
#2934 = CARTESIAN_POINT ( 'NONE',  ( 0.000000000000000000, -15.48615015657556171, -39.04073710021360455 ) ) ;
#2935 = DIRECTION ( 'NONE',  ( -1.000000000000000000, -0.000000000000000000, 0.000000000000000000 ) ) ;
#2936 = CARTESIAN_POINT ( 'NONE',  ( 10.00000000000000000, -59.03342792756231461, -46.54456581323868392 ) ) ;
#2937 = CYLINDRICAL_SURFACE ( 'NONE', #33848, 82.00000000000000000 ) ;
#2938 = CYLINDRICAL_SURFACE ( 'NONE', #26975, 16.00000000000000000 ) ;
#2939 = LINE ( 'NONE', #41132, #37323 ) ;
#2940 = ORIENTED_EDGE ( 'NONE', *, *, #33243, .T. ) ;
#2941 = EDGE_CURVE ( 'NONE', #20052, #22205, #21108, .T. ) ;
#2942 = VERTEX_POINT ( 'NONE', #10105 ) ;
#2943 = AXIS2_PLACEMENT_3D ( 'NONE', #43391, #9847, #5696 ) ;
#2944 = CARTESIAN_POINT ( 'NONE',  ( 0.000000000000000000, -64.81221759200379040, 50.23322058963324110 ) ) ;
#2945 = VECTOR ( 'NONE', #16433, 1000.000000000000000 ) ;
#2946 = CARTESIAN_POINT ( 'NONE',  ( 0.000000000000000000, -63.97538442413390669, -51.29473840253292138 ) ) ;
#2947 = EDGE_LOOP ( 'NONE', ( #8786, #22367, #17204, #26752 ) ) ;
#2948 = LINE ( 'NONE', #29622, #39084 ) ;
#2949 = CARTESIAN_POINT ( 'NONE',  ( 0.000000000000000000, 16.23288003029497162, 33.80338159004289622 ) ) ;
#2950 = ORIENTED_EDGE ( 'NONE', *, *, #45645, .F. ) ;
#2951 = DIRECTION ( 'NONE',  ( 0.000000000000000000, 0.000000000000000000, 1.000000000000000000 ) ) ;
#2952 =( GEOMETRIC_REPRESENTATION_CONTEXT ( 3 ) GLOBAL_UNCERTAINTY_ASSIGNED_CONTEXT ( ( #14457 ) ) GLOBAL_UNIT_ASSIGNED_CONTEXT ( ( #13192, #28117, #17094 ) ) REPRESENTATION_CONTEXT ( 'NONE', 'WORKASPACE' ) );
#2953 = ORIENTED_EDGE ( 'NONE', *, *, #1959, .T. ) ;
#2954 = AXIS2_PLACEMENT_3D ( 'NONE', #33914, #37841, #19954 ) ;
#2955 = LINE ( 'NONE', #47038, #10214 ) ;
#2956 = CARTESIAN_POINT ( 'NONE',  ( 5.000000000000000000, 26.79245525562762253, -32.34446384429941901 ) ) ;
#2957 = ORIENTED_EDGE ( 'NONE', *, *, #45172, .T. ) ;
#2958 = CARTESIAN_POINT ( 'NONE',  ( 0.000000000000000000, -67.80270845531921964, 46.11716303203163392 ) ) ;
#2959 = ORIENTED_EDGE ( 'NONE', *, *, #11459, .T. ) ;
#2960 = EDGE_CURVE ( 'NONE', #13263, #35674, #13535, .T. ) ;
#2961 = CARTESIAN_POINT ( 'NONE',  ( 0.000000000000000000, 0.6853352020795618893, -37.58145647212453611 ) ) ;
#2962 = EDGE_LOOP ( 'NONE', ( #38495, #17345, #23916, #2155 ) ) ;
#2963 = CARTESIAN_POINT ( 'NONE',  ( 11.99999999999999822, 46.21855187248630870, 62.20884554314035597 ) ) ;
#2964 = EDGE_CURVE ( 'NONE', #35055, #239, #2753, .T. ) ;
#2965 = ORIENTED_EDGE ( 'NONE', *, *, #42796, .T. ) ;
#2966 = LINE ( 'NONE', #6178, #33174 ) ;
#2967 = CARTESIAN_POINT ( 'NONE',  ( 10.00000000000000000, 37.58145647212453611, 0.6853352020791767529 ) ) ;
#2970 = EDGE_LOOP ( 'NONE', ( #24185, #4959, #11162, #29695 ) ) ;
#2969 = DIRECTION ( 'NONE',  ( 0.000000000000000000, -1.000000000000000000, -1.047444401652940007E-14 ) ) ;
#2968 = AXIS2_PLACEMENT_3D ( 'NONE', #44954, #21942, #11439 ) ;
#2971 = DIRECTION ( 'NONE',  ( 0.000000000000000000, 0.8090169943749487835, -0.5877852522924712497 ) ) ;
#2972 = ORIENTED_EDGE ( 'NONE', *, *, #37365, .F. ) ;
#2973 = DIRECTION ( 'NONE',  ( -1.000000000000000000, 0.000000000000000000, 0.000000000000000000 ) ) ;
#2974 = EDGE_LOOP ( 'NONE', ( #17846, #34037, #15084, #12770 ) ) ;
#2975 = ORIENTED_EDGE ( 'NONE', *, *, #33524, .T. ) ;
#2976 = EDGE_CURVE ( 'NONE', #37949, #43544, #10336, .T. ) ;
#2977 = LINE ( 'NONE', #40668, #21307 ) ;
#2978 = LINE ( 'NONE', #33331, #8973 ) ;
#2979 = CIRCLE ( 'NONE', #13919, 77.49899999999999523 ) ;
#2980 = DIRECTION ( 'NONE',  ( -1.000000000000000000, 0.000000000000000000, 0.000000000000000000 ) ) ;
#2981 = CYLINDRICAL_SURFACE ( 'NONE', #14905, 77.49899999999999523 ) ;
#2982 = LINE ( 'NONE', #39966, #35994 ) ;
#2983 = ORIENTED_EDGE ( 'NONE', *, *, #35523, .F. ) ;
#2984 = VECTOR ( 'NONE', #9958, 1000.000000000000227 ) ;
#2985 = DIRECTION ( 'NONE',  ( -1.000000000000000000, -0.000000000000000000, -0.000000000000000000 ) ) ;
#2986 = DIRECTION ( 'NONE',  ( 0.000000000000000000, 0.9781476007338065770, 0.2079116908177544853 ) ) ;
#2987 = EDGE_CURVE ( 'NONE', #35465, #17019, #42641, .T. ) ;
#2988 = DIRECTION ( 'NONE',  ( 0.000000000000000000, 0.000000000000000000, -1.000000000000000000 ) ) ;
#2989 = VERTEX_POINT ( 'NONE', #40219 ) ;
#2990 = CARTESIAN_POINT ( 'NONE',  ( 10.00000000000000000, 0.000000000000000000, 0.000000000000000000 ) ) ;
#2991 = EDGE_CURVE ( 'NONE', #1412, #35361, #21518, .T. ) ;
#2992 = DIRECTION ( 'NONE',  ( 0.000000000000000000, 0.3090169943749412340, 0.9510565162951556406 ) ) ;
#2993 = DIRECTION ( 'NONE',  ( 0.000000000000000000, -0.7604059656000368150, 0.6494480483301767748 ) ) ;
#2994 = CARTESIAN_POINT ( 'NONE',  ( 26.09152095774781799, -124.8716048804687375, 5.500000000000000000 ) ) ;
#2995 = FACE_OUTER_BOUND ( 'NONE', #47205, .T. ) ;
#2996 = DIRECTION ( 'NONE',  ( -1.000000000000000000, -0.000000000000000000, -0.000000000000000000 ) ) ;
#2997 = STYLED_ITEM ( 'NONE', ( #8975 ), #27490 ) ;
#2998 = DIRECTION ( 'NONE',  ( -1.000000000000000000, 0.000000000000000000, 0.000000000000000000 ) ) ;
#2999 = CARTESIAN_POINT ( 'NONE',  ( 10.00000000000000000, 2.956366410621684260, -75.11725578898465017 ) ) ;
#3000 = ORIENTED_EDGE ( 'NONE', *, *, #17073, .F. ) ;
#3001 = CIRCLE ( 'NONE', #34259, 82.00000000000000000 ) ;
#3002 = EDGE_CURVE ( 'NONE', #26893, #20243, #36046, .T. ) ;
#3003 = EDGE_LOOP ( 'NONE', ( #13930, #10435, #14734, #19264 ) ) ;
#3004 = CYLINDRICAL_SURFACE ( 'NONE', #35549, 31.99999999999998579 ) ;
#3005 = ORIENTED_EDGE ( 'NONE', *, *, #42514, .F. ) ;
#3006 = DIRECTION ( 'NONE',  ( -1.000000000000000000, 0.000000000000000000, 0.000000000000000000 ) ) ;
#3007 =( NAMED_UNIT ( * ) SI_UNIT ( $, .STERADIAN. ) SOLID_ANGLE_UNIT ( ) );
#3008 = CARTESIAN_POINT ( 'NONE',  ( 11.99999999999999822, 41.76937507738788469, 62.50329211542452157 ) ) ;
#3009 = ORIENTED_EDGE ( 'NONE', *, *, #4094, .F. ) ;
#3010 = EDGE_CURVE ( 'NONE', #37417, #9289, #43436, .T. ) ;
#3011 = CARTESIAN_POINT ( 'NONE',  ( 10.00000000000000000, -16.65972982744992592, 80.28980883073749908 ) ) ;
#3012 = VECTOR ( 'NONE', #6818, 1000.000000000000114 ) ;
#3013 = ORIENTED_EDGE ( 'NONE', *, *, #22436, .T. ) ;
#3014 = VECTOR ( 'NONE', #38561, 1000.000000000000000 ) ;
#3015 = CARTESIAN_POINT ( 'NONE',  ( 0.000000000000000000, 29.01471420065673712, -76.69515212745984911 ) ) ;
#3016 = EDGE_LOOP ( 'NONE', ( #32904, #12032, #47094, #6880 ) ) ;
#3017 = ADVANCED_FACE ( 'NONE', ( #36293 ), #29177, .T. ) ;
#3018 = LINE ( 'NONE', #18181, #11722 ) ;
#3019 = CYLINDRICAL_SURFACE ( 'NONE', #43389, 31.99999999999998579 ) ;
#3020 = VERTEX_POINT ( 'NONE', #36529 ) ;
#3021 = EDGE_CURVE ( 'NONE', #45240, #13460, #28473, .T. ) ;
#3022 = FACE_OUTER_BOUND ( 'NONE', #36010, .T. ) ;
#3023 = PRODUCT_DEFINITION_FORMATION_WITH_SPECIFIED_SOURCE ( 'ANY', '', #21428, .NOT_KNOWN. ) ;
#3024 = EDGE_LOOP ( 'NONE', ( #8311, #644, #44359, #28204, #41349, #33885 ) ) ;
#3025 = EDGE_CURVE ( 'NONE', #6278, #8792, #6915, .T. ) ;
#3026 = DIRECTION ( 'NONE',  ( -1.000000000000000000, -0.000000000000000000, 0.000000000000000000 ) ) ;
#3027 = DIRECTION ( 'NONE',  ( 1.000000000000000000, 0.000000000000000000, -0.000000000000000000 ) ) ;
#3028 = DIRECTION ( 'NONE',  ( -1.000000000000000000, 0.000000000000000000, 0.000000000000000000 ) ) ;
#3029 = CIRCLE ( 'NONE', #26496, 77.49900000000002365 ) ;
#3030 = EDGE_CURVE ( 'NONE', #13135, #28683, #19979, .T. ) ;
#3031 = EDGE_LOOP ( 'NONE', ( #23909, #3426, #11098, #27878 ) ) ;
#3032 = CARTESIAN_POINT ( 'NONE',  ( 11.99999999999999822, -6.903761155838323837, 77.19088730480521576 ) ) ;
#3033 = ORIENTED_EDGE ( 'NONE', *, *, #10122, .F. ) ;
#3034 = EDGE_LOOP ( 'NONE', ( #20211, #4846, #8905, #4012 ) ) ;
#3035 = EDGE_CURVE ( 'NONE', #14490, #47828, #10597, .T. ) ;
#3036 = DIRECTION ( 'NONE',  ( 0.000000000000000000, 0.000000000000000000, -1.000000000000000000 ) ) ;
#3037 = CARTESIAN_POINT ( 'NONE',  ( 10.00000000000000000, -40.68715046381921496, -10.41901085202121457 ) ) ;
#3038 = DIRECTION ( 'NONE',  ( 0.000000000000000000, 0.000000000000000000, 1.000000000000000000 ) ) ;
#3039 = DIRECTION ( 'NONE',  ( -1.000000000000000000, 0.000000000000000000, -0.000000000000000000 ) ) ;
#3040 = ORIENTED_EDGE ( 'NONE', *, *, #46065, .F. ) ;
#3041 = DIRECTION ( 'NONE',  ( -0.9038112904824846527, 0.4279312458752990711, 0.000000000000000000 ) ) ;
#3042 = CARTESIAN_POINT ( 'NONE',  ( 11.99999999999999822, -17.28742895386137945, 75.54627589209938776 ) ) ;
#3043 = CARTESIAN_POINT ( 'NONE',  ( 10.00000000000000000, 0.000000000000000000, 0.000000000000000000 ) ) ;
#3044 = DIRECTION ( 'NONE',  ( 0.000000000000000000, 0.000000000000000000, 1.000000000000000000 ) ) ;
#3045 = DIRECTION ( 'NONE',  ( -1.000000000000000000, 0.000000000000000000, -0.000000000000000000 ) ) ;
#3046 = ORIENTED_EDGE ( 'NONE', *, *, #12341, .T. ) ;
#3047 = AXIS2_PLACEMENT_3D ( 'NONE', #40586, #21509, #28617 ) ;
#3048 = DIRECTION ( 'NONE',  ( 0.6575728627325956310, -0.7533909544171997208, -1.230411769795008071E-16 ) ) ;
#3049 = AXIS2_PLACEMENT_3D ( 'NONE', #34196, #38122, #45452 ) ;
#3050 = DIRECTION ( 'NONE',  ( 0.000000000000000000, 0.3826834323650842862, 0.9238795325112890700 ) ) ;
#3051 = CARTESIAN_POINT ( 'NONE',  ( 11.99999999999999822, 0.000000000000000000, 0.000000000000000000 ) ) ;
#3052 = CIRCLE ( 'NONE', #17104, 1.000000000000000888 ) ;
#3053 = DIRECTION ( 'NONE',  ( -1.000000000000000000, 0.000000000000000000, -0.000000000000000000 ) ) ;
#3054 = ADVANCED_FACE ( 'NONE', ( #10599, #5973 ), #21352, .T. ) ;
#3055 = CARTESIAN_POINT ( 'NONE',  ( 0.000000000000000000, 0.000000000000000000, 0.000000000000000000 ) ) ;
#3056 = DIRECTION ( 'NONE',  ( 1.000000000000000000, 0.000000000000000000, 0.000000000000000000 ) ) ;
#3057 = EDGE_LOOP ( 'NONE', ( #18396, #24074, #32245, #32297 ) ) ;
#3058 = LINE ( 'NONE', #17260, #40245 ) ;
#3059 = ADVANCED_FACE ( 'NONE', ( #3225 ), #18148, .T. ) ;
#3060 = CARTESIAN_POINT ( 'NONE',  ( 10.00000000000000000, 55.20638768913760686, 51.02545421589343988 ) ) ;
#3061 = ORIENTED_EDGE ( 'NONE', *, *, #37337, .T. ) ;
#3062 = EDGE_CURVE ( 'NONE', #20359, #39585, #4350, .T. ) ;
#3063 = DIRECTION ( 'NONE',  ( -1.000000000000000000, 0.000000000000000000, 0.000000000000000000 ) ) ;
#3064 = EDGE_LOOP ( 'NONE', ( #41739, #6003, #17795, #31442 ) ) ;
#3065 = ORIENTED_EDGE ( 'NONE', *, *, #44702, .T. ) ;
#3066 = FACE_OUTER_BOUND ( 'NONE', #16381, .T. ) ;
#3067 = VECTOR ( 'NONE', #23921, 1000.000000000000000 ) ;
#3068 = EDGE_CURVE ( 'NONE', #18838, #35058, #37944, .T. ) ;
#3069 = CARTESIAN_POINT ( 'NONE',  ( 10.00000000000000000, -75.11725578898466438, -2.956366410621452001 ) ) ;
#3071 = ORIENTED_EDGE ( 'NONE', *, *, #25984, .T. ) ;
#3070 = CARTESIAN_POINT ( 'NONE',  ( 11.99999999999999822, 0.000000000000000000, 0.000000000000000000 ) ) ;
#3072 = ORIENTED_EDGE ( 'NONE', *, *, #1558, .T. ) ;
#3073 = CARTESIAN_POINT ( 'NONE',  ( 10.00000000000000000, -15.33399622253540251, 80.55351364060582853 ) ) ;
#3074 = ORIENTED_EDGE ( 'NONE', *, *, #1825, .T. ) ;
#3075 = EDGE_CURVE ( 'NONE', #6056, #33596, #32405, .T. ) ;
#3076 = EDGE_LOOP ( 'NONE', ( #34244, #18823, #6534, #26464 ) ) ;
#3077 = ORIENTED_EDGE ( 'NONE', *, *, #34407, .T. ) ;
#3078 = DIRECTION ( 'NONE',  ( 0.000000000000000000, 0.000000000000000000, 1.000000000000000000 ) ) ;
#3080 = ORIENTED_EDGE ( 'NONE', *, *, #26244, .F. ) ;
#3079 = CYLINDRICAL_SURFACE ( 'NONE', #19589, 42.00000000000000000 ) ;
#3081 = DIRECTION ( 'NONE',  ( -1.000000000000000000, 0.000000000000000000, 0.000000000000000000 ) ) ;
#3082 = ORIENTED_EDGE ( 'NONE', *, *, #32089, .T. ) ;
#3083 = ORIENTED_EDGE ( 'NONE', *, *, #35874, .F. ) ;
#3084 = AXIS2_PLACEMENT_3D ( 'NONE', #38500, #45349, #34824 ) ;
#3085 = DIRECTION ( 'NONE',  ( 0.000000000000000000, 0.8090169943749487835, -0.5877852522924713607 ) ) ;
#3086 = ORIENTED_EDGE ( 'NONE', *, *, #22996, .F. ) ;
#3087 = EDGE_CURVE ( 'NONE', #2339, #35473, #7370, .T. ) ;
#3088 = DIRECTION ( 'NONE',  ( 1.000000000000000000, 0.000000000000000000, 0.000000000000000000 ) ) ;
#3089 = DIRECTION ( 'NONE',  ( 0.000000000000000000, 0.8910065241883690090, -0.4539904997395446395 ) ) ;
#3090 = ADVANCED_FACE ( 'NONE', ( #7401 ), #18414, .F. ) ;
#3091 = FACE_BOUND ( 'NONE', #16469, .T. ) ;
#3092 = ORIENTED_EDGE ( 'NONE', *, *, #35353, .F. ) ;
#3093 = CARTESIAN_POINT ( 'NONE',  ( 15.00000000000000000, 6.762365576493647445, 25.66652317338391498 ) ) ;
#3094 = DIRECTION ( 'NONE',  ( 0.000000000000000000, 0.000000000000000000, 1.000000000000000000 ) ) ;
#3095 = DIRECTION ( 'NONE',  ( 0.000000000000000000, 0.000000000000000000, 1.000000000000000000 ) ) ;
#3096 = CARTESIAN_POINT ( 'NONE',  ( 5.999999999999999112, 67.80270845531887858, 46.11716303203210288 ) ) ;
#3097 = DIRECTION ( 'NONE',  ( 0.000000000000000000, 0.000000000000000000, 1.000000000000000000 ) ) ;
#3098 = ORIENTED_EDGE ( 'NONE', *, *, #15540, .T. ) ;
#3099 = DIRECTION ( 'NONE',  ( -1.000000000000000000, 0.000000000000000000, 0.000000000000000000 ) ) ;
#3100 = ORIENTED_EDGE ( 'NONE', *, *, #43406, .F. ) ;
#3101 = CARTESIAN_POINT ( 'NONE',  ( 2.047646702416564324, -96.54137380445985173, -2.500000000000000000 ) ) ;
#3102 = CARTESIAN_POINT ( 'NONE',  ( 5.999999999999999112, 46.11716303203186840, 67.80270845531904911 ) ) ;
#3103 = DIRECTION ( 'NONE',  ( -1.000000000000000000, -0.000000000000000000, -0.000000000000000000 ) ) ;
#3104 = FACE_OUTER_BOUND ( 'NONE', #18786, .T. ) ;
#3105 = CARTESIAN_POINT ( 'NONE',  ( 11.99999999999999822, 33.71516098798849015, -74.74816331893393340 ) ) ;
#3106 = AXIS2_PLACEMENT_3D ( 'NONE', #35258, #39178, #3160 ) ;
#3107 = CARTESIAN_POINT ( 'NONE',  ( -22.67106064244953245, -113.6342314410295842, 5.500000000000000000 ) ) ;
#3108 = FACE_OUTER_BOUND ( 'NONE', #37345, .T. ) ;
#3109 = CIRCLE ( 'NONE', #5469, 15.99999999999999822 ) ;
#3110 = AXIS2_PLACEMENT_3D ( 'NONE', #27172, #46015, #45511 ) ;
#3111 = CARTESIAN_POINT ( 'NONE',  ( -22.67106064244953245, -113.6342314410295842, -5.500000000000000000 ) ) ;
#3112 =( NAMED_UNIT ( * ) SI_UNIT ( $, .STERADIAN. ) SOLID_ANGLE_UNIT ( ) );
#3113 = CARTESIAN_POINT ( 'NONE',  ( 0.000000000000000000, 21.32104025579158701, -30.84782396557194772 ) ) ;
#3114 = AXIS2_PLACEMENT_3D ( 'NONE', #42240, #42015, #12629 ) ;
#3115 = ORIENTED_EDGE ( 'NONE', *, *, #19580, .F. ) ;
#3116 = ORIENTED_EDGE ( 'NONE', *, *, #17112, .T. ) ;
#3117 = AXIS2_PLACEMENT_3D ( 'NONE', #23505, #3948, #19823 ) ;
#3118 = ORIENTED_EDGE ( 'NONE', *, *, #21084, .F. ) ;
#3119 = ADVANCED_FACE ( 'NONE', ( #26248 ), #11071, .F. ) ;
#3120 = LINE ( 'NONE', #32281, #46045 ) ;
#3121 = CARTESIAN_POINT ( 'NONE',  ( -6.170112525937322623, 10.87104923258428180, 125.0000000000000000 ) ) ;
#3122 = ORIENTED_EDGE ( 'NONE', *, *, #25130, .F. ) ;
#3123 = CARTESIAN_POINT ( 'NONE',  ( 0.000000000000000000, 0.000000000000000000, 0.000000000000000000 ) ) ;
#3124 = ORIENTED_EDGE ( 'NONE', *, *, #14091, .T. ) ;
#3125 = ORIENTED_EDGE ( 'NONE', *, *, #36938, .F. ) ;
#3126 = EDGE_CURVE ( 'NONE', #2457, #30556, #23794, .T. ) ;
#3127 = EDGE_CURVE ( 'NONE', #199, #24143, #42575, .T. ) ;
#3128 = EDGE_CURVE ( 'NONE', #23303, #17771, #36305, .T. ) ;
#3129 = VECTOR ( 'NONE', #34152, 1000.000000000000000 ) ;
#3130 = LINE ( 'NONE', #21517, #42294 ) ;
#3132 = ORIENTED_EDGE ( 'NONE', *, *, #17169, .T. ) ;
#3131 = AXIS2_PLACEMENT_3D ( 'NONE', #24523, #28434, #24993 ) ;
#3133 = DIRECTION ( 'NONE',  ( -1.000000000000000000, -0.000000000000000000, 0.000000000000000000 ) ) ;
#3134 = VERTEX_POINT ( 'NONE', #26486 ) ;
#3135 = EDGE_LOOP ( 'NONE', ( #40906, #2458, #14966, #16279 ) ) ;
#3136 = EDGE_CURVE ( 'NONE', #6704, #9220, #19780, .T. ) ;
#3137 = DIRECTION ( 'NONE',  ( -1.000000000000000000, 0.000000000000000000, 0.000000000000000000 ) ) ;
#3138 = AXIS2_PLACEMENT_3D ( 'NONE', #35853, #2320, #31004 ) ;
#3139 = AXIS2_PLACEMENT_3D ( 'NONE', #39939, #47987, #32358 ) ;
#3140 = EDGE_CURVE ( 'NONE', #43853, #8436, #47246, .T. ) ;
#3141 = DIRECTION ( 'NONE',  ( 0.000000000000000000, -0.000000000000000000, 1.000000000000000000 ) ) ;
#3142 = CARTESIAN_POINT ( 'NONE',  ( 4.574237413256328308E-15, 3.992474787516289480E-15, 42.00000000000001421 ) ) ;
#3143 = ORIENTED_EDGE ( 'NONE', *, *, #36549, .T. ) ;
#3144 = VECTOR ( 'NONE', #39462, 1000.000000000000000 ) ;
#3145 = ORIENTED_EDGE ( 'NONE', *, *, #25841, .T. ) ;
#3146 = AXIS2_PLACEMENT_3D ( 'NONE', #19121, #7862, #37727 ) ;
#3147 = DIRECTION ( 'NONE',  ( 1.000000000000000000, 0.000000000000000000, 0.000000000000000000 ) ) ;
#3148 = CARTESIAN_POINT ( 'NONE',  ( 11.99999999999999822, 80.55351364060611274, -15.33399622253397609 ) ) ;
#3149 = VERTEX_POINT ( 'NONE', #10832 ) ;
#3150 = AXIS2_PLACEMENT_3D ( 'NONE', #24004, #42608, #13461 ) ;
#3151 = VERTEX_POINT ( 'NONE', #1200 ) ;
#3152 = DIRECTION ( 'NONE',  ( -0.4279312458752977388, -0.9038112904824853189, 0.000000000000000000 ) ) ;
#3153 = LINE ( 'NONE', #10517, #5910 ) ;
#3154 = VERTEX_POINT ( 'NONE', #29907 ) ;
#3155 = EDGE_LOOP ( 'NONE', ( #31976, #33090, #13576, #3342 ) ) ;
#3156 = FACE_OUTER_BOUND ( 'NONE', #2671, .T. ) ;
#3157 = DIRECTION ( 'NONE',  ( -1.000000000000000000, 0.000000000000000000, -0.000000000000000000 ) ) ;
#3158 = LINE ( 'NONE', #31860, #9695 ) ;
#3159 = CARTESIAN_POINT ( 'NONE',  ( 0.000000000000000000, 0.000000000000000000, 125.0000000000000000 ) ) ;
#3160 = DIRECTION ( 'NONE',  ( 0.000000000000000000, 0.9238795325112877377, -0.3826834323650873948 ) ) ;
#3161 = CARTESIAN_POINT ( 'NONE',  ( 11.99999999999999822, 73.95703589264006439, -23.16143007188350822 ) ) ;
#3162 = CARTESIAN_POINT ( 'NONE',  ( 4.999999999999999112, 10.41901085202135491, -40.68715046381917944 ) ) ;
#3163 = CARTESIAN_POINT ( 'NONE',  ( 0.000000000000000000, 0.000000000000000000, -56.19999999999998863 ) ) ;
#3164 = DIRECTION ( 'NONE',  ( -1.000000000000000000, 0.000000000000000000, -0.000000000000000000 ) ) ;
#3165 = LINE ( 'NONE', #33284, #18315 ) ;
#3166 = LINE ( 'NONE', #33035, #20124 ) ;
#3167 = ORIENTED_EDGE ( 'NONE', *, *, #3588, .T. ) ;
#3168 = ORIENTED_EDGE ( 'NONE', *, *, #43733, .T. ) ;
#3169 = EDGE_LOOP ( 'NONE', ( #29021, #30776, #30545, #35616 ) ) ;
#3170 = VECTOR ( 'NONE', #9899, 1000.000000000000000 ) ;
#3171 = EDGE_CURVE ( 'NONE', #17403, #911, #15209, .T. ) ;
#3172 = VECTOR ( 'NONE', #38870, 1000.000000000000000 ) ;
#3173 = PRODUCT_DEFINITION_CONTEXT ( 'detailed design', #695, 'design' ) ;
#3174 = DIRECTION ( 'NONE',  ( -1.000000000000000000, -0.000000000000000000, -0.000000000000000000 ) ) ;
#3175 = AXIS2_PLACEMENT_3D ( 'NONE', #13525, #2500, #24791 ) ;
#3176 = AXIS2_PLACEMENT_3D ( 'NONE', #33251, #26633, #29813 ) ;
#3177 = EDGE_CURVE ( 'NONE', #8888, #40065, #43342, .T. ) ;
#3178 = DIRECTION ( 'NONE',  ( -1.000000000000000000, 0.000000000000000000, 0.000000000000000000 ) ) ;
#3179 = EDGE_CURVE ( 'NONE', #27388, #4066, #15762, .T. ) ;
#3180 = VERTEX_POINT ( 'NONE', #1447 ) ;
#3181 = CIRCLE ( 'NONE', #34453, 42.00000000000000000 ) ;
#3182 = AXIS2_PLACEMENT_3D ( 'NONE', #41109, #37911, #15874 ) ;
#3183 = APPLICATION_CONTEXT ( 'automotive_design' ) ;
#3184 = CARTESIAN_POINT ( 'NONE',  ( 11.99999999999999822, 33.71516098798741012, 74.74816331893441657 ) ) ;
#3185 = ORIENTED_EDGE ( 'NONE', *, *, #11289, .F. ) ;
#3186 = DIRECTION ( 'NONE',  ( -1.000000000000000000, -0.000000000000000000, 0.000000000000000000 ) ) ;
#3187 = ORIENTED_EDGE ( 'NONE', *, *, #22923, .T. ) ;
#3188 = VERTEX_POINT ( 'NONE', #30168 ) ;
#3189 = CARTESIAN_POINT ( 'NONE',  ( 11.99999999999999822, -8.830959090341869100, -74.65491531819127147 ) ) ;
#3190 = EDGE_CURVE ( 'NONE', #27256, #1470, #1688, .T. ) ;
#3191 = EDGE_CURVE ( 'NONE', #45171, #17275, #16525, .T. ) ;
#3192 = CARTESIAN_POINT ( 'NONE',  ( 10.00000000000000000, 0.000000000000000000, 0.000000000000000000 ) ) ;
#3193 = VERTEX_POINT ( 'NONE', #5122 ) ;
#3194 = DIRECTION ( 'NONE',  ( 0.000000000000000000, 0.000000000000000000, 1.000000000000000000 ) ) ;
#3195 = ORIENTED_EDGE ( 'NONE', *, *, #9994, .F. ) ;
#3196 = CARTESIAN_POINT ( 'NONE',  ( 10.00000000000000000, 33.17418723428307459, 17.67226234102837878 ) ) ;
#3197 = FACE_OUTER_BOUND ( 'NONE', #22845, .T. ) ;
#3198 = EDGE_LOOP ( 'NONE', ( #11283, #46464, #34828, #29564 ) ) ;
#3199 = LINE ( 'NONE', #11300, #14336 ) ;
#3200 = DIRECTION ( 'NONE',  ( 0.000000000000000000, -0.9510565162951507556, 0.3090169943749561110 ) ) ;
#3201 = EDGE_CURVE ( 'NONE', #18192, #45952, #40683, .T. ) ;
#3202 = CIRCLE ( 'NONE', #103, 77.49900000000002365 ) ;
#3203 = LINE ( 'NONE', #36505, #23425 ) ;
#3204 = CARTESIAN_POINT ( 'NONE',  ( 10.00000000000000000, 0.000000000000000000, 0.000000000000000000 ) ) ;
#3205 = ORIENTED_EDGE ( 'NONE', *, *, #22373, .F. ) ;
#3206 = AXIS2_PLACEMENT_3D ( 'NONE', #5029, #31468, #16289 ) ;
#3207 = DIRECTION ( 'NONE',  ( 0.000000000000000000, 0.000000000000000000, 1.000000000000000000 ) ) ;
#3208 = ORIENTED_EDGE ( 'NONE', *, *, #20823, .F. ) ;
#3209 = ORIENTED_EDGE ( 'NONE', *, *, #21139, .T. ) ;
#3210 = LINE ( 'NONE', #41174, #42431 ) ;
#3211 = DIRECTION ( 'NONE',  ( 0.000000000000000000, 0.000000000000000000, 1.000000000000000000 ) ) ;
#3212 = AXIS2_PLACEMENT_3D ( 'NONE', #24002, #5393, #8567 ) ;
#3213 = VECTOR ( 'NONE', #32945, 1000.000000000000000 ) ;
#3214 = DIRECTION ( 'NONE',  ( -1.000000000000000000, -0.000000000000000000, 0.000000000000000000 ) ) ;
#3215 = LINE ( 'NONE', #21342, #8642 ) ;
#3216 = DIRECTION ( 'NONE',  ( -1.000000000000000000, -0.000000000000000000, 0.000000000000000000 ) ) ;
#3217 = EDGE_LOOP ( 'NONE', ( #2015, #40552, #32867, #25486 ) ) ;
#3218 = FACE_OUTER_BOUND ( 'NONE', #27755, .T. ) ;
#3219 = AXIS2_PLACEMENT_3D ( 'NONE', #18576, #12690, #23217 ) ;
#3220 = FACE_OUTER_BOUND ( 'NONE', #31301, .T. ) ;
#3221 = AXIS2_PLACEMENT_3D ( 'NONE', #40861, #11251, #36926 ) ;
#3222 = DIRECTION ( 'NONE',  ( 1.000000000000000000, 0.000000000000000000, -0.000000000000000000 ) ) ;
#3223 = ORIENTED_EDGE ( 'NONE', *, *, #47675, .F. ) ;
#3224 = CARTESIAN_POINT ( 'NONE',  ( 15.00000000000000000, -3.948201729842032215, 23.21447184625297666 ) ) ;
#3225 = FACE_OUTER_BOUND ( 'NONE', #20798, .T. ) ;
#3226 = DIRECTION ( 'NONE',  ( 0.000000000000000000, 0.000000000000000000, 1.000000000000000000 ) ) ;
#3227 = CARTESIAN_POINT ( 'NONE',  ( 10.00000000000000000, -41.19522573413687638, -65.64334221924953283 ) ) ;
#3228 = AXIS2_PLACEMENT_3D ( 'NONE', #24463, #39408, #5389 ) ;
#3229 = ORIENTED_EDGE ( 'NONE', *, *, #4162, .F. ) ;
#3230 = DIRECTION ( 'NONE',  ( 1.000000000000000000, 0.000000000000000000, 0.000000000000000000 ) ) ;
#3231 = DIRECTION ( 'NONE',  ( -1.000000000000000000, 0.000000000000000000, 0.000000000000000000 ) ) ;
#3232 = DIRECTION ( 'NONE',  ( -1.000000000000000000, 0.000000000000000000, 0.000000000000000000 ) ) ;
#3233 = LINE ( 'NONE', #47780, #27268 ) ;
#3234 = VERTEX_POINT ( 'NONE', #3480 ) ;
#3235 = EDGE_CURVE ( 'NONE', #23364, #10143, #33344, .T. ) ;
#3236 = CARTESIAN_POINT ( 'NONE',  ( 11.99999999999999822, -59.46389618801999433, 49.70050353004867816 ) ) ;
#3237 = VERTEX_POINT ( 'NONE', #9980 ) ;
#3238 = LINE ( 'NONE', #14273, #29209 ) ;
#3239 = EDGE_CURVE ( 'NONE', #15601, #16667, #29023, .T. ) ;
#3240 = DIRECTION ( 'NONE',  ( -0.7533909544171990547, -0.6575728627325962972, -1.172970231617250413E-15 ) ) ;
#3241 = DIRECTION ( 'NONE',  ( 0.6575728627325956310, -0.7533909544171996098, 0.000000000000000000 ) ) ;
#3242 = EDGE_CURVE ( 'NONE', #22090, #15687, #42569, .T. ) ;
#3243 = ORIENTED_EDGE ( 'NONE', *, *, #36006, .T. ) ;
#3244 = MANIFOLD_SOLID_BREP ( 'Fillet1', #6745 ) ;
#3245 = AXIS2_PLACEMENT_3D ( 'NONE', #22206, #33934, #18533 ) ;
#3246 = AXIS2_PLACEMENT_3D ( 'NONE', #2541, #40011, #24832 ) ;
#3247 = VECTOR ( 'NONE', #47516, 1000.000000000000000 ) ;
#3248 = CARTESIAN_POINT ( 'NONE',  ( 0.000000000000000000, 54.21277698773675979, 55.38113227695801299 ) ) ;
#3249 = ORIENTED_EDGE ( 'NONE', *, *, #43702, .T. ) ;
#3250 = ORIENTED_EDGE ( 'NONE', *, *, #44216, .F. ) ;
#3251 = VECTOR ( 'NONE', #29052, 1000.000000000000000 ) ;
#3252 = EDGE_CURVE ( 'NONE', #20905, #10988, #16860, .T. ) ;
#3253 = ADVANCED_FACE ( 'NONE', ( #28108 ), #9496, .T. ) ;
#3254 = DIRECTION ( 'NONE',  ( 0.000000000000000000, -0.9945218953682742891, 0.1045284632676436315 ) ) ;
#3255 = EDGE_CURVE ( 'NONE', #9902, #23423, #32264, .T. ) ;
#3256 = CARTESIAN_POINT ( 'NONE',  ( 5.000000000000002665, -16.65972982744991882, 80.28980883073752750 ) ) ;
#3257 = DIRECTION ( 'NONE',  ( 0.000000000000000000, -0.9510565162951565288, 0.3090169943749382919 ) ) ;
#3258 = CIRCLE ( 'NONE', #918, 82.00000000000000000 ) ;
#3259 = VERTEX_POINT ( 'NONE', #13669 ) ;
#3260 = CARTESIAN_POINT ( 'NONE',  ( 0.000000000000000000, -28.89263327155693517, -71.91182617369219088 ) ) ;
#3261 = VERTEX_POINT ( 'NONE', #32035 ) ;
#3262 = DIRECTION ( 'NONE',  ( -1.000000000000000000, -0.000000000000000000, 0.000000000000000000 ) ) ;
#3263 = LINE ( 'NONE', #18188, #1499 ) ;
#3264 = CARTESIAN_POINT ( 'NONE',  ( 11.99999999999999822, -60.67117009219176538, 55.16347631943021668 ) ) ;
#3265 = EDGE_CURVE ( 'NONE', #27284, #36359, #7753, .T. ) ;
#3266 = DIRECTION ( 'NONE',  ( -1.000000000000000000, 0.000000000000000000, -0.000000000000000000 ) ) ;
#3267 = ORIENTED_EDGE ( 'NONE', *, *, #14213, .T. ) ;
#3268 = DIRECTION ( 'NONE',  ( 0.000000000000000000, 0.000000000000000000, 1.000000000000000000 ) ) ;
#3269 = ORIENTED_EDGE ( 'NONE', *, *, #19805, .T. ) ;
#3270 = VERTEX_POINT ( 'NONE', #35206 ) ;
#3271 = DIRECTION ( 'NONE',  ( 0.000000000000000000, -0.9238795325112906243, 0.3826834323650805669 ) ) ;
#3272 = FACE_OUTER_BOUND ( 'NONE', #33366, .T. ) ;
#3273 = CARTESIAN_POINT ( 'NONE',  ( 0.000000000000000000, 35.95386929396241271, 10.96151621346552751 ) ) ;
#3274 = DIRECTION ( 'NONE',  ( -1.000000000000000000, -0.000000000000000000, 0.000000000000000000 ) ) ;
#3275 = ORIENTED_EDGE ( 'NONE', *, *, #28327, .F. ) ;
#3276 = DIRECTION ( 'NONE',  ( -1.000000000000000000, 0.000000000000000000, 0.000000000000000000 ) ) ;
#3277 = CARTESIAN_POINT ( 'NONE',  ( -11.59999999999999787, 0.000000000000000000, 52.00000000000002132 ) ) ;
#3278 = DIRECTION ( 'NONE',  ( 0.000000000000000000, 0.000000000000000000, 1.000000000000000000 ) ) ;
#3279 = CYLINDRICAL_SURFACE ( 'NONE', #41601, 16.00000000000000000 ) ;
#3280 = DIRECTION ( 'NONE',  ( -1.000000000000000000, -0.000000000000000000, 0.000000000000000000 ) ) ;
#3281 = ORIENTED_EDGE ( 'NONE', *, *, #17632, .T. ) ;
#3282 = DIRECTION ( 'NONE',  ( 0.000000000000000000, -0.9876883405951358830, -0.1564344650402420822 ) ) ;
#3283 = DIRECTION ( 'NONE',  ( 0.000000000000000000, -0.7071067811865389130, -0.7071067811865561215 ) ) ;
#3284 = AXIS2_PLACEMENT_3D ( 'NONE', #45795, #22777, #18851 ) ;
#3285 = DIRECTION ( 'NONE',  ( 0.3090169943749448977, 0.9510565162951543083, 0.000000000000000000 ) ) ;
#3286 = CARTESIAN_POINT ( 'NONE',  ( 6.000000000000000000, 34.94270380257639630, 74.18225833017899618 ) ) ;
#3287 = VECTOR ( 'NONE', #39059, 1000.000000000000000 ) ;
#3288 = CARTESIAN_POINT ( 'NONE',  ( 5.822613034544236399, -142.8165987265839760, 5.500000000000000000 ) ) ;
#3289 = DIRECTION ( 'NONE',  ( 1.000000000000000000, -0.000000000000000000, -0.000000000000000000 ) ) ;
#3290 = CARTESIAN_POINT ( 'NONE',  ( 10.00000000000000000, -73.72996012237449293, 14.67089635893687571 ) ) ;
#3291 = ORIENTED_EDGE ( 'NONE', *, *, #19897, .F. ) ;
#3292 = CARTESIAN_POINT ( 'NONE',  ( 10.00000000000000000, -75.11764819372149304, 2.946379043146075905 ) ) ;
#3293 = AXIS2_PLACEMENT_3D ( 'NONE', #9939, #24864, #21901 ) ;
#3294 = EDGE_CURVE ( 'NONE', #45623, #6665, #3842, .T. ) ;
#3295 = ADVANCED_FACE ( 'NONE', ( #28340 ), #31558, .T. ) ;
#3296 = CARTESIAN_POINT ( 'NONE',  ( 0.000000000000000000, 0.000000000000000000, 0.000000000000000000 ) ) ;
#3297 = EDGE_CURVE ( 'NONE', #12549, #23907, #38899, .T. ) ;
#3298 = EDGE_LOOP ( 'NONE', ( #12279, #35398, #34194, #8022 ) ) ;
#3299 = EDGE_CURVE ( 'NONE', #12589, #8139, #6088, .T. ) ;
#3300 = EDGE_CURVE ( 'NONE', #20106, #31210, #39264, .T. ) ;
#3301 = ORIENTED_EDGE ( 'NONE', *, *, #3582, .F. ) ;
#3302 = DIRECTION ( 'NONE',  ( -1.000000000000000000, -0.000000000000000000, 0.000000000000000000 ) ) ;
#3303 = ORIENTED_EDGE ( 'NONE', *, *, #32493, .F. ) ;
#3304 = EDGE_CURVE ( 'NONE', #18104, #15496, #22065, .T. ) ;
#3305 = ORIENTED_EDGE ( 'NONE', *, *, #41146, .T. ) ;
#3306 = AXIS2_PLACEMENT_3D ( 'NONE', #44125, #47324, #25259 ) ;
#3307 = CIRCLE ( 'NONE', #36917, 16.00000000000000000 ) ;
#3308 = CARTESIAN_POINT ( 'NONE',  ( 10.00000000000000000, -71.21200624218823805, 40.65526001592589722 ) ) ;
#3309 = ORIENTED_EDGE ( 'NONE', *, *, #44430, .F. ) ;
#3310 = EDGE_CURVE ( 'NONE', #24385, #34476, #34560, .T. ) ;
#3311 = DIRECTION ( 'NONE',  ( -1.000000000000000000, -0.000000000000000000, 0.000000000000000000 ) ) ;
#3312 = VECTOR ( 'NONE', #40845, 1000.000000000000000 ) ;
#3313 = DIRECTION ( 'NONE',  ( -1.000000000000000000, 0.000000000000000000, 0.000000000000000000 ) ) ;
#3314 = ORIENTED_EDGE ( 'NONE', *, *, #16929, .F. ) ;
#3315 = CARTESIAN_POINT ( 'NONE',  ( 10.00000000000000000, 77.32052557432841411, 5.256550761633138613 ) ) ;
#3316 = AXIS2_PLACEMENT_3D ( 'NONE', #28094, #20492, #12442 ) ;
#3317 = ORIENTED_EDGE ( 'NONE', *, *, #11839, .F. ) ;
#3318 = ORIENTED_EDGE ( 'NONE', *, *, #25893, .T. ) ;
#3319 = AXIS2_PLACEMENT_3D ( 'NONE', #42183, #41706, #23576 ) ;
#3320 = VERTEX_POINT ( 'NONE', #47896 ) ;
#3321 = CYLINDRICAL_SURFACE ( 'NONE', #2191, 37.49900000000000233 ) ;
#3322 = LINE ( 'NONE', #29287, #14933 ) ;
#3323 = ADVANCED_FACE ( 'NONE', ( #3104 ), #29789, .F. ) ;
#3324 = FACE_BOUND ( 'NONE', #22303, .T. ) ;
#3325 = AXIS2_PLACEMENT_3D ( 'NONE', #42013, #4559, #38830 ) ;
#3326 = ORIENTED_EDGE ( 'NONE', *, *, #25398, .F. ) ;
#3327 = ORIENTED_EDGE ( 'NONE', *, *, #30178, .T. ) ;
#3328 = CYLINDRICAL_SURFACE ( 'NONE', #25545, 82.00000000000000000 ) ;
#3329 = ORIENTED_EDGE ( 'NONE', *, *, #7204, .T. ) ;
#3330 = CARTESIAN_POINT ( 'NONE',  ( 11.99999999999999822, -58.39081064771786345, 50.95692526931308919 ) ) ;
#3331 = AXIS2_PLACEMENT_3D ( 'NONE', #46850, #28486, #24812 ) ;
#3332 = CYLINDRICAL_SURFACE ( 'NONE', #4548, 16.00000000000000000 ) ;
#3333 = CARTESIAN_POINT ( 'NONE',  ( 10.00000000000000000, -36.73666225445940370, 65.58780272294062286 ) ) ;
#3334 = DIRECTION ( 'NONE',  ( -1.000000000000000000, 0.000000000000000000, 0.000000000000000000 ) ) ;
#3335 = CYLINDRICAL_SURFACE ( 'NONE', #46372, 31.99999999999999289 ) ;
#3336 = LINE ( 'NONE', #18022, #26437 ) ;
#3337 = LINE ( 'NONE', #36871, #30485 ) ;
#3338 = ADVANCED_FACE ( 'NONE', ( #10467 ), #44479, .T. ) ;
#3339 = DIRECTION ( 'NONE',  ( -1.000000000000000000, 0.000000000000000000, 0.000000000000000000 ) ) ;
#3340 = VERTEX_POINT ( 'NONE', #40344 ) ;
#3341 = DIRECTION ( 'NONE',  ( -1.000000000000000000, 0.000000000000000000, 0.000000000000000000 ) ) ;
#3342 = ORIENTED_EDGE ( 'NONE', *, *, #39541, .T. ) ;
#3343 = DIRECTION ( 'NONE',  ( 0.000000000000000000, -0.07845909572783055230, -0.9969173337331290741 ) ) ;
#3344 = DIRECTION ( 'NONE',  ( -1.000000000000000000, 0.000000000000000000, 0.000000000000000000 ) ) ;
#3345 = VECTOR ( 'NONE', #54, 1000.000000000000000 ) ;
#3346 = CARTESIAN_POINT ( 'NONE',  ( 5.000000000000000000, -68.55367621811112144, -44.99326035066125939 ) ) ;
#3347 = CARTESIAN_POINT ( 'NONE',  ( 10.00000000000000000, 0.000000000000000000, 0.000000000000000000 ) ) ;
#3349 = CIRCLE ( 'NONE', #36952, 82.00000000000000000 ) ;
#3348 = DIRECTION ( 'NONE',  ( -0.3853207896976523772, 0.9227826878668550226, 0.000000000000000000 ) ) ;
#3350 = EDGE_CURVE ( 'NONE', #22595, #7784, #19003, .T. ) ;
#3351 = CIRCLE ( 'NONE', #5713, 77.49900000000002365 ) ;
#3352 = DIRECTION ( 'NONE',  ( -1.000000000000000000, -0.000000000000000000, 0.000000000000000000 ) ) ;
#3353 = LINE ( 'NONE', #3852, #33138 ) ;
#3354 = ADVANCED_FACE ( 'NONE', ( #41071 ), #40568, .F. ) ;
#3355 = VECTOR ( 'NONE', #28045, 1000.000000000000000 ) ;
#3356 = CIRCLE ( 'NONE', #23002, 19.05560546998412974 ) ;
#3357 = AXIS2_PLACEMENT_3D ( 'NONE', #15810, #863, #37114 ) ;
#3358 = CARTESIAN_POINT ( 'NONE',  ( 2.047646702416564768, -96.54137380445985173, 5.500000000000000000 ) ) ;
#3359 = CARTESIAN_POINT ( 'NONE',  ( 0.000000000000000000, 41.19522573413826194, -65.64334221924865176 ) ) ;
#3360 = EDGE_CURVE ( 'NONE', #26085, #31548, #30236, .T. ) ;
#3361 = ORIENTED_EDGE ( 'NONE', *, *, #38679, .T. ) ;
#3362 = ORIENTED_EDGE ( 'NONE', *, *, #41369, .F. ) ;
#3363 = CIRCLE ( 'NONE', #44009, 31.99999999999998934 ) ;
#3364 = EDGE_CURVE ( 'NONE', #14436, #25362, #18535, .T. ) ;
#3365 = ORIENTED_EDGE ( 'NONE', *, *, #11147, .T. ) ;
#3366 = DIRECTION ( 'NONE',  ( -0.000000000000000000, 0.4067366430757998752, 0.9135454576426010886 ) ) ;
#3367 = CARTESIAN_POINT ( 'NONE',  ( -3.000000000000000000, 22.07842321921481243, 8.187992925817422218 ) ) ;
#3368 = EDGE_LOOP ( 'NONE', ( #24723, #11491, #31582, #33311 ) ) ;
#3369 = CARTESIAN_POINT ( 'NONE',  ( -10.43921258969510824, -98.89258801967538659, 5.500000000000000000 ) ) ;
#3370 = VERTEX_POINT ( 'NONE', #17805 ) ;
#3371 = ORIENTED_EDGE ( 'NONE', *, *, #23331, .F. ) ;
#3372 = VECTOR ( 'NONE', #31147, 1000.000000000000000 ) ;
#3373 = AXIS2_PLACEMENT_3D ( 'NONE', #9987, #25151, #6097 ) ;
#3374 = DIRECTION ( 'NONE',  ( 0.000000000000000000, 0.9876883405951372152, 0.1564344650402346160 ) ) ;
#3375 = DIRECTION ( 'NONE',  ( -1.000000000000000000, 0.000000000000000000, 0.000000000000000000 ) ) ;
#3376 = VERTEX_POINT ( 'NONE', #22208 ) ;
#3377 = CARTESIAN_POINT ( 'NONE',  ( 0.000000000000000000, 24.73286445877703699, 73.44644590900068692 ) ) ;
#3378 = CIRCLE ( 'NONE', #47929, 37.49900000000000944 ) ;
#3379 = VECTOR ( 'NONE', #5315, 1000.000000000000000 ) ;
#3380 = AXIS2_PLACEMENT_3D ( 'NONE', #18742, #22187, #15091 ) ;
#3381 = DIRECTION ( 'NONE',  ( 0.000000000000000000, -0.8910065241883722287, 0.4539904997395382558 ) ) ;
#3382 = CARTESIAN_POINT ( 'NONE',  ( 10.00000000000000000, -0.8828120875898013420, -37.48860685352291711 ) ) ;
#3383 = VECTOR ( 'NONE', #654, 1000.000000000000000 ) ;
#3384 = ORIENTED_EDGE ( 'NONE', *, *, #1786, .T. ) ;
#3385 = ORIENTED_EDGE ( 'NONE', *, *, #1957, .T. ) ;
#3386 = DIRECTION ( 'NONE',  ( -1.000000000000000000, -0.000000000000000000, -0.000000000000000000 ) ) ;
#3387 = DIRECTION ( 'NONE',  ( 0.1276937514489694392, 0.9918136447140102341, -0.000000000000000000 ) ) ;
#3388 = AXIS2_PLACEMENT_3D ( 'NONE', #25148, #6094, #28345 ) ;
#3389 = VECTOR ( 'NONE', #25566, 1000.000000000000000 ) ;
#3390 = ORIENTED_EDGE ( 'NONE', *, *, #38914, .F. ) ;
#3391 = ORIENTED_EDGE ( 'NONE', *, *, #3068, .T. ) ;
#3392 = AXIS2_PLACEMENT_3D ( 'NONE', #8353, #42368, #12040 ) ;
#3393 = DIRECTION ( 'NONE',  ( -1.000000000000000000, -0.000000000000000000, 0.000000000000000000 ) ) ;
#3394 = DIRECTION ( 'NONE',  ( 9.814797785686868941E-17, -1.000000000000000000, 0.000000000000000000 ) ) ;
#3395 = EDGE_LOOP ( 'NONE', ( #47926, #405, #25717, #36183 ) ) ;
#3396 = CIRCLE ( 'NONE', #16739, 31.99999999999998224 ) ;
#3397 = CARTESIAN_POINT ( 'NONE',  ( 10.00000000000000000, -12.42422080174614862, -35.38097989696524337 ) ) ;
#3398 = CARTESIAN_POINT ( 'NONE',  ( 10.00000000000000000, 41.91543099594818500, 2.663952781846293139 ) ) ;
#3399 = FACE_OUTER_BOUND ( 'NONE', #29085, .T. ) ;
#3400 = CARTESIAN_POINT ( 'NONE',  ( -235.0000123116479926, -117.0000000000000142, 2.500000000000000000 ) ) ;
#3401 = DIRECTION ( 'NONE',  ( 1.000000000000000000, 0.000000000000000000, 0.000000000000000000 ) ) ;
#3402 = AXIS2_PLACEMENT_3D ( 'NONE', #24334, #39266, #17215 ) ;
#3403 = CYLINDRICAL_SURFACE ( 'NONE', #16972, 82.00000000000000000 ) ;
#3404 = ADVANCED_FACE ( 'NONE', ( #25388 ), #25144, .T. ) ;
#3405 = PLANE ( 'NONE',  #499 ) ;
#3406 = CARTESIAN_POINT ( 'NONE',  ( 5.000000000000002665, 81.34940948281351325, -10.30890764327296161 ) ) ;
#3407 = VERTEX_POINT ( 'NONE', #25628 ) ;
#3408 = EDGE_CURVE ( 'NONE', #23027, #26795, #38842, .T. ) ;
#3409 = DIRECTION ( 'NONE',  ( -1.000000000000000000, 0.000000000000000000, -0.000000000000000000 ) ) ;
#3410 = DIRECTION ( 'NONE',  ( 1.000000000000000000, 0.000000000000000000, -0.000000000000000000 ) ) ;
#3411 = ADVANCED_FACE ( 'NONE', ( #36645 ), #43753, .T. ) ;
#3412 =( NAMED_UNIT ( * ) SI_UNIT ( $, .STERADIAN. ) SOLID_ANGLE_UNIT ( ) );
#3413 = LINE ( 'NONE', #36474, #3701 ) ;
#3414 = ORIENTED_EDGE ( 'NONE', *, *, #35958, .T. ) ;
#3415 = ORIENTED_EDGE ( 'NONE', *, *, #42497, .F. ) ;
#3416 = CIRCLE ( 'NONE', #47209, 77.49899999999999523 ) ;
#3417 = ORIENTED_EDGE ( 'NONE', *, *, #269, .T. ) ;
#3418 = AXIS2_PLACEMENT_3D ( 'NONE', #11059, #2742, #28924 ) ;
#3419 = LINE ( 'NONE', #11019, #36189 ) ;
#3420 = ADVANCED_FACE ( 'NONE', ( #21485 ), #7027, .T. ) ;
#3421 = CIRCLE ( 'NONE', #5007, 42.00000000000000000 ) ;
#3422 = AXIS2_PLACEMENT_3D ( 'NONE', #6786, #21212, #13890 ) ;
#3423 = CIRCLE ( 'NONE', #13608, 31.99999999999999645 ) ;
#3424 = EDGE_CURVE ( 'NONE', #39585, #16941, #37380, .T. ) ;
#3425 = CARTESIAN_POINT ( 'NONE',  ( 6.000000000000000000, 81.50828551894227303, 8.966570791700986476 ) ) ;
#3426 = ORIENTED_EDGE ( 'NONE', *, *, #13173, .F. ) ;
#3427 = AXIS2_PLACEMENT_3D ( 'NONE', #44484, #6807, #29555 ) ;
#3428 = CIRCLE ( 'NONE', #23782, 31.99999999999999289 ) ;
#3429 = AXIS2_PLACEMENT_3D ( 'NONE', #211, #44529, #15170 ) ;
#3430 = DIRECTION ( 'NONE',  ( -1.000000000000000000, 0.000000000000000000, 0.000000000000000000 ) ) ;
#3431 = AXIS2_PLACEMENT_3D ( 'NONE', #11937, #3864, #38123 ) ;
#3432 = ORIENTED_EDGE ( 'NONE', *, *, #11070, .T. ) ;
#3433 = DIRECTION ( 'NONE',  ( 0.000000000000000000, 0.7071067811865439090, 0.7071067811865512365 ) ) ;
#3434 = ORIENTED_EDGE ( 'NONE', *, *, #30667, .F. ) ;
#3435 = EDGE_CURVE ( 'NONE', #15783, #22095, #2879, .T. ) ;
#3436 = ORIENTED_EDGE ( 'NONE', *, *, #21804, .T. ) ;
#3437 = EDGE_LOOP ( 'NONE', ( #15915, #27323, #27063, #33416 ) ) ;
#3438 = ORIENTED_EDGE ( 'NONE', *, *, #41015, .F. ) ;
#3439 = CARTESIAN_POINT ( 'NONE',  ( 0.000000000000000000, -15.33399622253540961, 80.55351364060584274 ) ) ;
#3440 = AXIS2_PLACEMENT_3D ( 'NONE', #11817, #26748, #7431 ) ;
#3441 = DIRECTION ( 'NONE',  ( 1.000000000000000000, 0.000000000000000000, 0.000000000000000000 ) ) ;
#3442 = ORIENTED_EDGE ( 'NONE', *, *, #48177, .F. ) ;
#3443 = ORIENTED_EDGE ( 'NONE', *, *, #497, .T. ) ;
#3444 = ORIENTED_EDGE ( 'NONE', *, *, #17635, .T. ) ;
#3445 = CARTESIAN_POINT ( 'NONE',  ( 0.000000000000000000, 12.26510123303259725, 35.53030884539089840 ) ) ;
#3446 = ORIENTED_EDGE ( 'NONE', *, *, #17332, .F. ) ;
#3447 = CARTESIAN_POINT ( 'NONE',  ( 15.00000000000000000, -22.67460108101774452, 6.353146135318220367 ) ) ;
#3448 = DIRECTION ( 'NONE',  ( 1.000000000000000000, -0.000000000000000000, -0.000000000000000000 ) ) ;
#3449 = ORIENTED_EDGE ( 'NONE', *, *, #10331, .T. ) ;
#3450 = DIRECTION ( 'NONE',  ( 0.000000000000000000, 0.9723699203976756689, 0.2334453638559094157 ) ) ;
#3451 = FACE_OUTER_BOUND ( 'NONE', #39530, .T. ) ;
#3452 = ORIENTED_EDGE ( 'NONE', *, *, #11934, .T. ) ;
#3453 = CARTESIAN_POINT ( 'NONE',  ( 11.99999999999999822, -51.29473840253269401, 63.97538442413408433 ) ) ;
#3454 = CIRCLE ( 'NONE', #21457, 42.00000000000000000 ) ;
#3455 = EDGE_CURVE ( 'NONE', #18078, #12619, #35713, .T. ) ;
#3456 = FACE_OUTER_BOUND ( 'NONE', #6651, .T. ) ;
#3457 = ORIENTED_EDGE ( 'NONE', *, *, #18170, .F. ) ;
#3458 = LINE ( 'NONE', #21592, #35763 ) ;
#3459 = VERTEX_POINT ( 'NONE', #14636 ) ;
#3460 = ORIENTED_EDGE ( 'NONE', *, *, #12945, .T. ) ;
#3461 = CYLINDRICAL_SURFACE ( 'NONE', #4107, 82.00000000000000000 ) ;
#3462 = CARTESIAN_POINT ( 'NONE',  ( -10.00000000000000000, 0.000000000000000000, 0.000000000000000000 ) ) ;
#3463 = VERTEX_POINT ( 'NONE', #29551 ) ;
#3464 = CIRCLE ( 'NONE', #1951, 16.00000000000000355 ) ;
#3465 = EDGE_CURVE ( 'NONE', #39693, #12539, #43541, .T. ) ;
#3466 = CARTESIAN_POINT ( 'NONE',  ( 11.99999999999999822, 67.80270845531889279, 46.11716303203210288 ) ) ;
#3467 = DIRECTION ( 'NONE',  ( -1.000000000000000000, -0.000000000000000000, 0.000000000000000000 ) ) ;
#3468 = FACE_OUTER_BOUND ( 'NONE', #36043, .T. ) ;
#3469 = ORIENTED_EDGE ( 'NONE', *, *, #10515, .T. ) ;
#3470 = AXIS2_PLACEMENT_3D ( 'NONE', #41447, #7905, #22839 ) ;
#3471 = PRODUCT_DEFINITION_SHAPE ( 'NONE', 'NONE',  #48460 ) ;
#3472 = EDGE_CURVE ( 'NONE', #9793, #9902, #44971, .T. ) ;
#3473 = CYLINDRICAL_SURFACE ( 'NONE', #10909, 77.49899999999999523 ) ;
#3474 = DIRECTION ( 'NONE',  ( -1.000000000000000000, 0.000000000000000000, 0.000000000000000000 ) ) ;
#3475 = CARTESIAN_POINT ( 'NONE',  ( 6.000000000000000000, 81.90746397400387480, 3.894527615418180044 ) ) ;
#3476 = ORIENTED_EDGE ( 'NONE', *, *, #20730, .F. ) ;
#3477 = VECTOR ( 'NONE', #46918, 1000.000000000000000 ) ;
#3478 = CIRCLE ( 'NONE', #21434, 31.99999999999998579 ) ;
#3479 = CARTESIAN_POINT ( 'NONE',  ( 0.000000000000000000, 20.85821328998756385, -10.92862929874494959 ) ) ;
#3480 = CARTESIAN_POINT ( 'NONE',  ( 23.11608002360578240, -124.4885236261218182, 2.500000000000000000 ) ) ;
#3481 = DIRECTION ( 'NONE',  ( 1.000000000000000000, 0.000000000000000000, -0.000000000000000000 ) ) ;
#3483 = AXIS2_PLACEMENT_3D ( 'NONE', #39367, #6551, #5847 ) ;
#3482 = DIRECTION ( 'NONE',  ( 0.000000000000000000, 0.9238795325112877377, -0.3826834323650873948 ) ) ;
#3484 = AXIS2_PLACEMENT_3D ( 'NONE', #30533, #45453, #7545 ) ;
#3485 = CARTESIAN_POINT ( 'NONE',  ( -3.000000000000002665, 0.000000000000000000, 0.000000000000000000 ) ) ;
#3486 = DIRECTION ( 'NONE',  ( -1.000000000000000000, 0.000000000000000000, -0.000000000000000000 ) ) ;
#3487 = DIRECTION ( 'NONE',  ( 0.000000000000000000, 0.000000000000000000, 1.000000000000000000 ) ) ;
#3488 = EDGE_CURVE ( 'NONE', #27073, #16066, #23196, .T. ) ;
#3489 = CARTESIAN_POINT ( 'NONE',  ( -8.637688417678527131, 13.69818742750669394, 42.00000000000001421 ) ) ;
#3490 = CIRCLE ( 'NONE', #7364, 42.00000000000000000 ) ;
#3491 = EDGE_CURVE ( 'NONE', #40723, #15200, #25530, .T. ) ;
#3492 = ORIENTED_EDGE ( 'NONE', *, *, #15630, .F. ) ;
#3493 = ADVANCED_FACE ( 'NONE', ( #30288 ), #1135, .F. ) ;
#3494 = ORIENTED_EDGE ( 'NONE', *, *, #25032, .F. ) ;
#3495 = CYLINDRICAL_SURFACE ( 'NONE', #12083, 82.00000000000000000 ) ;
#3496 = VERTEX_POINT ( 'NONE', #23646 ) ;
#3497 = CARTESIAN_POINT ( 'NONE',  ( 10.00000000000000000, 72.35160999960817207, 20.41045688087850607 ) ) ;
#3498 = DIRECTION ( 'NONE',  ( 0.9634709561335031980, -0.2678128389140318477, 0.000000000000000000 ) ) ;
#3499 = DIRECTION ( 'NONE',  ( -0.000000000000000000, -0.000000000000000000, -1.000000000000000000 ) ) ;
#3500 = ORIENTED_EDGE ( 'NONE', *, *, #6790, .F. ) ;
#3501 = EDGE_CURVE ( 'NONE', #24269, #29100, #163, .T. ) ;
#3502 = AXIS2_PLACEMENT_3D ( 'NONE', #30094, #30566, #38157 ) ;
#3503 = DIRECTION ( 'NONE',  ( 0.000000000000000000, 0.000000000000000000, 1.000000000000000000 ) ) ;
#3504 = EDGE_LOOP ( 'NONE', ( #5725, #7666, #12034, #15312 ) ) ;
#3505 = VECTOR ( 'NONE', #28967, 1000.000000000000000 ) ;
#3506 = CARTESIAN_POINT ( 'NONE',  ( 11.99999999999999822, -65.59268652807183742, -36.72794159290312166 ) ) ;
#3507 = LINE ( 'NONE', #37284, #15629 ) ;
#3508 = DIRECTION ( 'NONE',  ( -1.000000000000000000, -0.000000000000000000, 0.000000000000000000 ) ) ;
#3509 = ORIENTED_EDGE ( 'NONE', *, *, #2215, .T. ) ;
#3510 = CYLINDRICAL_SURFACE ( 'NONE', #21544, 31.99999999999998579 ) ;
#3511 = CIRCLE ( 'NONE', #5102, 77.49899999999999523 ) ;
#3512 = EDGE_LOOP ( 'NONE', ( #29808, #38762, #16961, #15142 ) ) ;
#3513 = CIRCLE ( 'NONE', #5876, 31.99999999999999289 ) ;
#3514 = CARTESIAN_POINT ( 'NONE',  ( -0.8815729230226008184, -93.47222532549339746, -5.500000000000000000 ) ) ;
#3515 = DIRECTION ( 'NONE',  ( 1.000000000000000000, 0.000000000000000000, 0.000000000000000000 ) ) ;
#3516 = DIRECTION ( 'NONE',  ( 0.000000000000000000, -0.8910065241883723397, 0.4539904997395382003 ) ) ;
#3517 = DIRECTION ( 'NONE',  ( 0.000000000000000000, 0.8090169943749486725, -0.5877852522924714718 ) ) ;
#3518 = EDGE_CURVE ( 'NONE', #46278, #12381, #42027, .T. ) ;
#3519 = ORIENTED_EDGE ( 'NONE', *, *, #37903, .T. ) ;
#3520 = CARTESIAN_POINT ( 'NONE',  ( 0.000000000000000000, -2.946379043146863719, 75.11764819372146462 ) ) ;
#3521 = ORIENTED_EDGE ( 'NONE', *, *, #21613, .T. ) ;
#3522 = ORIENTED_EDGE ( 'NONE', *, *, #46589, .T. ) ;
#3523 = CARTESIAN_POINT ( 'NONE',  ( -7.572224309238338336, -145.4393675041377492, -5.500000000000000000 ) ) ;
#3524 = ADVANCED_FACE ( 'NONE', ( #11453 ), #45213, .T. ) ;
#3525 = CYLINDRICAL_SURFACE ( 'NONE', #30880, 31.99999999999998579 ) ;
#3526 = VECTOR ( 'NONE', #43810, 1000.000000000000000 ) ;
#3527 = LINE ( 'NONE', #45605, #27393 ) ;
#3528 = DIRECTION ( 'NONE',  ( 1.000000000000000000, -0.000000000000000000, -0.000000000000000000 ) ) ;
#3529 = ORIENTED_EDGE ( 'NONE', *, *, #42664, .F. ) ;
#3530 = DIRECTION ( 'NONE',  ( -1.000000000000000000, 0.000000000000000000, 0.000000000000000000 ) ) ;
#3531 = ADVANCED_FACE ( 'NONE', ( #19476 ), #41783, .T. ) ;
#3532 = DIRECTION ( 'NONE',  ( -0.000000000000000000, -0.000000000000000000, -1.000000000000000000 ) ) ;
#3533 = LINE ( 'NONE', #18465, #6307 ) ;
#3534 = CARTESIAN_POINT ( 'NONE',  ( 0.000000000000000000, 12.26510123303308752, -35.53030884539072787 ) ) ;
#3535 = AXIS2_PLACEMENT_3D ( 'NONE', #5714, #46603, #28000 ) ;
#3536 = CARTESIAN_POINT ( 'NONE',  ( 0.000000000000000000, -72.35160999960801576, -20.41045688087902121 ) ) ;
#3537 = DIRECTION ( 'NONE',  ( -1.000000000000000000, -0.000000000000000000, 0.000000000000000000 ) ) ;
#3538 = LINE ( 'NONE', #45617, #37266 ) ;
#3539 = CARTESIAN_POINT ( 'NONE',  ( 10.00000000000000000, 17.28742895386084655, 75.54627589209950145 ) ) ;
#3540 = VECTOR ( 'NONE', #44889, 1000.000000000000000 ) ;
#3541 = DIRECTION ( 'NONE',  ( -1.000000000000000000, -0.000000000000000000, 0.000000000000000000 ) ) ;
#3542 = DIRECTION ( 'NONE',  ( 1.000000000000000000, -0.000000000000000000, -0.000000000000000000 ) ) ;
#3543 = EDGE_CURVE ( 'NONE', #13144, #12926, #31045, .T. ) ;
#3544 = ADVANCED_FACE ( 'NONE', ( #34405 ), #656, .F. ) ;
#3545 = CARTESIAN_POINT ( 'NONE',  ( 10.00000000000000000, -15.33399622253424965, -80.55351364060605590 ) ) ;
#3546 = VECTOR ( 'NONE', #13274, 1000.000000000000000 ) ;
#3547 = CYLINDRICAL_SURFACE ( 'NONE', #33369, 13.90444123027096879 ) ;
#3548 = DIRECTION ( 'NONE',  ( -0.9580045777625459946, -0.2867529058022011412, 0.000000000000000000 ) ) ;
#3549 = DIRECTION ( 'NONE',  ( 0.000000000000000000, 0.000000000000000000, 1.000000000000000000 ) ) ;
#3550 = DIRECTION ( 'NONE',  ( -1.000000000000000000, 0.000000000000000000, 0.000000000000000000 ) ) ;
#3551 = CIRCLE ( 'NONE', #27824, 37.49900000000000233 ) ;
#3552 = CARTESIAN_POINT ( 'NONE',  ( 0.000000000000000000, 34.94270380257639630, 74.18225833017899618 ) ) ;
#3553 = AXIS2_PLACEMENT_3D ( 'NONE', #27076, #5036, #19953 ) ;
#3554 = AXIS2_PLACEMENT_3D ( 'NONE', #29583, #36446, #33492 ) ;
#3555 = EDGE_LOOP ( 'NONE', ( #34376, #7559, #10795, #28368 ) ) ;
#3556 = ORIENTED_EDGE ( 'NONE', *, *, #22753, .F. ) ;
#3557 = EDGE_CURVE ( 'NONE', #22223, #24540, #34130, .T. ) ;
#3558 = VECTOR ( 'NONE', #39500, 1000.000000000000000 ) ;
#3559 = VERTEX_POINT ( 'NONE', #30516 ) ;
#3560 = VECTOR ( 'NONE', #13337, 1000.000000000000000 ) ;
#3561 = CARTESIAN_POINT ( 'NONE',  ( 10.00000000000000000, 51.02545421589324803, 55.20638768913779870 ) ) ;
#3562 = ORIENTED_EDGE ( 'NONE', *, *, #2909, .T. ) ;
#3563 = AXIS2_PLACEMENT_3D ( 'NONE', #13013, #28164, #5414 ) ;
#3564 = DIRECTION ( 'NONE',  ( -0.2867529058022035837, 0.9580045777625452175, 0.000000000000000000 ) ) ;
#3565 = DIRECTION ( 'NONE',  ( 0.000000000000000000, 0.2079116908177555123, -0.9781476007338064660 ) ) ;
#3566 = DIRECTION ( 'NONE',  ( 1.000000000000000000, 0.000000000000000000, 0.000000000000000000 ) ) ;
#3567 = ORIENTED_EDGE ( 'NONE', *, *, #16872, .F. ) ;
#3568 = DIRECTION ( 'NONE',  ( 1.000000000000000000, -0.000000000000000000, -0.000000000000000000 ) ) ;
#3569 = ORIENTED_EDGE ( 'NONE', *, *, #43344, .F. ) ;
#3570 = EDGE_LOOP ( 'NONE', ( #17424, #665, #3936, #21252 ) ) ;
#3571 = VERTEX_POINT ( 'NONE', #45688 ) ;
#3572 = MANIFOLD_SOLID_BREP ( 'Boss-Extrude1', #23125 ) ;
#3573 = DIRECTION ( 'NONE',  ( 0.000000000000000000, 0.000000000000000000, 1.000000000000000000 ) ) ;
#3574 = DIRECTION ( 'NONE',  ( -1.000000000000000000, 0.000000000000000000, 0.000000000000000000 ) ) ;
#3575 = CARTESIAN_POINT ( 'NONE',  ( 15.00000000000000000, 8.688484142254226938, 21.88630264137359305 ) ) ;
#3576 = AXIS2_PLACEMENT_3D ( 'NONE', #28628, #1970, #17343 ) ;
#3577 = VERTEX_POINT ( 'NONE', #418 ) ;
#3578 = ORIENTED_EDGE ( 'NONE', *, *, #33962, .T. ) ;
#3579 = CARTESIAN_POINT ( 'NONE',  ( -9.937067298023311679, 7.583184918921313411, 125.0000000000000000 ) ) ;
#3580 = ORIENTED_EDGE ( 'NONE', *, *, #2827, .F. ) ;
#3581 = CARTESIAN_POINT ( 'NONE',  ( 35.50000000000000711, -120.0000000000000000, -2.500000000000000000 ) ) ;
#3582 = EDGE_CURVE ( 'NONE', #15492, #39405, #39644, .T. ) ;
#3583 = CIRCLE ( 'NONE', #30968, 82.00000000000000000 ) ;
#3584 = CARTESIAN_POINT ( 'NONE',  ( 10.00000000000000000, -27.05870788708213226, -26.08949754953053102 ) ) ;
#3585 = LINE ( 'NONE', #18517, #30731 ) ;
#3586 = CYLINDRICAL_SURFACE ( 'NONE', #8117, 31.99999999999998579 ) ;
#3587 = CARTESIAN_POINT ( 'NONE',  ( 0.000000000000000000, 8.966570791700705811, 81.50828551894228724 ) ) ;
#3588 = EDGE_CURVE ( 'NONE', #21447, #15966, #2112, .T. ) ;
#3589 = DIRECTION ( 'NONE',  ( -1.000000000000000000, 0.000000000000000000, 0.000000000000000000 ) ) ;
#3590 = CARTESIAN_POINT ( 'NONE',  ( 0.000000000000000000, -16.23288003029473359, -33.80338159004301701 ) ) ;
#3591 = LINE ( 'NONE', #30278, #34716 ) ;
#3592 = EDGE_LOOP ( 'NONE', ( #31845, #9182, #38858, #40891 ) ) ;
#3593 = DIRECTION ( 'NONE',  ( 1.000000000000000000, 0.000000000000000000, -0.000000000000000000 ) ) ;
#3594 = ORIENTED_EDGE ( 'NONE', *, *, #15647, .F. ) ;
#3595 = CIRCLE ( 'NONE', #30973, 82.00000000000000000 ) ;
#3596 = EDGE_CURVE ( 'NONE', #23277, #27199, #20948, .T. ) ;
#3597 = CARTESIAN_POINT ( 'NONE',  ( -10.00000000000000000, 0.000000000000000000, 0.000000000000000000 ) ) ;
#3598 = DIRECTION ( 'NONE',  ( 0.000000000000000000, 0.07845909572784530439, -0.9969173337331279638 ) ) ;
#3599 = CIRCLE ( 'NONE', #26281, 31.99999999999998934 ) ;
#3600 = CARTESIAN_POINT ( 'NONE',  ( 6.000000000000000000, -22.90783923731575200, -78.73519480814978522 ) ) ;
#3601 = DIRECTION ( 'NONE',  ( 1.000000000000000000, 0.000000000000000000, 0.000000000000000000 ) ) ;
#3602 = AXIS2_PLACEMENT_3D ( 'NONE', #20362, #20135, #9355 ) ;
#3603 = EDGE_CURVE ( 'NONE', #45052, #28496, #38059, .T. ) ;
#3604 = DIRECTION ( 'NONE',  ( -1.000000000000000000, -0.000000000000000000, 0.000000000000000000 ) ) ;
#3605 = DIRECTION ( 'NONE',  ( -1.000000000000000000, 0.000000000000000000, -0.000000000000000000 ) ) ;
#3606 = AXIS2_PLACEMENT_3D ( 'NONE', #47706, #25676, #40155 ) ;
#3607 = CYLINDRICAL_SURFACE ( 'NONE', #23983, 31.99999999999998579 ) ;
#3608 = DIRECTION ( 'NONE',  ( -1.000000000000000000, -0.000000000000000000, -0.000000000000000000 ) ) ;
#3609 = EDGE_CURVE ( 'NONE', #19346, #14976, #8354, .T. ) ;
#3610 = DIRECTION ( 'NONE',  ( -0.9827303690289285187, -0.1850432970638656860, 0.000000000000000000 ) ) ;
#3611 =( NAMED_UNIT ( * ) SI_UNIT ( $, .STERADIAN. ) SOLID_ANGLE_UNIT ( ) );
#3612 = AXIS2_PLACEMENT_3D ( 'NONE', #15358, #38105, #41532 ) ;
#3613 = CARTESIAN_POINT ( 'NONE',  ( -10.00000000000000000, 0.000000000000000000, 0.000000000000000000 ) ) ;
#3614 = VERTEX_POINT ( 'NONE', #2334 ) ;
#3615 = ORIENTED_EDGE ( 'NONE', *, *, #15695, .F. ) ;
#3616 = ADVANCED_FACE ( 'NONE', ( #20702 ), #39069, .T. ) ;
#3617 = AXIS2_PLACEMENT_3D ( 'NONE', #11481, #18317, #26403 ) ;
#3618 = EDGE_LOOP ( 'NONE', ( #40947, #27259, #40984, #24700 ) ) ;
#3619 = CIRCLE ( 'NONE', #8307, 82.00000000000000000 ) ;
#3620 = CARTESIAN_POINT ( 'NONE',  ( 11.99999999999999822, -31.47745569255092235, -68.26794271651296242 ) ) ;
#3621 = CARTESIAN_POINT ( 'NONE',  ( 0.000000000000000000, 62.50329211542494789, -41.76937507738723099 ) ) ;
#3622 = ORIENTED_EDGE ( 'NONE', *, *, #13594, .T. ) ;
#3623 = ORIENTED_EDGE ( 'NONE', *, *, #2418, .T. ) ;
#3624 = ADVANCED_FACE ( 'NONE', ( #35870 ), #48214, .F. ) ;
#3625 = CARTESIAN_POINT ( 'NONE',  ( 11.99999999999999822, 81.96053171279901051, -2.543863470248673764 ) ) ;
#3626 = EDGE_LOOP ( 'NONE', ( #38255, #27177, #18126, #3562 ) ) ;
#3627 = ORIENTED_EDGE ( 'NONE', *, *, #35868, .F. ) ;
#3628 = VECTOR ( 'NONE', #38463, 1000.000000000000000 ) ;
#3629 = EDGE_LOOP ( 'NONE', ( #26626, #11407, #29031, #16703 ) ) ;
#3630 = AXIS2_PLACEMENT_3D ( 'NONE', #16180, #19345, #34759 ) ;
#3631 = VECTOR ( 'NONE', #35927, 1000.000000000000000 ) ;
#3632 = CARTESIAN_POINT ( 'NONE',  ( 10.00000000000000000, 0.000000000000000000, 0.000000000000000000 ) ) ;
#3633 = EDGE_LOOP ( 'NONE', ( #28091, #37120, #25456, #4239 ) ) ;
#3634 = CYLINDRICAL_SURFACE ( 'NONE', #46567, 82.00000000000000000 ) ;
#3635 = ORIENTED_EDGE ( 'NONE', *, *, #37997, .T. ) ;
#3636 = ORIENTED_EDGE ( 'NONE', *, *, #8442, .F. ) ;
#3637 = EDGE_CURVE ( 'NONE', #6704, #16500, #20864, .T. ) ;
#3638 = LINE ( 'NONE', #916, #37687 ) ;
#3639 = ADVANCED_FACE ( 'NONE', ( #16800 ), #9204, .F. ) ;
#3640 = DIRECTION ( 'NONE',  ( -1.000000000000000000, -0.000000000000000000, -0.000000000000000000 ) ) ;
#3641 = DIRECTION ( 'NONE',  ( -1.000000000000000000, -0.000000000000000000, 0.000000000000000000 ) ) ;
#3642 = ORIENTED_EDGE ( 'NONE', *, *, #4528, .T. ) ;
#3643 = EDGE_CURVE ( 'NONE', #47876, #27745, #24775, .T. ) ;
#3644 = ORIENTED_EDGE ( 'NONE', *, *, #15798, .T. ) ;
#3645 = CARTESIAN_POINT ( 'NONE',  ( 18.80329974962065265, -105.8248132807389084, 5.500000000000000000 ) ) ;
#3646 = DIRECTION ( 'NONE',  ( -1.000000000000000000, -0.000000000000000000, -0.000000000000000000 ) ) ;
#3647 = VECTOR ( 'NONE', #14616, 1000.000000000000114 ) ;
#3648 = VERTEX_POINT ( 'NONE', #46896 ) ;
#3649 = ORIENTED_EDGE ( 'NONE', *, *, #45761, .F. ) ;
#3650 = ADVANCED_FACE ( 'NONE', ( #31751 ), #12645, .T. ) ;
#3651 = CYLINDRICAL_SURFACE ( 'NONE', #1788, 77.49899999999999523 ) ;
#3652 = LINE ( 'NONE', #18582, #13691 ) ;
#3653 = ORIENTED_EDGE ( 'NONE', *, *, #11617, .F. ) ;
#3654 = DIRECTION ( 'NONE',  ( -1.000000000000000000, -0.000000000000000000, -0.000000000000000000 ) ) ;
#3655 = DIRECTION ( 'NONE',  ( -0.5687579148473752566, 0.8225049752423786442, 0.000000000000000000 ) ) ;
#3656 = AXIS2_PLACEMENT_3D ( 'NONE', #38223, #11790, #46055 ) ;
#3657 = DIRECTION ( 'NONE',  ( 0.000000000000000000, -0.2079116908177664758, -0.9781476007338042455 ) ) ;
#3658 = DIRECTION ( 'NONE',  ( 0.000000000000000000, -0.9969173337331271867, -0.07845909572785571273 ) ) ;
#3659 = DIRECTION ( 'NONE',  ( -1.000000000000000000, 0.000000000000000000, -0.000000000000000000 ) ) ;
#3660 = DIRECTION ( 'NONE',  ( 0.000000000000000000, -0.000000000000000000, 1.000000000000000000 ) ) ;
#3661 = CARTESIAN_POINT ( 'NONE',  ( 0.000000000000000000, 30.84782396557248418, -21.32104025579081252 ) ) ;
#3662 = VECTOR ( 'NONE', #12582, 1000.000000000000000 ) ;
#3663 = CYLINDRICAL_SURFACE ( 'NONE', #38025, 77.49899999999999523 ) ;
#3664 = LINE ( 'NONE', #15176, #46557 ) ;
#3665 = DIRECTION ( 'NONE',  ( 0.000000000000000000, 0.7071067811865486830, -0.7071067811865464625 ) ) ;
#3666 = DIRECTION ( 'NONE',  ( -1.000000000000000000, -0.000000000000000000, -0.000000000000000000 ) ) ;
#3667 = DIRECTION ( 'NONE',  ( 1.000000000000000000, 0.000000000000000000, 0.000000000000000000 ) ) ;
#3668 = CARTESIAN_POINT ( 'NONE',  ( 1.459549131277868561, -120.3460004817713411, -2.500000000000000000 ) ) ;
#3669 = VERTEX_POINT ( 'NONE', #24138 ) ;
#3670 = ORIENTED_EDGE ( 'NONE', *, *, #32119, .F. ) ;
#3671 = AXIS2_PLACEMENT_3D ( 'NONE', #36112, #18222, #13363 ) ;
#3672 = EDGE_CURVE ( 'NONE', #2120, #16057, #22442, .T. ) ;
#3673 = PRODUCT_DEFINITION_CONTEXT ( 'detailed design', #5717, 'design' ) ;
#3674 = DIRECTION ( 'NONE',  ( -0.000000000000000000, -0.000000000000000000, -1.000000000000000000 ) ) ;
#3675 = LINE ( 'NONE', #18604, #18253 ) ;
#3676 = LINE ( 'NONE', #7346, #40175 ) ;
#3677 = ORIENTED_EDGE ( 'NONE', *, *, #7779, .F. ) ;
#3678 = VERTEX_POINT ( 'NONE', #13598 ) ;
#3679 = AXIS2_PLACEMENT_3D ( 'NONE', #32431, #20196, #46390 ) ;
#3680 = LINE ( 'NONE', #39932, #8492 ) ;
#3681 = ORIENTED_EDGE ( 'NONE', *, *, #7115, .F. ) ;
#3682 = ORIENTED_EDGE ( 'NONE', *, *, #44489, .T. ) ;
#3683 = VECTOR ( 'NONE', #7084, 1000.000000000000000 ) ;
#3684 = VERTEX_POINT ( 'NONE', #43220 ) ;
#3685 = ORIENTED_EDGE ( 'NONE', *, *, #42156, .F. ) ;
#3686 = VERTEX_POINT ( 'NONE', #13359 ) ;
#3687 = DIRECTION ( 'NONE',  ( 0.000000000000000000, 0.000000000000000000, 1.000000000000000000 ) ) ;
#3688 = DIRECTION ( 'NONE',  ( -1.000000000000000000, -0.000000000000000000, -0.000000000000000000 ) ) ;
#3689 = VECTOR ( 'NONE', #20571, 1000.000000000000000 ) ;
#3690 = VERTEX_POINT ( 'NONE', #9677 ) ;
#3691 = ORIENTED_EDGE ( 'NONE', *, *, #34310, .F. ) ;
#3692 = EDGE_CURVE ( 'NONE', #27936, #13603, #26353, .T. ) ;
#3693 = CYLINDRICAL_SURFACE ( 'NONE', #8717, 16.00000000000000000 ) ;
#3694 = VERTEX_POINT ( 'NONE', #9931 ) ;
#3695 = CARTESIAN_POINT ( 'NONE',  ( 0.000000000000000000, 74.74816331893430288, 33.71516098798768013 ) ) ;
#3696 = EDGE_CURVE ( 'NONE', #18977, #39357, #34908, .T. ) ;
#3697 = CARTESIAN_POINT ( 'NONE',  ( -12.49999999999999645, 0.000000000000000000, 125.0000000000000000 ) ) ;
#3698 = ORIENTED_EDGE ( 'NONE', *, *, #41058, .F. ) ;
#3699 = DIRECTION ( 'NONE',  ( -1.000000000000000000, 0.000000000000000000, 0.000000000000000000 ) ) ;
#3700 = CARTESIAN_POINT ( 'NONE',  ( 20.10151712711562766, -102.7321394148470830, -2.500000000000000000 ) ) ;
#3701 = VECTOR ( 'NONE', #44781, 1000.000000000000000 ) ;
#3703 = ORIENTED_EDGE ( 'NONE', *, *, #17024, .F. ) ;
#3702 = DIRECTION ( 'NONE',  ( 0.000000000000000000, -0.7071067811865535679, 0.7071067811865413555 ) ) ;
#3704 = CARTESIAN_POINT ( 'NONE',  ( 0.000000000000000000, 62.50884508063427347, 41.76106447765511831 ) ) ;
#3705 = ORIENTED_EDGE ( 'NONE', *, *, #12403, .F. ) ;
#3706 = DIRECTION ( 'NONE',  ( -0.8541291221503261033, 0.5200609990133016058, 0.000000000000000000 ) ) ;
#3707 = ORIENTED_EDGE ( 'NONE', *, *, #21900, .F. ) ;
#3708 = ORIENTED_EDGE ( 'NONE', *, *, #18499, .T. ) ;
#3709 = EDGE_CURVE ( 'NONE', #21714, #6290, #24016, .T. ) ;
#3710 = LINE ( 'NONE', #40202, #11931 ) ;
#3711 = DIRECTION ( 'NONE',  ( 0.000000000000000000, 0.3090169943749560555, 0.9510565162951506446 ) ) ;
#3712 = CYLINDRICAL_SURFACE ( 'NONE', #28490, 42.00000000000000000 ) ;
#3713 = EDGE_CURVE ( 'NONE', #20060, #11606, #11510, .T. ) ;
#3714 = LINE ( 'NONE', #33799, #20345 ) ;
#3715 = CARTESIAN_POINT ( 'NONE',  ( 10.00000000000000000, -34.44570377933649041, 69.42325613327427902 ) ) ;
#3716 = DIRECTION ( 'NONE',  ( -0.6575728627325955200, 0.7533909544171997208, 0.000000000000000000 ) ) ;
#3717 = CARTESIAN_POINT ( 'NONE',  ( 0.000000000000000000, 6.762365576493643893, -25.66652317338391853 ) ) ;
#3718 = DIRECTION ( 'NONE',  ( -1.000000000000000000, 0.000000000000000000, 0.000000000000000000 ) ) ;
#3719 = CIRCLE ( 'NONE', #31093, 16.00000000000000355 ) ;
#3720 = EDGE_LOOP ( 'NONE', ( #10458, #47860, #46613, #20728 ) ) ;
#3721 = FACE_OUTER_BOUND ( 'NONE', #27692, .T. ) ;
#3722 = DIRECTION ( 'NONE',  ( -1.000000000000000000, -0.000000000000000000, -0.000000000000000000 ) ) ;
#3723 = DIRECTION ( 'NONE',  ( -1.000000000000000000, -0.000000000000000000, 0.000000000000000000 ) ) ;
#3724 = CARTESIAN_POINT ( 'NONE',  ( 0.000000000000000000, 76.66974797899852945, -11.30684508768257679 ) ) ;
#3725 = ADVANCED_FACE ( 'NONE', ( #23900 ), #5302, .T. ) ;
#3726 = AXIS2_PLACEMENT_3D ( 'NONE', #37620, #1136, #15587 ) ;
#3727 = LINE ( 'NONE', #44842, #17389 ) ;
#3728 = CYLINDRICAL_SURFACE ( 'NONE', #15160, 42.00000000000000000 ) ;
#3729 = CARTESIAN_POINT ( 'NONE',  ( 10.00000000000000000, 5.256550761633969060, -77.32052557432835727 ) ) ;
#3730 = LINE ( 'NONE', #18423, #40530 ) ;
#3731 = EDGE_LOOP ( 'NONE', ( #45449, #16266, #35435, #23257 ) ) ;
#3732 = ORIENTED_EDGE ( 'NONE', *, *, #39586, .F. ) ;
#3733 = DIRECTION ( 'NONE',  ( 0.9730327541852497042, -0.2306669878475622604, 0.000000000000000000 ) ) ;
#3734 = CIRCLE ( 'NONE', #39705, 31.99999999999999289 ) ;
#3735 = ORIENTED_EDGE ( 'NONE', *, *, #17068, .T. ) ;
#3736 = LINE ( 'NONE', #18659, #2536 ) ;
#3737 = CARTESIAN_POINT ( 'NONE',  ( 0.000000000000000000, -120.0000000000000000, 40.00000000000000000 ) ) ;
#3738 = LINE ( 'NONE', #18662, #9623 ) ;
#3739 = VERTEX_POINT ( 'NONE', #36110 ) ;
#3740 = AXIS2_PLACEMENT_3D ( 'NONE', #11899, #8688, #22905 ) ;
#3741 = EDGE_CURVE ( 'NONE', #36132, #28640, #30276, .T. ) ;
#3742 = DIRECTION ( 'NONE',  ( -1.000000000000000000, 0.000000000000000000, 0.000000000000000000 ) ) ;
#3743 = VERTEX_POINT ( 'NONE', #3545 ) ;
#3744 = ADVANCED_FACE ( 'NONE', ( #6978 ), #10406, .T. ) ;
#3745 = CIRCLE ( 'NONE', #17818, 15.99999999999999645 ) ;
#3746 = CARTESIAN_POINT ( 'NONE',  ( 10.00000000000000000, -3.925862922256464493, 41.81611651403861174 ) ) ;
#3747 = CARTESIAN_POINT ( 'NONE',  ( 11.99999999999999822, 77.19088730480532945, -6.903761155836932062 ) ) ;
#3749 = VERTEX_POINT ( 'NONE', #40515 ) ;
#3748 = CARTESIAN_POINT ( 'NONE',  ( 0.000000000000000000, 75.16055320797057959, -18.89407956138179046 ) ) ;
#3750 = EDGE_LOOP ( 'NONE', ( #25235, #38923, #17432, #39153 ) ) ;
#3751 = VECTOR ( 'NONE', #46897, 1000.000000000000000 ) ;
#3752 = CARTESIAN_POINT ( 'NONE',  ( 10.00000000000000000, -35.53030884539094103, 12.26510123303246935 ) ) ;
#3753 = EDGE_CURVE ( 'NONE', #42541, #956, #43481, .T. ) ;
#3754 = VECTOR ( 'NONE', #38869, 1000.000000000000114 ) ;
#3755 = EDGE_CURVE ( 'NONE', #33968, #47670, #22142, .T. ) ;
#3756 = EDGE_CURVE ( 'NONE', #30305, #25221, #19984, .T. ) ;
#3757 = FACE_OUTER_BOUND ( 'NONE', #3958, .T. ) ;
#3758 = CARTESIAN_POINT ( 'NONE',  ( 0.000000000000000000, 0.000000000000000000, 0.000000000000000000 ) ) ;
#3759 = FACE_OUTER_BOUND ( 'NONE', #29095, .T. ) ;
#3760 = CARTESIAN_POINT ( 'NONE',  ( 10.00000000000000000, 37.22597642581150268, 5.202137450157037435 ) ) ;
#3761 = ORIENTED_EDGE ( 'NONE', *, *, #19163, .T. ) ;
#3762 = CARTESIAN_POINT ( 'NONE',  ( 11.99999999999999822, 77.32052557432849937, -5.256550761632002633 ) ) ;
#3763 = ORIENTED_EDGE ( 'NONE', *, *, #35214, .T. ) ;
#3764 = VERTEX_POINT ( 'NONE', #21894 ) ;
#3765 = DIRECTION ( 'NONE',  ( -1.000000000000000000, -0.000000000000000000, 0.000000000000000000 ) ) ;
#3766 = DIRECTION ( 'NONE',  ( 0.000000000000000000, 0.000000000000000000, -1.000000000000000000 ) ) ;
#3767 = EDGE_CURVE ( 'NONE', #16750, #16956, #36822, .T. ) ;
#3768 = CARTESIAN_POINT ( 'NONE',  ( 10.00000000000000000, 35.38097989696528600, -12.42422080174602605 ) ) ;
#3769 = CYLINDRICAL_SURFACE ( 'NONE', #47683, 12.50000000000000000 ) ;
#3770 = ORIENTED_EDGE ( 'NONE', *, *, #22635, .T. ) ;
#3772 = CARTESIAN_POINT ( 'NONE',  ( -10.00000000000000000, 0.000000000000000000, 0.000000000000000000 ) ) ;
#3771 = PRESENTATION_LAYER_ASSIGNMENT (  '', '', ( #2997 ) ) ;
#3773 = DIRECTION ( 'NONE',  ( -1.000000000000000000, -0.000000000000000000, 0.000000000000000000 ) ) ;
#3774 = DIRECTION ( 'NONE',  ( 0.000000000000000000, 0.9876883405951372152, 0.1564344650402346160 ) ) ;
#3775 = CARTESIAN_POINT ( 'NONE',  ( 10.00000000000000000, 37.22597642581158084, 10.79786254984347593 ) ) ;
#3776 = CARTESIAN_POINT ( 'NONE',  ( 0.000000000000000000, -66.50666863321971789, -39.78640506895676054 ) ) ;
#3777 = CARTESIAN_POINT ( 'NONE',  ( 0.000000000000000000, 41.76937507738788469, 62.50329211542452157 ) ) ;
#3778 = ORIENTED_EDGE ( 'NONE', *, *, #29950, .T. ) ;
#3779 = LINE ( 'NONE', #4029, #42763 ) ;
#3780 = CARTESIAN_POINT ( 'NONE',  ( 0.000000000000000000, -26.08949754953005495, -27.05870788708258701 ) ) ;
#3781 = CARTESIAN_POINT ( 'NONE',  ( 11.99999999999999822, -59.03961581697432592, 46.53671651293927880 ) ) ;
#3782 = FACE_OUTER_BOUND ( 'NONE', #7092, .T. ) ;
#3783 = LINE ( 'NONE', #30700, #28598 ) ;
#3784 = EDGE_LOOP ( 'NONE', ( #45526, #13775, #39141, #11597 ) ) ;
#3785 = FACE_OUTER_BOUND ( 'NONE', #20250, .T. ) ;
#3786 = DIRECTION ( 'NONE',  ( 0.000000000000000000, 0.000000000000000000, -1.000000000000000000 ) ) ;
#3787 = CARTESIAN_POINT ( 'NONE',  ( 11.99999999999999822, 0.000000000000000000, 0.000000000000000000 ) ) ;
#3788 = DIRECTION ( 'NONE',  ( -1.000000000000000000, -0.000000000000000000, 0.000000000000000000 ) ) ;
#3789 = AXIS2_PLACEMENT_3D ( 'NONE', #23684, #38636, #39105 ) ;
#3790 = VECTOR ( 'NONE', #48382, 999.9999999999998863 ) ;
#3791 = AXIS2_PLACEMENT_3D ( 'NONE', #22427, #37103, #27069 ) ;
#3792 = CARTESIAN_POINT ( 'NONE',  ( 10.00000000000000000, 73.95703589264006439, -23.16143007188350822 ) ) ;
#3793 = ORIENTED_EDGE ( 'NONE', *, *, #40289, .T. ) ;
#3794 = ORIENTED_EDGE ( 'NONE', *, *, #25279, .T. ) ;
#3795 = EDGE_CURVE ( 'NONE', #9001, #40828, #14322, .T. ) ;
#3796 = EDGE_CURVE ( 'NONE', #23423, #11302, #25805, .T. ) ;
#3797 = ORIENTED_EDGE ( 'NONE', *, *, #14332, .T. ) ;
#3798 = EDGE_CURVE ( 'NONE', #15671, #8125, #28623, .T. ) ;
#3799 = EDGE_LOOP ( 'NONE', ( #1084, #12084, #25830, #4015 ) ) ;
#3800 = CARTESIAN_POINT ( 'NONE',  ( 10.00000000000000000, 62.50884508063487033, -41.76106447765422303 ) ) ;
#3801 = CARTESIAN_POINT ( 'NONE',  ( 11.99999999999999822, 46.21855187248719687, -62.20884554313968806 ) ) ;
#3802 = ORIENTED_EDGE ( 'NONE', *, *, #27807, .T. ) ;
#3803 = ORIENTED_EDGE ( 'NONE', *, *, #1610, .F. ) ;
#3804 = EDGE_CURVE ( 'NONE', #37452, #25110, #29000, .T. ) ;
#3805 = AXIS2_PLACEMENT_3D ( 'NONE', #31386, #47016, #13481 ) ;
#3806 = CARTESIAN_POINT ( 'NONE',  ( 10.00000000000000000, 55.19960302592066625, 51.03279382321107249 ) ) ;
#3807 = CARTESIAN_POINT ( 'NONE',  ( -3.000000000000002665, 0.000000000000000000, -19.21700905503013601 ) ) ;
#3809 = EDGE_LOOP ( 'NONE', ( #4105, #5843, #7603, #4696 ) ) ;
#3808 = LINE ( 'NONE', #29752, #44918 ) ;
#3810 = ORIENTED_EDGE ( 'NONE', *, *, #24211, .F. ) ;
#3811 = CARTESIAN_POINT ( 'NONE',  ( 0.000000000000000000, 33.80338159004307386, -16.23288003029461279 ) ) ;
#3812 = ORIENTED_EDGE ( 'NONE', *, *, #8759, .T. ) ;
#3813 = VERTEX_POINT ( 'NONE', #10163 ) ;
#3814 = ORIENTED_EDGE ( 'NONE', *, *, #38294, .T. ) ;
#3815 = EDGE_CURVE ( 'NONE', #18791, #43612, #32507, .T. ) ;
#3816 = ADVANCED_FACE ( 'NONE', ( #32674 ), #13854, .F. ) ;
#3817 = CARTESIAN_POINT ( 'NONE',  ( 10.00000000000000000, 0.000000000000000000, 0.000000000000000000 ) ) ;
#3818 = DIRECTION ( 'NONE',  ( -1.000000000000000000, 0.000000000000000000, 0.000000000000000000 ) ) ;
#3819 = DIRECTION ( 'NONE',  ( -1.000000000000000000, 0.000000000000000000, -0.000000000000000000 ) ) ;
#3820 = ORIENTED_EDGE ( 'NONE', *, *, #28732, .T. ) ;
#3821 = ORIENTED_EDGE ( 'NONE', *, *, #45248, .F. ) ;
#3822 = VERTEX_POINT ( 'NONE', #40036 ) ;
#3823 = CIRCLE ( 'NONE', #20278, 31.99999999999999289 ) ;
#3824 = CARTESIAN_POINT ( 'NONE',  ( 0.000000000000000000, -21.53537804866103045, 30.80686688397002371 ) ) ;
#3825 = ORIENTED_EDGE ( 'NONE', *, *, #40768, .F. ) ;
#3826 = DIRECTION ( 'NONE',  ( -1.000000000000000000, 0.000000000000000000, 0.000000000000000000 ) ) ;
#3827 = VECTOR ( 'NONE', #36429, 999.9999999999998863 ) ;
#3828 = DIRECTION ( 'NONE',  ( 0.000000000000000000, 0.000000000000000000, 1.000000000000000000 ) ) ;
#3830 = CARTESIAN_POINT ( 'NONE',  ( 11.99999999999999822, 62.50884508063427347, 41.76106447765511831 ) ) ;
#3829 = CIRCLE ( 'NONE', #37441, 31.99999999999998934 ) ;
#3831 = DIRECTION ( 'NONE',  ( -0.2306669878475637314, -0.9730327541852493711, 0.000000000000000000 ) ) ;
#3832 = CARTESIAN_POINT ( 'NONE',  ( -3.000000000000000000, 20.85821328998756385, -10.92862929874494959 ) ) ;
#3833 = DIRECTION ( 'NONE',  ( -1.000000000000000000, 0.000000000000000000, 0.000000000000000000 ) ) ;
#3834 = AXIS2_PLACEMENT_3D ( 'NONE', #7185, #44876, #19397 ) ;
#3835 = DIRECTION ( 'NONE',  ( 0.000000000000000000, 0.3826834323650907810, -0.9238795325112864054 ) ) ;
#3836 = DIRECTION ( 'NONE',  ( 1.000000000000000000, -0.000000000000000000, 0.000000000000000000 ) ) ;
#3838 = ADVANCED_FACE ( 'NONE', ( #32453 ), #7214, .F. ) ;
#3837 = CARTESIAN_POINT ( 'NONE',  ( -3.000000000000000000, 16.83928648764945279, -16.46020748918028076 ) ) ;
#3839 = CARTESIAN_POINT ( 'NONE',  ( -12.50000000000000000, -107.5000000000000000, 40.00000000000000000 ) ) ;
#3840 = ORIENTED_EDGE ( 'NONE', *, *, #22653, .T. ) ;
#3841 = DIRECTION ( 'NONE',  ( -1.000000000000000000, -0.000000000000000000, -0.000000000000000000 ) ) ;
#3842 = CIRCLE ( 'NONE', #37449, 31.99999999999998934 ) ;
#3843 = CARTESIAN_POINT ( 'NONE',  ( 0.000000000000000000, 35.47612816024556537, -22.48208911017461631 ) ) ;
#3844 = ORIENTED_EDGE ( 'NONE', *, *, #12127, .T. ) ;
#3845 = LINE ( 'NONE', #41780, #39991 ) ;
#3846 = DIRECTION ( 'NONE',  ( 0.8225049752423776450, 0.5687579148473765889, 0.000000000000000000 ) ) ;
#3847 = DIRECTION ( 'NONE',  ( -1.000000000000000000, 0.000000000000000000, -0.000000000000000000 ) ) ;
#3848 =( GEOMETRIC_REPRESENTATION_CONTEXT ( 3 ) GLOBAL_UNCERTAINTY_ASSIGNED_CONTEXT ( ( #4164 ) ) GLOBAL_UNIT_ASSIGNED_CONTEXT ( ( #21552, #36230, #3412 ) ) REPRESENTATION_CONTEXT ( 'NONE', 'WORKASPACE' ) );
#3849 = CARTESIAN_POINT ( 'NONE',  ( 10.00000000000000000, -10.96151621346461447, -35.95386929396268272 ) ) ;
#3850 = ORIENTED_EDGE ( 'NONE', *, *, #9160, .F. ) ;
#3851 = DIRECTION ( 'NONE',  ( 1.000000000000000000, -0.000000000000000000, -0.000000000000000000 ) ) ;
#3852 = CARTESIAN_POINT ( 'NONE',  ( -3.000000000000000000, 8.688484142253939169, 21.88630264137371029 ) ) ;
#3853 = VERTEX_POINT ( 'NONE', #6497 ) ;
#3854 = CARTESIAN_POINT ( 'NONE',  ( 0.000000000000000000, 0.000000000000000000, -43.79999999999998295 ) ) ;
#3855 = SHAPE_REPRESENTATION_RELATIONSHIP ( 'NONE' , 'NONE' ,  #31260, #31571 ) ;
#3856 = CARTESIAN_POINT ( 'NONE',  ( 0.000000000000000000, 0.000000000000000000, 0.000000000000000000 ) ) ;
#3857 = ORIENTED_EDGE ( 'NONE', *, *, #34399, .F. ) ;
#3858 = VECTOR ( 'NONE', #34524, 1000.000000000000000 ) ;
#3859 = ORIENTED_EDGE ( 'NONE', *, *, #18405, .T. ) ;
#3861 = EDGE_CURVE ( 'NONE', #43300, #25765, #2050, .T. ) ;
#3860 = AXIS2_PLACEMENT_3D ( 'NONE', #2835, #3063, #17991 ) ;
#3862 = ORIENTED_EDGE ( 'NONE', *, *, #28651, .T. ) ;
#3863 = DIRECTION ( 'NONE',  ( 0.000000000000000000, 0.000000000000000000, 1.000000000000000000 ) ) ;
#3864 = DIRECTION ( 'NONE',  ( -0.000000000000000000, -0.000000000000000000, -1.000000000000000000 ) ) ;
#3865 = ORIENTED_EDGE ( 'NONE', *, *, #24921, .T. ) ;
#3866 = EDGE_CURVE ( 'NONE', #8218, #34570, #41918, .T. ) ;
#3867 = DIRECTION ( 'NONE',  ( -1.000000000000000000, 0.000000000000000000, -0.000000000000000000 ) ) ;
#3868 = ORIENTED_EDGE ( 'NONE', *, *, #9825, .T. ) ;
#3869 = ORIENTED_EDGE ( 'NONE', *, *, #17877, .F. ) ;
#3870 = EDGE_CURVE ( 'NONE', #27962, #26444, #39801, .T. ) ;
#3871 = EDGE_CURVE ( 'NONE', #42217, #21692, #3783, .T. ) ;
#3872 = DIRECTION ( 'NONE',  ( 0.6575728627325957421, -0.7533909544171993877, -1.230411769795008318E-16 ) ) ;
#3873 = CARTESIAN_POINT ( 'NONE',  ( 10.00000000000000000, -35.95386929396264009, 10.96151621346475658 ) ) ;
#3874 = CARTESIAN_POINT ( 'NONE',  ( 0.000000000000000000, 22.74946021919175720, -29.81001611430984255 ) ) ;
#3875 = ORIENTED_EDGE ( 'NONE', *, *, #44754, .F. ) ;
#3876 = LINE ( 'NONE', #45004, #30961 ) ;
#3877 = ADVANCED_FACE ( 'NONE', ( #23116 ), #22866, .T. ) ;
#3878 = ORIENTED_EDGE ( 'NONE', *, *, #9783, .T. ) ;
#3879 = ORIENTED_EDGE ( 'NONE', *, *, #40840, .F. ) ;
#3880 = DIRECTION ( 'NONE',  ( 0.000000000000000000, -0.2079116908177653100, 0.9781476007338044676 ) ) ;
#3881 = FACE_OUTER_BOUND ( 'NONE', #989, .T. ) ;
#3882 = LINE ( 'NONE', #33729, #10385 ) ;
#3883 = ORIENTED_EDGE ( 'NONE', *, *, #1054, .F. ) ;
#3884 = ORIENTED_EDGE ( 'NONE', *, *, #39018, .F. ) ;
#3885 = CARTESIAN_POINT ( 'NONE',  ( -43.60332556124591008, -133.0000000000000000, 2.500000000000002220 ) ) ;
#3886 = EDGE_CURVE ( 'NONE', #7287, #40723, #26311, .T. ) ;
#3887 = AXIS2_PLACEMENT_3D ( 'NONE', #15414, #41120, #37432 ) ;
#3888 = CARTESIAN_POINT ( 'NONE',  ( 0.000000000000000000, 0.000000000000000000, 21.00000000000000000 ) ) ;
#3889 = ORIENTED_EDGE ( 'NONE', *, *, #2570, .T. ) ;
#3890 = CIRCLE ( 'NONE', #28136, 13.71319123027096865 ) ;
#3891 = VERTEX_POINT ( 'NONE', #38052 ) ;
#3892 = CARTESIAN_POINT ( 'NONE',  ( 5.000000000000000000, 68.55367621811141987, 44.99326035066078333 ) ) ;
#3893 = VERTEX_POINT ( 'NONE', #102 ) ;
#3894 = CARTESIAN_POINT ( 'NONE',  ( 10.00000000000000000, -50.95692526931372157, 58.39081064771733054 ) ) ;
#3895 = VECTOR ( 'NONE', #22639, 1000.000000000000000 ) ;
#3896 = DIRECTION ( 'NONE',  ( 0.000000000000000000, 0.000000000000000000, 1.000000000000000000 ) ) ;
#3897 = FACE_OUTER_BOUND ( 'NONE', #25999, .T. ) ;
#3898 = DIRECTION ( 'NONE',  ( 0.000000000000000000, 0.000000000000000000, -1.000000000000000000 ) ) ;
#3899 = PLANE ( 'NONE',  #9617 ) ;
#3900 = CARTESIAN_POINT ( 'NONE',  ( 0.000000000000000000, 0.000000000000000000, 0.000000000000000000 ) ) ;
#3901 = AXIS2_PLACEMENT_3D ( 'NONE', #33212, #14624, #29539 ) ;
#3902 = CARTESIAN_POINT ( 'NONE',  ( 10.00000000000000000, 8.840884882375075193, 74.65374052328651544 ) ) ;
#3903 = CARTESIAN_POINT ( 'NONE',  ( 0.000000000000000000, 21.53537804866126137, -30.80686688396986028 ) ) ;
#3904 = AXIS2_PLACEMENT_3D ( 'NONE', #28202, #43387, #2254 ) ;
#3905 = LINE ( 'NONE', #33999, #37144 ) ;
#3906 = ORIENTED_EDGE ( 'NONE', *, *, #5531, .T. ) ;
#3907 = CARTESIAN_POINT ( 'NONE',  ( 0.000000000000000000, -36.88895765772628010, -6.736453364083947015 ) ) ;
#3908 = DIRECTION ( 'NONE',  ( -1.000000000000000000, 0.000000000000000000, 0.000000000000000000 ) ) ;
#3909 = SURFACE_SIDE_STYLE ('',( #22516 ) ) ;
#3910 = DIRECTION ( 'NONE',  ( 0.000000000000000000, 0.000000000000000000, 1.000000000000000000 ) ) ;
#3911 = ORIENTED_EDGE ( 'NONE', *, *, #8358, .F. ) ;
#3912 = EDGE_CURVE ( 'NONE', #41773, #29157, #48151, .T. ) ;
#3913 = DIRECTION ( 'NONE',  ( -1.000000000000000000, 0.000000000000000000, 0.000000000000000000 ) ) ;
#3914 = EDGE_CURVE ( 'NONE', #10647, #20850, #45624, .T. ) ;
#3915 = DIRECTION ( 'NONE',  ( 0.000000000000000000, 0.000000000000000000, 1.000000000000000000 ) ) ;
#3916 = FACE_OUTER_BOUND ( 'NONE', #19929, .T. ) ;
#3917 = EDGE_CURVE ( 'NONE', #14446, #11050, #46596, .T. ) ;
#3918 = ORIENTED_EDGE ( 'NONE', *, *, #13261, .F. ) ;
#3919 = ADVANCED_FACE ( 'NONE', ( #19422, #29973, #45154 ), #33879, .F. ) ;
#3920 = EDGE_CURVE ( 'NONE', #1286, #11028, #350, .T. ) ;
#3921 = VECTOR ( 'NONE', #22423, 1000.000000000000000 ) ;
#3922 = EDGE_CURVE ( 'NONE', #13075, #13054, #45378, .T. ) ;
#3923 = VECTOR ( 'NONE', #10626, 1000.000000000000000 ) ;
#3924 = EDGE_CURVE ( 'NONE', #10878, #23379, #41479, .T. ) ;
#3925 = DIRECTION ( 'NONE',  ( -1.000000000000000000, 0.000000000000000000, 0.000000000000000000 ) ) ;
#3926 = ORIENTED_EDGE ( 'NONE', *, *, #1332, .F. ) ;
#3927 = ORIENTED_EDGE ( 'NONE', *, *, #28049, .F. ) ;
#3928 = ORIENTED_EDGE ( 'NONE', *, *, #24030, .T. ) ;
#3929 = ORIENTED_EDGE ( 'NONE', *, *, #38470, .F. ) ;
#3930 = ORIENTED_EDGE ( 'NONE', *, *, #27422, .T. ) ;
#3931 = CARTESIAN_POINT ( 'NONE',  ( -0.7800914985199643992, -121.2811936832255100, -2.500000000000000000 ) ) ;
#3932 = AXIS2_PLACEMENT_3D ( 'NONE', #28271, #9919, #17243 ) ;
#3933 = AXIS2_PLACEMENT_3D ( 'NONE', #3273, #18204, #47818 ) ;
#3934 = CARTESIAN_POINT ( 'NONE',  ( 10.00000000000000000, 75.11764819372149304, -2.946379043146603482 ) ) ;
#3935 = AXIS2_PLACEMENT_3D ( 'NONE', #25424, #3386, #44514 ) ;
#3936 = ORIENTED_EDGE ( 'NONE', *, *, #20497, .F. ) ;
#3937 = EDGE_CURVE ( 'NONE', #32083, #37092, #22366, .T. ) ;
#3938 = EDGE_LOOP ( 'NONE', ( #18113, #44434, #30257, #31538 ) ) ;
#3939 = DIRECTION ( 'NONE',  ( -1.000000000000000000, -0.000000000000000000, -0.000000000000000000 ) ) ;
#3940 = EDGE_LOOP ( 'NONE', ( #42106, #27417, #41222, #3943 ) ) ;
#3941 = CARTESIAN_POINT ( 'NONE',  ( 10.00000000000000000, -81.90746397400386059, -3.894527615418773347 ) ) ;
#3942 = CARTESIAN_POINT ( 'NONE',  ( 2.874421927457452952, -143.3717286177755739, 5.500000000000000000 ) ) ;
#3943 = ORIENTED_EDGE ( 'NONE', *, *, #25757, .T. ) ;
#3944 = ORIENTED_EDGE ( 'NONE', *, *, #13761, .F. ) ;
#3945 = CARTESIAN_POINT ( 'NONE',  ( 10.00000000000000000, 27.74655509720669144, 77.16300072079670258 ) ) ;
#3946 = DIRECTION ( 'NONE',  ( 0.000000000000000000, -0.07845909572783053842, -0.9969173337331290741 ) ) ;
#3947 = ORIENTED_EDGE ( 'NONE', *, *, #42333, .F. ) ;
#3949 = VERTEX_POINT ( 'NONE', #827 ) ;
#3948 = DIRECTION ( 'NONE',  ( -1.000000000000000000, 0.000000000000000000, 0.000000000000000000 ) ) ;
#3950 = EDGE_CURVE ( 'NONE', #14358, #28358, #44905, .T. ) ;
#3951 = CARTESIAN_POINT ( 'NONE',  ( 10.00000000000000000, -17.80606268964563554, 33.00180498840040855 ) ) ;
#3952 = ORIENTED_EDGE ( 'NONE', *, *, #9433, .T. ) ;
#3953 = LINE ( 'NONE', #18861, #43618 ) ;
#3954 = ORIENTED_EDGE ( 'NONE', *, *, #12430, .T. ) ;
#3955 = ORIENTED_EDGE ( 'NONE', *, *, #931, .F. ) ;
#3956 = DIRECTION ( 'NONE',  ( -1.000000000000000000, 0.000000000000000000, 0.000000000000000000 ) ) ;
#3957 = DIRECTION ( 'NONE',  ( 0.000000000000000000, -0.9238795325112822976, -0.3826834323651006065 ) ) ;
#3958 = EDGE_LOOP ( 'NONE', ( #15499, #27224, #24592, #14182 ) ) ;
#3959 = DIRECTION ( 'NONE',  ( 0.000000000000000000, 0.000000000000000000, 1.000000000000000000 ) ) ;
#3960 = CARTESIAN_POINT ( 'NONE',  ( 10.00000000000000000, 73.73191006444551476, 14.66109333815590254 ) ) ;
#3961 = DIRECTION ( 'NONE',  ( -1.000000000000000000, 0.000000000000000000, 0.000000000000000000 ) ) ;
#3962 = EDGE_CURVE ( 'NONE', #29157, #24923, #4287, .T. ) ;
#3963 = DIRECTION ( 'NONE',  ( 0.000000000000000000, -0.1564344650402380854, 0.9876883405951365491 ) ) ;
#3964 = CARTESIAN_POINT ( 'NONE',  ( 11.99999999999999822, -14.66109333815513160, 73.73191006444567108 ) ) ;
#3966 = AXIS2_PLACEMENT_3D ( 'NONE', #31220, #17223, #46376 ) ;
#3965 = DIRECTION ( 'NONE',  ( 0.000000000000000000, -0.5877852522924801315, 0.8090169943749421222 ) ) ;
#3967 = EDGE_CURVE ( 'NONE', #18691, #35660, #2787, .T. ) ;
#3968 = VECTOR ( 'NONE', #23800, 1000.000000000000000 ) ;
#3969 = CARTESIAN_POINT ( 'NONE',  ( 5.000000000000000000, -26.79245525562690844, -32.34446384430000876 ) ) ;
#3970 = CARTESIAN_POINT ( 'NONE',  ( 11.99999999999999822, 36.72794159290241822, 65.59268652807223532 ) ) ;
#3971 = CARTESIAN_POINT ( 'NONE',  ( -10.00000000000000000, 0.000000000000000000, 0.000000000000000000 ) ) ;
#3972 = DIRECTION ( 'NONE',  ( 0.000000000000000000, 0.000000000000000000, 1.000000000000000000 ) ) ;
#3973 = VECTOR ( 'NONE', #35315, 1000.000000000000000 ) ;
#3974 = CIRCLE ( 'NONE', #38350, 31.99999999999999289 ) ;
#3975 = DIRECTION ( 'NONE',  ( 0.000000000000000000, 0.000000000000000000, 1.000000000000000000 ) ) ;
#3976 = DIRECTION ( 'NONE',  ( -1.000000000000000000, -0.000000000000000000, 0.000000000000000000 ) ) ;
#3977 = FACE_OUTER_BOUND ( 'NONE', #41368, .T. ) ;
#3978 = DIRECTION ( 'NONE',  ( 0.000000000000000000, 0.000000000000000000, 1.000000000000000000 ) ) ;
#3979 = AXIS2_PLACEMENT_3D ( 'NONE', #41632, #11306, #8098 ) ;
#3980 = CIRCLE ( 'NONE', #22725, 77.49900000000000944 ) ;
#3981 = ADVANCED_FACE ( 'NONE', ( #11390 ), #30463, .F. ) ;
#3982 = ORIENTED_EDGE ( 'NONE', *, *, #16423, .T. ) ;
#3983 = FACE_BOUND ( 'NONE', #33500, .T. ) ;
#3984 = VECTOR ( 'NONE', #1673, 1000.000000000000114 ) ;
#3985 = ORIENTED_EDGE ( 'NONE', *, *, #24756, .T. ) ;
#3986 = EDGE_CURVE ( 'NONE', #45638, #30137, #36412, .T. ) ;
#3987 = CARTESIAN_POINT ( 'NONE',  ( -12.40464318976454727, 10.41032311384371845, -55.00000000000000000 ) ) ;
#3988 = DIRECTION ( 'NONE',  ( 0.000000000000000000, 0.000000000000000000, 1.000000000000000000 ) ) ;
#3989 = EDGE_CURVE ( 'NONE', #37838, #23605, #39576, .T. ) ;
#3990 = CARTESIAN_POINT ( 'NONE',  ( 0.000000000000000000, 0.000000000000000000, 0.000000000000000000 ) ) ;
#3991 = ORIENTED_EDGE ( 'NONE', *, *, #41015, .T. ) ;
#3992 = EDGE_CURVE ( 'NONE', #1521, #16286, #31660, .T. ) ;
#3993 = EDGE_CURVE ( 'NONE', #21082, #44212, #18445, .T. ) ;
#3994 = CARTESIAN_POINT ( 'NONE',  ( 0.000000000000000000, -4.992566952385247170, 37.16516213103275845 ) ) ;
#3995 = ORIENTED_EDGE ( 'NONE', *, *, #3967, .T. ) ;
#3996 = CIRCLE ( 'NONE', #6338, 42.00000000000000000 ) ;
#3997 = CARTESIAN_POINT ( 'NONE',  ( 0.000000000000000000, 0.000000000000000000, 0.000000000000000000 ) ) ;
#3998 = CIRCLE ( 'NONE', #42287, 15.99999999999999467 ) ;
#3999 = LINE ( 'NONE', #19157, #32103 ) ;
#4001 = VERTEX_POINT ( 'NONE', #27012 ) ;
#4000 = CARTESIAN_POINT ( 'NONE',  ( 10.00000000000000000, 0.000000000000000000, 0.000000000000000000 ) ) ;
#4002 = AXIS2_PLACEMENT_3D ( 'NONE', #19461, #144, #4795 ) ;
#4003 = VECTOR ( 'NONE', #16395, 1000.000000000000000 ) ;
#4004 = ORIENTED_EDGE ( 'NONE', *, *, #8970, .F. ) ;
#4005 = AXIS2_PLACEMENT_3D ( 'NONE', #36683, #3387, #18330 ) ;
#4006 = DIRECTION ( 'NONE',  ( 0.000000000000000000, 0.000000000000000000, 1.000000000000000000 ) ) ;
#4007 = DIRECTION ( 'NONE',  ( -1.000000000000000000, -0.000000000000000000, 0.000000000000000000 ) ) ;
#4008 = VECTOR ( 'NONE', #23758, 1000.000000000000000 ) ;
#4009 = DIRECTION ( 'NONE',  ( -1.000000000000000000, 0.000000000000000000, 0.000000000000000000 ) ) ;
#4011 = EDGE_LOOP ( 'NONE', ( #1714, #11285, #46389, #35520 ) ) ;
#4010 = CARTESIAN_POINT ( 'NONE',  ( 0.000000000000000000, -35.92658777277502935, -10.74501242461320594 ) ) ;
#4012 = ORIENTED_EDGE ( 'NONE', *, *, #15003, .T. ) ;
#4013 = VECTOR ( 'NONE', #17791, 1000.000000000000000 ) ;
#4014 = CARTESIAN_POINT ( 'NONE',  ( 10.00000000000000000, 58.39081064771823293, -50.95692526931266286 ) ) ;
#4015 = ORIENTED_EDGE ( 'NONE', *, *, #34966, .F. ) ;
#4016 = ORIENTED_EDGE ( 'NONE', *, *, #44597, .T. ) ;
#4017 = DIRECTION ( 'NONE',  ( -1.000000000000000000, 0.000000000000000000, 0.000000000000000000 ) ) ;
#4018 = DIRECTION ( 'NONE',  ( 0.000000000000000000, 0.000000000000000000, -1.000000000000000000 ) ) ;
#4019 = LINE ( 'NONE', #26040, #1597 ) ;
#4020 = LINE ( 'NONE', #4272, #32846 ) ;
#4021 = VERTEX_POINT ( 'NONE', #27735 ) ;
#4022 = CYLINDRICAL_SURFACE ( 'NONE', #5789, 42.00000000000000000 ) ;
#4023 = DIRECTION ( 'NONE',  ( -1.000000000000000000, 0.000000000000000000, 0.000000000000000000 ) ) ;
#4024 = LINE ( 'NONE', #19186, #23518 ) ;
#4025 = CARTESIAN_POINT ( 'NONE',  ( -10.00000000000000000, 0.000000000000000000, 0.000000000000000000 ) ) ;
#4026 = DIRECTION ( 'NONE',  ( -1.000000000000000000, 0.000000000000000000, -0.000000000000000000 ) ) ;
#4027 = DIRECTION ( 'NONE',  ( -1.000000000000000000, 0.000000000000000000, -0.000000000000000000 ) ) ;
#4028 = VERTEX_POINT ( 'NONE', #27979 ) ;
#4029 = CARTESIAN_POINT ( 'NONE',  ( 5.000000000000000000, 81.96053171279902472, -2.543863470248670211 ) ) ;
#4030 = CARTESIAN_POINT ( 'NONE',  ( 11.99999999999999822, 55.19960302592141232, -51.03279382321027668 ) ) ;
#4031 = CARTESIAN_POINT ( 'NONE',  ( 10.00000000000000000, 4.992566952384984269, 37.16516213103279398 ) ) ;
#4032 = CARTESIAN_POINT ( 'NONE',  ( 10.00000000000000000, 0.000000000000000000, 0.000000000000000000 ) ) ;
#4033 = DIRECTION ( 'NONE',  ( -1.000000000000000000, -0.000000000000000000, -0.000000000000000000 ) ) ;
#4034 = VECTOR ( 'NONE', #30035, 1000.000000000000000 ) ;
#4035 = DIRECTION ( 'NONE',  ( 1.000000000000000000, 0.000000000000000000, 0.000000000000000000 ) ) ;
#4036 = CARTESIAN_POINT ( 'NONE',  ( 10.00000000000000000, 36.72794159290334903, -65.59268652807170952 ) ) ;
#4037 = CIRCLE ( 'NONE', #8702, 82.00000000000000000 ) ;
#4038 = CYLINDRICAL_SURFACE ( 'NONE', #2822, 31.99999999999999289 ) ;
#4039 = EDGE_CURVE ( 'NONE', #38706, #45887, #7485, .T. ) ;
#4040 = CARTESIAN_POINT ( 'NONE',  ( 0.000000000000000000, 75.11764819372149304, -2.946379043146603482 ) ) ;
#4041 = EDGE_CURVE ( 'NONE', #1914, #36873, #42904, .T. ) ;
#4042 = CARTESIAN_POINT ( 'NONE',  ( 5.999999999999999112, 77.16300072079660310, 27.74655509720697211 ) ) ;
#4043 = VECTOR ( 'NONE', #38835, 1000.000000000000000 ) ;
#4044 = EDGE_LOOP ( 'NONE', ( #48070, #21337, #22064, #45180, #17709, #29362 ) ) ;
#4045 = ADVANCED_FACE ( 'NONE', ( #38497 ), #34562, .F. ) ;
#4046 = EDGE_CURVE ( 'NONE', #13148, #11292, #6713, .T. ) ;
#4047 = ORIENTED_EDGE ( 'NONE', *, *, #34315, .T. ) ;
#4048 = VECTOR ( 'NONE', #18848, 1000.000000000000000 ) ;
#4049 = EDGE_CURVE ( 'NONE', #4021, #14753, #9123, .T. ) ;
#4050 = FACE_OUTER_BOUND ( 'NONE', #41755, .T. ) ;
#4051 = EDGE_LOOP ( 'NONE', ( #874, #14968, #39484, #9962 ) ) ;
#4052 = DIRECTION ( 'NONE',  ( -0.000000000000000000, -0.000000000000000000, -1.000000000000000000 ) ) ;
#4053 = DIRECTION ( 'NONE',  ( -1.000000000000000000, 0.000000000000000000, 0.000000000000000000 ) ) ;
#4054 = CARTESIAN_POINT ( 'NONE',  ( 12.00000000000000000, -14.54903810567644484, 22.19967320028775504 ) ) ;
#4055 = ADVANCED_FACE ( 'NONE', ( #35062 ), #38257, .T. ) ;
#4056 = ORIENTED_EDGE ( 'NONE', *, *, #2874, .T. ) ;
#4057 = CARTESIAN_POINT ( 'NONE',  ( 0.000000000000000000, 0.000000000000000000, 0.000000000000000000 ) ) ;
#4058 = ORIENTED_EDGE ( 'NONE', *, *, #44385, .T. ) ;
#4059 = VERTEX_POINT ( 'NONE', #24061 ) ;
#4060 = ORIENTED_EDGE ( 'NONE', *, *, #37418, .T. ) ;
#4061 = CYLINDRICAL_SURFACE ( 'NONE', #24898, 16.00000000000000000 ) ;
#4062 = CARTESIAN_POINT ( 'NONE',  ( -3.000000000000000000, -13.04903810567647682, -19.60159698893442481 ) ) ;
#4063 = AXIS2_PLACEMENT_3D ( 'NONE', #46411, #8960, #38840 ) ;
#4064 = CARTESIAN_POINT ( 'NONE',  ( 5.999999999999999112, 64.81221759200342092, 50.23322058963371006 ) ) ;
#4065 = ORIENTED_EDGE ( 'NONE', *, *, #29169, .F. ) ;
#4066 = VERTEX_POINT ( 'NONE', #23323 ) ;
#4067 = ORIENTED_EDGE ( 'NONE', *, *, #788, .F. ) ;
#4068 = CARTESIAN_POINT ( 'NONE',  ( -10.00000000000000000, 0.000000000000000000, 0.000000000000000000 ) ) ;
#4069 = EDGE_LOOP ( 'NONE', ( #11121, #19683, #17058, #33040 ) ) ;
#4070 = AXIS2_PLACEMENT_3D ( 'NONE', #35299, #42901, #1775 ) ;
#4071 = DIRECTION ( 'NONE',  ( 0.000000000000000000, 0.000000000000000000, 1.000000000000000000 ) ) ;
#4072 = PLANE ( 'NONE',  #20161 ) ;
#4073 = LINE ( 'NONE', #11659, #8849 ) ;
#4074 = DIRECTION ( 'NONE',  ( 1.000000000000000000, 0.000000000000000000, 0.000000000000000000 ) ) ;
#4075 = DIRECTION ( 'NONE',  ( -1.000000000000000000, -0.000000000000000000, 0.000000000000000000 ) ) ;
#4076 = CARTESIAN_POINT ( 'NONE',  ( -3.000000000000000000, -3.948201729842038432, -23.21447184625298021 ) ) ;
#4077 = AXIS2_PLACEMENT_3D ( 'NONE', #10397, #33627, #14071 ) ;
#4078 = CARTESIAN_POINT ( 'NONE',  ( 26.47460221209471598, -121.8961639463267090, 5.500000000000000000 ) ) ;
#4080 = EDGE_CURVE ( 'NONE', #39866, #25379, #44244, .T. ) ;
#4079 = ORIENTED_EDGE ( 'NONE', *, *, #27813, .F. ) ;
#4081 = DIRECTION ( 'NONE',  ( 1.000000000000000000, 0.000000000000000000, 0.000000000000000000 ) ) ;
#4082 = CARTESIAN_POINT ( 'NONE',  ( 10.00000000000000000, 16.23288003029497162, 33.80338159004289622 ) ) ;
#4083 = ORIENTED_EDGE ( 'NONE', *, *, #17683, .T. ) ;
#4084 = DIRECTION ( 'NONE',  ( 0.000000000000000000, -0.6494480483301903195, 0.7604059656000251577 ) ) ;
#4085 = ADVANCED_FACE ( 'NONE', ( #1541 ), #1778, .F. ) ;
#4086 = ORIENTED_EDGE ( 'NONE', *, *, #10061, .T. ) ;
#4087 = ORIENTED_EDGE ( 'NONE', *, *, #17802, .F. ) ;
#4088 = CARTESIAN_POINT ( 'NONE',  ( 11.99999999999999822, 0.000000000000000000, 0.000000000000000000 ) ) ;
#4089 = VECTOR ( 'NONE', #36909, 1000.000000000000000 ) ;
#4090 = EDGE_CURVE ( 'NONE', #17460, #6193, #35648, .T. ) ;
#4091 = CYLINDRICAL_SURFACE ( 'NONE', #33179, 31.99999999999999289 ) ;
#4092 = CARTESIAN_POINT ( 'NONE',  ( -0.1219594728601508804, -118.5049662589159567, -2.500000000000000000 ) ) ;
#4093 = CARTESIAN_POINT ( 'NONE',  ( 10.00000000000000000, -68.55367621811110723, -44.99326035066125939 ) ) ;
#4094 = EDGE_CURVE ( 'NONE', #28981, #42650, #27057, .T. ) ;
#4095 = DIRECTION ( 'NONE',  ( -0.000000000000000000, -0.000000000000000000, -1.000000000000000000 ) ) ;
#4096 = CARTESIAN_POINT ( 'NONE',  ( -23.30023580412278505, -123.4057321492263384, 5.500000000000000000 ) ) ;
#4097 = CARTESIAN_POINT ( 'NONE',  ( 0.000000000000000000, 21.60688246758585507, 79.10210256391376049 ) ) ;
#4098 = LINE ( 'NONE', #45944, #33426 ) ;
#4099 = DIRECTION ( 'NONE',  ( -1.000000000000000000, -0.000000000000000000, -0.000000000000000000 ) ) ;
#4100 = EDGE_CURVE ( 'NONE', #14333, #38548, #12556, .T. ) ;
#4101 =( LENGTH_UNIT ( ) NAMED_UNIT ( * ) SI_UNIT ( .MILLI., .METRE. ) );
#4102 = FACE_OUTER_BOUND ( 'NONE', #23591, .T. ) ;
#4103 = EDGE_CURVE ( 'NONE', #23663, #31053, #22405, .T. ) ;
#4104 = EDGE_CURVE ( 'NONE', #45931, #18858, #38019, .T. ) ;
#4105 = ORIENTED_EDGE ( 'NONE', *, *, #17498, .F. ) ;
#4106 = VECTOR ( 'NONE', #33814, 1000.000000000000000 ) ;
#4107 = AXIS2_PLACEMENT_3D ( 'NONE', #18634, #14495, #25725 ) ;
#4108 = ORIENTED_EDGE ( 'NONE', *, *, #2133, .F. ) ;
#4109 = VECTOR ( 'NONE', #28632, 1000.000000000000000 ) ;
#4110 = VERTEX_POINT ( 'NONE', #5949 ) ;
#4111 = DIRECTION ( 'NONE',  ( 0.000000000000000000, -0.000000000000000000, 1.000000000000000000 ) ) ;
#4112 = DIRECTION ( 'NONE',  ( 0.000000000000000000, 0.9238795325112878487, -0.3826834323650874503 ) ) ;
#4113 = EDGE_LOOP ( 'NONE', ( #5825, #4828, #38494, #2708 ) ) ;
#4114 = EDGE_CURVE ( 'NONE', #43888, #24385, #40368, .T. ) ;
#4115 = AXIS2_PLACEMENT_3D ( 'NONE', #23159, #868, #22910 ) ;
#4116 = DIRECTION ( 'NONE',  ( 0.000000000000000000, -0.8090169943749426773, -0.5877852522924797984 ) ) ;
#4117 = ORIENTED_EDGE ( 'NONE', *, *, #15260, .F. ) ;
#4118 = ORIENTED_EDGE ( 'NONE', *, *, #8151, .T. ) ;
#4119 = DIRECTION ( 'NONE',  ( 0.000000000000000000, 0.000000000000000000, -1.000000000000000000 ) ) ;
#4120 = DIRECTION ( 'NONE',  ( -1.000000000000000000, 0.000000000000000000, 0.000000000000000000 ) ) ;
#4121 = DIRECTION ( 'NONE',  ( -1.000000000000000000, 0.000000000000000000, 0.000000000000000000 ) ) ;
#4122 = ORIENTED_EDGE ( 'NONE', *, *, #4208, .T. ) ;
#4123 = VERTEX_POINT ( 'NONE', #6657 ) ;
#4124 = FACE_OUTER_BOUND ( 'NONE', #1301, .T. ) ;
#4125 = ORIENTED_EDGE ( 'NONE', *, *, #7115, .T. ) ;
#4126 = ORIENTED_EDGE ( 'NONE', *, *, #45711, .F. ) ;
#4127 = CARTESIAN_POINT ( 'NONE',  ( 11.99999999999999822, -5.256550761633395297, 77.32052557432841411 ) ) ;
#4128 = DIRECTION ( 'NONE',  ( 0.9827303690289279636, 0.1850432970638682395, -0.000000000000000000 ) ) ;
#4129 = VECTOR ( 'NONE', #7416, 1000.000000000000000 ) ;
#4130 = DIRECTION ( 'NONE',  ( -1.000000000000000000, -0.000000000000000000, -0.000000000000000000 ) ) ;
#4131 = ORIENTED_EDGE ( 'NONE', *, *, #15428, .T. ) ;
#4132 = ORIENTED_EDGE ( 'NONE', *, *, #18095, .F. ) ;
#4133 = AXIS2_PLACEMENT_3D ( 'NONE', #765, #46293, #42635 ) ;
#4134 = SURFACE_STYLE_FILL_AREA ( #48422 ) ;
#4135 = DIRECTION ( 'NONE',  ( -1.000000000000000000, 0.000000000000000000, 0.000000000000000000 ) ) ;
#4136 = AXIS2_PLACEMENT_3D ( 'NONE', #16901, #21042, #20312 ) ;
#4137 = EDGE_CURVE ( 'NONE', #41352, #39824, #9097, .T. ) ;
#4138 = VERTEX_POINT ( 'NONE', #10081 ) ;
#4139 = ORIENTED_EDGE ( 'NONE', *, *, #25885, .F. ) ;
#4140 = CARTESIAN_POINT ( 'NONE',  ( 18.80329974962065265, -105.8248132807389084, 5.500000000000000000 ) ) ;
#4141 = ORIENTED_EDGE ( 'NONE', *, *, #36477, .T. ) ;
#4142 = CIRCLE ( 'NONE', #18960, 77.49900000000000944 ) ;
#4143 = FACE_OUTER_BOUND ( 'NONE', #5628, .T. ) ;
#4144 = EDGE_CURVE ( 'NONE', #23375, #48194, #9888, .T. ) ;
#4145 = DIRECTION ( 'NONE',  ( -1.000000000000000000, -0.000000000000000000, -0.000000000000000000 ) ) ;
#4146 = CIRCLE ( 'NONE', #36925, 77.49900000000000944 ) ;
#4147 = DIRECTION ( 'NONE',  ( 0.000000000000000000, 0.000000000000000000, 1.000000000000000000 ) ) ;
#4148 = CARTESIAN_POINT ( 'NONE',  ( 11.99999999999999822, 44.88180994100466847, -63.18004540532978552 ) ) ;
#4149 = CARTESIAN_POINT ( 'NONE',  ( 11.99999999999999822, 27.74655509720779989, -77.16300072079630468 ) ) ;
#4150 = DIRECTION ( 'NONE',  ( 0.000000000000000000, -0.9945218953682740670, -0.1045284632676459352 ) ) ;
#4151 = EDGE_CURVE ( 'NONE', #31423, #46006, #21585, .T. ) ;
#4152 = AXIS2_PLACEMENT_3D ( 'NONE', #11253, #26178, #41119 ) ;
#4153 = DIRECTION ( 'NONE',  ( 1.000000000000000000, 0.000000000000000000, 0.000000000000000000 ) ) ;
#4154 = DIRECTION ( 'NONE',  ( -0.000000000000000000, 0.9781476007338067991, 0.2079116908177533474 ) ) ;
#4155 = CARTESIAN_POINT ( 'NONE',  ( 10.00000000000000000, 2.946379043147425492, -75.11764819372145041 ) ) ;
#4156 = ORIENTED_EDGE ( 'NONE', *, *, #44088, .F. ) ;
#4157 = AXIS2_PLACEMENT_3D ( 'NONE', #27776, #16748, #31698 ) ;
#4158 = LINE ( 'NONE', #48445, #2606 ) ;
#4159 = CARTESIAN_POINT ( 'NONE',  ( 0.000000000000000000, -120.0000000000000000, 5.500000000000000888 ) ) ;
#4160 = CARTESIAN_POINT ( 'NONE',  ( 11.99999999999999822, 75.11764819372142199, 2.946379043147685728 ) ) ;
#4161 = EDGE_CURVE ( 'NONE', #2738, #31325, #39476, .T. ) ;
#4162 = EDGE_CURVE ( 'NONE', #29283, #24216, #6750, .T. ) ;
#4163 = ORIENTED_EDGE ( 'NONE', *, *, #41011, .F. ) ;
#4164 = UNCERTAINTY_MEASURE_WITH_UNIT (LENGTH_MEASURE( 1.000000000000000082E-05 ), #21552, 'distance_accuracy_value', 'NONE');
#4165 = CYLINDRICAL_SURFACE ( 'NONE', #13621, 82.00000000000000000 ) ;
#4166 = CARTESIAN_POINT ( 'NONE',  ( 11.99999999999999822, -46.21855187248585395, -62.20884554314068993 ) ) ;
#4167 = AXIS2_PLACEMENT_3D ( 'NONE', #15184, #44545, #33042 ) ;
#4168 = DIRECTION ( 'NONE',  ( -1.000000000000000000, -0.000000000000000000, -0.000000000000000000 ) ) ;
#4169 = ORIENTED_EDGE ( 'NONE', *, *, #38145, .T. ) ;
#4170 = VECTOR ( 'NONE', #24251, 1000.000000000000000 ) ;
#4171 = EDGE_CURVE ( 'NONE', #35650, #8522, #2487, .T. ) ;
#4172 = FACE_OUTER_BOUND ( 'NONE', #23018, .T. ) ;
#4173 = CIRCLE ( 'NONE', #29951, 82.00000000000000000 ) ;
#4174 = VECTOR ( 'NONE', #47882, 1000.000000000000000 ) ;
#4175 = ORIENTED_EDGE ( 'NONE', *, *, #32777, .T. ) ;
#4176 = ORIENTED_EDGE ( 'NONE', *, *, #46618, .F. ) ;
#4177 = CIRCLE ( 'NONE', #236, 42.00000000000000000 ) ;
#4178 = VERTEX_POINT ( 'NONE', #47519 ) ;
#4179 = VERTEX_POINT ( 'NONE', #32129 ) ;
#4180 = ORIENTED_EDGE ( 'NONE', *, *, #45631, .F. ) ;
#4181 = AXIS2_PLACEMENT_3D ( 'NONE', #33462, #14866, #29784 ) ;
#4182 = CYLINDRICAL_SURFACE ( 'NONE', #40, 16.00000000000000000 ) ;
#4183 = VECTOR ( 'NONE', #21852, 1000.000000000000000 ) ;
#4184 = VECTOR ( 'NONE', #26548, 1000.000000000000000 ) ;
#4185 = ORIENTED_EDGE ( 'NONE', *, *, #13381, .T. ) ;
#4186 = VERTEX_POINT ( 'NONE', #43386 ) ;
#4187 = AXIS2_PLACEMENT_3D ( 'NONE', #11061, #18640, #26718 ) ;
#4188 = DIRECTION ( 'NONE',  ( 0.000000000000000000, 0.1564344650402312298, -0.9876883405951375483 ) ) ;
#4189 = VECTOR ( 'NONE', #2231, 1000.000000000000000 ) ;
#4190 = VERTEX_POINT ( 'NONE', #2037 ) ;
#4191 = CARTESIAN_POINT ( 'NONE',  ( 11.99999999999999822, 0.000000000000000000, 0.000000000000000000 ) ) ;
#4192 = CARTESIAN_POINT ( 'NONE',  ( -3.000000000000000000, -25.60904388321925396, 6.976881207771172377 ) ) ;
#4193 = ORIENTED_EDGE ( 'NONE', *, *, #24021, .F. ) ;
#4194 = CARTESIAN_POINT ( 'NONE',  ( 15.00000000000000000, 8.688484142254226938, 21.88630264137359305 ) ) ;
#4195 = ORIENTED_EDGE ( 'NONE', *, *, #32752, .F. ) ;
#4196 = CARTESIAN_POINT ( 'NONE',  ( 11.99999999999999822, -62.20884554314051229, 46.21855187248609553 ) ) ;
#4197 = CARTESIAN_POINT ( 'NONE',  ( 11.99999999999999822, 73.72996012237460661, -14.67089635893632504 ) ) ;
#4198 = VERTEX_POINT ( 'NONE', #25000 ) ;
#4199 = CYLINDRICAL_SURFACE ( 'NONE', #610, 32.00000000000000000 ) ;
#4200 = ORIENTED_EDGE ( 'NONE', *, *, #13047, .F. ) ;
#4201 = ORIENTED_EDGE ( 'NONE', *, *, #25950, .F. ) ;
#4202 = LINE ( 'NONE', #30155, #45519 ) ;
#4203 = CARTESIAN_POINT ( 'NONE',  ( 10.00000000000000000, 74.65491531819118620, -8.830959090342659579 ) ) ;
#4204 = EDGE_CURVE ( 'NONE', #13208, #32168, #17680, .T. ) ;
#4205 = CARTESIAN_POINT ( 'NONE',  ( 0.000000000000000000, 0.000000000000000000, 0.000000000000000000 ) ) ;
#4206 = DIRECTION ( 'NONE',  ( -1.000000000000000000, 0.000000000000000000, -0.000000000000000000 ) ) ;
#4207 = DIRECTION ( 'NONE',  ( -1.000000000000000000, -0.000000000000000000, 0.000000000000000000 ) ) ;
#4208 = EDGE_CURVE ( 'NONE', #16066, #29887, #46815, .T. ) ;
#4209 = CARTESIAN_POINT ( 'NONE',  ( 0.000000000000000000, 78.73519480814985627, -22.90783923731548199 ) ) ;
#4210 = EDGE_CURVE ( 'NONE', #3259, #11083, #25231, .T. ) ;
#4211 = CARTESIAN_POINT ( 'NONE',  ( 10.00000000000000000, 16.65972982744934683, 80.28980883073762698 ) ) ;
#4212 = CIRCLE ( 'NONE', #31576, 12.49999999999999645 ) ;
#4213 = PLANE ( 'NONE',  #40358 ) ;
#4214 = ORIENTED_EDGE ( 'NONE', *, *, #21143, .T. ) ;
#4215 = DIRECTION ( 'NONE',  ( 0.000000000000000000, 0.5877852522924689183, 0.8090169943749504489 ) ) ;
#4216 = EDGE_CURVE ( 'NONE', #6463, #24385, #6414, .T. ) ;
#4217 = CARTESIAN_POINT ( 'NONE',  ( -7.670864526094549163, -97.73662565058241114, -5.500000000000000000 ) ) ;
#4218 = DIRECTION ( 'NONE',  ( -1.000000000000000000, -0.000000000000000000, -0.000000000000000000 ) ) ;
#4219 = CIRCLE ( 'NONE', #31580, 16.00000000000000000 ) ;
#4220 = AXIS2_PLACEMENT_3D ( 'NONE', #13110, #35124, #9190 ) ;
#4221 = VECTOR ( 'NONE', #30298, 1000.000000000000114 ) ;
#4222 = CARTESIAN_POINT ( 'NONE',  ( 11.99999999999999822, 14.66109333815460225, 73.73191006444577056 ) ) ;
#4223 = CARTESIAN_POINT ( 'NONE',  ( 0.000000000000000000, 81.50828551894227303, 8.966570791700979370 ) ) ;
#4224 = DIRECTION ( 'NONE',  ( 0.000000000000000000, 0.000000000000000000, 1.000000000000000000 ) ) ;
#4225 = DIRECTION ( 'NONE',  ( -1.000000000000000000, -0.000000000000000000, -0.000000000000000000 ) ) ;
#4226 = VERTEX_POINT ( 'NONE', #10573 ) ;
#4227 = ADVANCED_FACE ( 'NONE', ( #17662 ), #21086, .T. ) ;
#4228 = ORIENTED_EDGE ( 'NONE', *, *, #22524, .T. ) ;
#4229 = FACE_BOUND ( 'NONE', #36849, .T. ) ;
#4230 = VECTOR ( 'NONE', #33815, 1000.000000000000000 ) ;
#4231 = ORIENTED_EDGE ( 'NONE', *, *, #33058, .T. ) ;
#4232 = EDGE_CURVE ( 'NONE', #35871, #37888, #8318, .T. ) ;
#4233 = AXIS2_PLACEMENT_3D ( 'NONE', #41356, #11731, #8044 ) ;
#4234 = DIRECTION ( 'NONE',  ( -1.000000000000000000, -0.000000000000000000, 0.000000000000000000 ) ) ;
#4235 = AXIS2_PLACEMENT_3D ( 'NONE', #36482, #21788, #7100 ) ;
#4236 = APPLICATION_PROTOCOL_DEFINITION ( 'draft international standard', 'automotive_design', 1998, #13219 ) ;
#4237 = DIRECTION ( 'NONE',  ( -1.000000000000000000, -0.000000000000000000, -0.000000000000000000 ) ) ;
#4238 = VECTOR ( 'NONE', #45848, 1000.000000000000000 ) ;
#4239 = ORIENTED_EDGE ( 'NONE', *, *, #16396, .T. ) ;
#4240 = EDGE_CURVE ( 'NONE', #43656, #43844, #34906, .T. ) ;
#4241 = CARTESIAN_POINT ( 'NONE',  ( 0.000000000000000000, 33.71516098798849015, -74.74816331893394761 ) ) ;
#4242 = ORIENTED_EDGE ( 'NONE', *, *, #27612, .T. ) ;
#4243 = ADVANCED_FACE ( 'NONE', ( #28695 ), #32594, .F. ) ;
#4244 = AXIS2_PLACEMENT_3D ( 'NONE', #1789, #27503, #43151 ) ;
#4245 = DIRECTION ( 'NONE',  ( 0.000000000000000000, -0.4067366430757887730, 0.9135454576426059736 ) ) ;
#4246 = CARTESIAN_POINT ( 'NONE',  ( 0.000000000000000000, -4.261787119644969479, -26.19803753235780519 ) ) ;
#4247 = CIRCLE ( 'NONE', #24542, 82.00000000000000000 ) ;
#4249 = ORIENTED_EDGE ( 'NONE', *, *, #34403, .F. ) ;
#4248 = CARTESIAN_POINT ( 'NONE',  ( 10.00000000000000000, 26.08949754953024325, 27.05870788708241648 ) ) ;
#4250 = AXIS2_PLACEMENT_3D ( 'NONE', #44664, #48098, #3786 ) ;
#4251 = VERTEX_POINT ( 'NONE', #43141 ) ;
#4252 = CIRCLE ( 'NONE', #6581, 77.49900000000000944 ) ;
#4253 = ORIENTED_EDGE ( 'NONE', *, *, #26981, .T. ) ;
#4254 = DIRECTION ( 'NONE',  ( 0.000000000000000000, 0.000000000000000000, 1.000000000000000000 ) ) ;
#4255 = DIRECTION ( 'NONE',  ( 0.7273375899149802093, -0.6862798483830544471, 0.000000000000000000 ) ) ;
#4256 = DIRECTION ( 'NONE',  ( -1.000000000000000000, 0.000000000000000000, -0.000000000000000000 ) ) ;
#4258 = ORIENTED_EDGE ( 'NONE', *, *, #4266, .F. ) ;
#4257 = CARTESIAN_POINT ( 'NONE',  ( 0.000000000000000000, 31.46837873495072913, -68.27212725128242710 ) ) ;
#4259 = CIRCLE ( 'NONE', #40216, 31.99999999999998934 ) ;
#4260 = VECTOR ( 'NONE', #14450, 1000.000000000000000 ) ;
#4261 = VERTEX_POINT ( 'NONE', #40193 ) ;
#4262 = DIRECTION ( 'NONE',  ( 0.000000000000000000, -0.9876883405951358830, -0.1564344650402421932 ) ) ;
#4263 = ORIENTED_EDGE ( 'NONE', *, *, #47960, .T. ) ;
#4264 = ORIENTED_EDGE ( 'NONE', *, *, #22224, .T. ) ;
#4265 = AXIS2_PLACEMENT_3D ( 'NONE', #12951, #701, #45992 ) ;
#4266 = EDGE_CURVE ( 'NONE', #39544, #20444, #21811, .T. ) ;
#4267 = CARTESIAN_POINT ( 'NONE',  ( 3.429551818649054340, -146.3199197248623875, 5.500000000000000000 ) ) ;
#4268 = AXIS2_PLACEMENT_3D ( 'NONE', #2638, #18301, #21245 ) ;
#4269 = EDGE_CURVE ( 'NONE', #32513, #46010, #28660, .T. ) ;
#4270 = CARTESIAN_POINT ( 'NONE',  ( 0.000000000000000000, 0.000000000000000000, -40.00000000000000000 ) ) ;
#4271 = LINE ( 'NONE', #18921, #44561 ) ;
#4272 = CARTESIAN_POINT ( 'NONE',  ( -3.000000000000000000, 5.835314593368772229, -22.81335362449846826 ) ) ;
#4273 = ORIENTED_EDGE ( 'NONE', *, *, #24861, .F. ) ;
#4274 = CYLINDRICAL_SURFACE ( 'NONE', #41734, 37.49900000000000233 ) ;
#4275 = CIRCLE ( 'NONE', #28511, 82.00000000000000000 ) ;
#4276 = DIRECTION ( 'NONE',  ( 0.000000000000000000, 0.7431448254773960205, -0.6691306063588563502 ) ) ;
#4277 = ADVANCED_FACE ( 'NONE', ( #30382 ), #40659, .F. ) ;
#4278 = FACE_OUTER_BOUND ( 'NONE', #32052, .T. ) ;
#4279 = DIRECTION ( 'NONE',  ( -0.9827303690289279636, -0.1850432970638682117, 0.000000000000000000 ) ) ;
#4280 = CARTESIAN_POINT ( 'NONE',  ( 11.99999999999999822, 55.20638768913760686, 51.02545421589343988 ) ) ;
#4281 = CARTESIAN_POINT ( 'NONE',  ( 4.999999999999999112, -36.13751322684434797, 21.40280677340357940 ) ) ;
#4283 = ADVANCED_FACE ( 'NONE', ( #14962 ), #14484, .T. ) ;
#4282 = DIRECTION ( 'NONE',  ( -1.000000000000000000, 0.000000000000000000, -0.000000000000000000 ) ) ;
#4284 = CARTESIAN_POINT ( 'NONE',  ( 0.000000000000000000, -23.16143007188479075, 73.95703589263966649 ) ) ;
#4285 = DIRECTION ( 'NONE',  ( 0.000000000000000000, 0.9238795325112851842, 0.3826834323650937786 ) ) ;
#4286 = CARTESIAN_POINT ( 'NONE',  ( 0.000000000000000000, 77.32052557432849937, -5.256550761632002633 ) ) ;
#4287 = LINE ( 'NONE', #27041, #25458 ) ;
#4288 = ORIENTED_EDGE ( 'NONE', *, *, #38592, .F. ) ;
#4289 = CIRCLE ( 'NONE', #7377, 77.49899999999999523 ) ;
#4290 = CARTESIAN_POINT ( 'NONE',  ( 0.000000000000000000, -39.78640506895651185, 66.50666863321987421 ) ) ;
#4291 = DIRECTION ( 'NONE',  ( -0.000000000000000000, -0.000000000000000000, -1.000000000000000000 ) ) ;
#4292 = DIRECTION ( 'NONE',  ( 0.000000000000000000, 0.000000000000000000, 1.000000000000000000 ) ) ;
#4293 = ORIENTED_EDGE ( 'NONE', *, *, #28755, .F. ) ;
#4294 = VECTOR ( 'NONE', #39015, 1000.000000000000000 ) ;
#4295 = PRODUCT_DEFINITION_SHAPE ( 'NONE', 'NONE',  #48459 ) ;
#4296 = DIRECTION ( 'NONE',  ( 1.000000000000000000, -0.000000000000000000, 0.000000000000000000 ) ) ;
#4297 = ORIENTED_EDGE ( 'NONE', *, *, #18834, .F. ) ;
#4298 = CIRCLE ( 'NONE', #5063, 82.00000000000000000 ) ;
#4299 = VECTOR ( 'NONE', #14583, 1000.000000000000000 ) ;
#4300 = CIRCLE ( 'NONE', #21475, 31.99999999999998934 ) ;
#4301 = VERTEX_POINT ( 'NONE', #25964 ) ;
#4302 = AXIS2_PLACEMENT_3D ( 'NONE', #39760, #2522, #21371 ) ;
#4303 = AXIS2_PLACEMENT_3D ( 'NONE', #34770, #31120, #46043 ) ;
#4304 = DIRECTION ( 'NONE',  ( 0.000000000000000000, 0.000000000000000000, 1.000000000000000000 ) ) ;
#4305 = ORIENTED_EDGE ( 'NONE', *, *, #17282, .T. ) ;
#4306 = DIRECTION ( 'NONE',  ( 0.000000000000000000, 0.000000000000000000, 1.000000000000000000 ) ) ;
#4307 = ORIENTED_EDGE ( 'NONE', *, *, #27409, .T. ) ;
#4308 = CARTESIAN_POINT ( 'NONE',  ( 10.00000000000000000, 46.53671651293948486, 59.03961581697416250 ) ) ;
#4309 = DIRECTION ( 'NONE',  ( 0.000000000000000000, 0.000000000000000000, 1.000000000000000000 ) ) ;
#4310 = ORIENTED_EDGE ( 'NONE', *, *, #21274, .T. ) ;
#4311 = DIRECTION ( 'NONE',  ( 0.000000000000000000, -0.8090169943749402348, -0.5877852522924830181 ) ) ;
#4312 = VERTEX_POINT ( 'NONE', #18128 ) ;
#4313 = CARTESIAN_POINT ( 'NONE',  ( 5.999999999999999112, -63.97538442413390669, -51.29473840253292138 ) ) ;
#4314 = PLANE ( 'NONE',  #107 ) ;
#4316 = CARTESIAN_POINT ( 'NONE',  ( -10.00000000000000000, 0.000000000000000000, 0.000000000000000000 ) ) ;
#4315 = AXIS2_PLACEMENT_3D ( 'NONE', #11496, #37428, #3896 ) ;
#4317 = ORIENTED_EDGE ( 'NONE', *, *, #8241, .F. ) ;
#4318 = EDGE_LOOP ( 'NONE', ( #29922, #37525, #7279, #34533 ) ) ;
#4319 = ORIENTED_EDGE ( 'NONE', *, *, #8783, .F. ) ;
#4320 = DIRECTION ( 'NONE',  ( 0.000000000000000000, 0.4539904997395479702, -0.8910065241883673437 ) ) ;
#4321 = EDGE_LOOP ( 'NONE', ( #26402, #38211, #36173, #32922 ) ) ;
#4322 = EDGE_CURVE ( 'NONE', #26338, #45549, #11539, .T. ) ;
#4323 = AXIS2_PLACEMENT_3D ( 'NONE', #6190, #9852, #35072 ) ;
#4324 = DIRECTION ( 'NONE',  ( -1.000000000000000000, 0.000000000000000000, 0.000000000000000000 ) ) ;
#4325 = DIRECTION ( 'NONE',  ( 1.000000000000000000, -0.000000000000000000, -0.000000000000000000 ) ) ;
#4326 = CARTESIAN_POINT ( 'NONE',  ( 10.00000000000000000, -35.53030884539094103, 12.26510123303246935 ) ) ;
#4327 = LINE ( 'NONE', #4794, #22962 ) ;
#4328 = DIRECTION ( 'NONE',  ( -1.000000000000000000, -0.000000000000000000, -0.000000000000000000 ) ) ;
#4329 = ADVANCED_FACE ( 'NONE', ( #22547 ), #37477, .T. ) ;
#4330 = CARTESIAN_POINT ( 'NONE',  ( 15.00000000000000000, -0.9646360437375368635, -23.52805723605589705 ) ) ;
#4331 = CARTESIAN_POINT ( 'NONE',  ( 0.000000000000000000, 0.000000000000000000, 0.000000000000000000 ) ) ;
#4332 = ORIENTED_EDGE ( 'NONE', *, *, #43443, .T. ) ;
#4333 = LINE ( 'NONE', #38097, #10249 ) ;
#4334 = CYLINDRICAL_SURFACE ( 'NONE', #35533, 32.00000000000000000 ) ;
#4335 = ORIENTED_EDGE ( 'NONE', *, *, #26981, .F. ) ;
#4336 = CARTESIAN_POINT ( 'NONE',  ( -3.000000000000000000, 8.688484142254221609, -21.88630264137359660 ) ) ;
#4337 = AXIS2_PLACEMENT_3D ( 'NONE', #9639, #1589, #20183 ) ;
#4338 = AXIS2_PLACEMENT_3D ( 'NONE', #24536, #21589, #17174 ) ;
#4339 = ORIENTED_EDGE ( 'NONE', *, *, #24489, .F. ) ;
#4340 = ORIENTED_EDGE ( 'NONE', *, *, #41488, .T. ) ;
#4342 = EDGE_CURVE ( 'NONE', #4790, #23277, #44336, .T. ) ;
#4341 = CARTESIAN_POINT ( 'NONE',  ( 10.00000000000000000, -41.76106447765533147, 62.50884508063410294 ) ) ;
#4343 = DIRECTION ( 'NONE',  ( 1.000000000000000000, 0.000000000000000000, -0.000000000000000000 ) ) ;
#4344 = EDGE_CURVE ( 'NONE', #13122, #5353, #29414, .T. ) ;
#4345 = DIRECTION ( 'NONE',  ( 0.02332147558787671729, 0.9997280174009349762, -0.000000000000000000 ) ) ;
#4346 = CARTESIAN_POINT ( 'NONE',  ( 15.00000000000000000, 14.60985201121729737, 18.46759930825687235 ) ) ;
#4347 = AXIS2_PLACEMENT_3D ( 'NONE', #18850, #41391, #7613 ) ;
#4348 = CARTESIAN_POINT ( 'NONE',  ( 5.822613034544236399, -142.8165987265839760, 5.500000000000000000 ) ) ;
#4349 = FACE_OUTER_BOUND ( 'NONE', #38065, .T. ) ;
#4350 = CIRCLE ( 'NONE', #31712, 77.49899999999999523 ) ;
#4351 = DIRECTION ( 'NONE',  ( -1.000000000000000000, -0.000000000000000000, 0.000000000000000000 ) ) ;
#4352 = DIRECTION ( 'NONE',  ( 1.000000000000000000, 0.000000000000000000, 0.000000000000000000 ) ) ;
#4353 = EDGE_CURVE ( 'NONE', #2189, #18404, #42706, .T. ) ;
#4354 = AXIS2_PLACEMENT_3D ( 'NONE', #47958, #47254, #13729 ) ;
#4355 = SURFACE_STYLE_USAGE ( .BOTH. , #890 ) ;
#4356 = CARTESIAN_POINT ( 'NONE',  ( 11.99999999999999822, 0.000000000000000000, 0.000000000000000000 ) ) ;
#4357 = VERTEX_POINT ( 'NONE', #18854 ) ;
#4358 = ORIENTED_EDGE ( 'NONE', *, *, #3299, .F. ) ;
#4359 = AXIS2_PLACEMENT_3D ( 'NONE', #1324, #38781, #15297 ) ;
#4360 = ORIENTED_EDGE ( 'NONE', *, *, #23706, .T. ) ;
#4361 = EDGE_LOOP ( 'NONE', ( #25135, #27732, #22578, #460 ) ) ;
#4362 = LINE ( 'NONE', #8003, #23384 ) ;
#4363 = CARTESIAN_POINT ( 'NONE',  ( 0.000000000000000000, -22.48208911017525580, 35.47612816024516036 ) ) ;
#4364 = ORIENTED_EDGE ( 'NONE', *, *, #14528, .T. ) ;
#4365 = EDGE_CURVE ( 'NONE', #14824, #1839, #41140, .T. ) ;
#4366 = CIRCLE ( 'NONE', #31742, 32.00000000000000000 ) ;
#4367 = CYLINDRICAL_SURFACE ( 'NONE', #2284, 77.49899999999999523 ) ;
#4368 = EDGE_CURVE ( 'NONE', #10399, #16188, #4417, .T. ) ;
#4369 = VERTEX_POINT ( 'NONE', #22312 ) ;
#4370 = CIRCLE ( 'NONE', #40328, 31.99999999999999289 ) ;
#4371 = EDGE_LOOP ( 'NONE', ( #257, #24392, #30476, #11036 ) ) ;
#4372 = EDGE_CURVE ( 'NONE', #23243, #48285, #32531, .T. ) ;
#4373 = CIRCLE ( 'NONE', #46577, 31.99999999999998579 ) ;
#4374 = CYLINDRICAL_SURFACE ( 'NONE', #21014, 77.49899999999999523 ) ;
#4376 = ORIENTED_EDGE ( 'NONE', *, *, #34726, .F. ) ;
#4375 = PLANE ( 'NONE',  #18825 ) ;
#4377 = CARTESIAN_POINT ( 'NONE',  ( 10.00000000000000000, 0.000000000000000000, 0.000000000000000000 ) ) ;
#4378 = ORIENTED_EDGE ( 'NONE', *, *, #1900, .F. ) ;
#4379 = ORIENTED_EDGE ( 'NONE', *, *, #45938, .F. ) ;
#4380 = CARTESIAN_POINT ( 'NONE',  ( -10.00000000000000000, 0.000000000000000000, 0.000000000000000000 ) ) ;
#4381 = EDGE_LOOP ( 'NONE', ( #10742, #4714, #16922, #3391 ) ) ;
#4382 = VERTEX_POINT ( 'NONE', #7127 ) ;
#4383 = FACE_OUTER_BOUND ( 'NONE', #42783, .T. ) ;
#4384 = AXIS2_PLACEMENT_3D ( 'NONE', #39858, #9502, #43048 ) ;
#4385 = CARTESIAN_POINT ( 'NONE',  ( 4.348517481000897078, -143.0941636721797465, -2.500000000000000000 ) ) ;
#4386 = EDGE_CURVE ( 'NONE', #15128, #16057, #10669, .T. ) ;
#4387 = CYLINDRICAL_SURFACE ( 'NONE', #29135, 32.00000000000000000 ) ;
#4388 = VECTOR ( 'NONE', #27248, 1000.000000000000000 ) ;
#4389 = ORIENTED_EDGE ( 'NONE', *, *, #14264, .F. ) ;
#4390 = EDGE_CURVE ( 'NONE', #2942, #44487, #41164, .T. ) ;
#4391 = ADVANCED_FACE ( 'NONE', ( #3451 ), #44572, .T. ) ;
#4392 = ORIENTED_EDGE ( 'NONE', *, *, #32506, .T. ) ;
#4393 = PLANE ( 'NONE',  #34458 ) ;
#4394 = AXIS2_PLACEMENT_3D ( 'NONE', #17690, #11069, #14257 ) ;
#4395 = DIRECTION ( 'NONE',  ( 0.000000000000000000, 1.000000000000000000, 0.000000000000000000 ) ) ;
#4396 = ORIENTED_EDGE ( 'NONE', *, *, #5654, .T. ) ;
#4397 = CARTESIAN_POINT ( 'NONE',  ( 0.000000000000000000, 0.000000000000000000, 125.0000000000000000 ) ) ;
#4398 = EDGE_LOOP ( 'NONE', ( #22307, #45341, #2278, #37703 ) ) ;
#4399 = CARTESIAN_POINT ( 'NONE',  ( 0.000000000000000000, -81.50828551894220197, -8.966570791701583332 ) ) ;
#4400 = CARTESIAN_POINT ( 'NONE',  ( 0.000000000000000000, -10.96151621346461447, -35.95386929396268272 ) ) ;
#4401 = CARTESIAN_POINT ( 'NONE',  ( 0.000000000000000000, -120.0000000000000000, 40.00000000000000711 ) ) ;
#4402 = CARTESIAN_POINT ( 'NONE',  ( 0.000000000000000000, 17.80606268964585226, -33.00180498840028775 ) ) ;
#4403 = CARTESIAN_POINT ( 'NONE',  ( 0.000000000000000000, 16.95692799528845640, -1.176623242955009039E-14 ) ) ;
#4404 = CARTESIAN_POINT ( 'NONE',  ( 15.00000000000000000, -4.261787119644963262, 26.19803753235780164 ) ) ;
#4405 = PLANE ( 'NONE',  #23225 ) ;
#4406 = VECTOR ( 'NONE', #36394, 1000.000000000000114 ) ;
#4407 = LINE ( 'NONE', #29845, #17685 ) ;
#4408 = FACE_OUTER_BOUND ( 'NONE', #37610, .T. ) ;
#4409 = AXIS2_PLACEMENT_3D ( 'NONE', #25251, #43160, #25021 ) ;
#4410 = DIRECTION ( 'NONE',  ( 1.000000000000000000, 0.000000000000000000, -0.000000000000000000 ) ) ;
#4411 = DIRECTION ( 'NONE',  ( 0.000000000000000000, 0.000000000000000000, 1.000000000000000000 ) ) ;
#4412 = LINE ( 'NONE', #11511, #32666 ) ;
#4413 = VERTEX_POINT ( 'NONE', #18387 ) ;
#4414 = CARTESIAN_POINT ( 'NONE',  ( 15.00000000000000000, 18.84667830672605859, 18.68964196561243796 ) ) ;
#4415 = VECTOR ( 'NONE', #5416, 1000.000000000000000 ) ;
#4416 = DIRECTION ( 'NONE',  ( -0.9827303690289279636, -0.1850432970638682117, 0.000000000000000000 ) ) ;
#4417 = CIRCLE ( 'NONE', #495, 77.49900000000002365 ) ;
#4418 = LINE ( 'NONE', #45771, #1068 ) ;
#4419 = VERTEX_POINT ( 'NONE', #14726 ) ;
#4420 = ADVANCED_FACE ( 'NONE', ( #8093 ), #18626, .T. ) ;
#4421 = AXIS2_PLACEMENT_3D ( 'NONE', #5126, #31318, #27898 ) ;
#4422 = ORIENTED_EDGE ( 'NONE', *, *, #45697, .T. ) ;
#4423 = ADVANCED_FACE ( 'NONE', ( #33069 ), #29884, .T. ) ;
#4424 = LINE ( 'NONE', #34490, #25786 ) ;
#4425 = ORIENTED_EDGE ( 'NONE', *, *, #109, .F. ) ;
#4426 = EDGE_CURVE ( 'NONE', #43334, #35253, #35004, .T. ) ;
#4427 = ORIENTED_EDGE ( 'NONE', *, *, #6299, .T. ) ;
#4428 = ORIENTED_EDGE ( 'NONE', *, *, #42660, .T. ) ;
#4429 = EDGE_CURVE ( 'NONE', #30390, #39278, #16156, .T. ) ;
#4430 = AXIS2_PLACEMENT_3D ( 'NONE', #38567, #11895, #5033 ) ;
#4431 = CARTESIAN_POINT ( 'NONE',  ( 10.00000000000000000, -33.17418723428294669, -17.67226234102862747 ) ) ;
#4432 = ORIENTED_EDGE ( 'NONE', *, *, #40707, .F. ) ;
#4433 = ORIENTED_EDGE ( 'NONE', *, *, #47454, .T. ) ;
#4434 = CARTESIAN_POINT ( 'NONE',  ( 10.00000000000000000, -27.13269053701078448, -25.88420570971428702 ) ) ;
#4435 = ORIENTED_EDGE ( 'NONE', *, *, #24594, .T. ) ;
#4436 = VECTOR ( 'NONE', #39181, 1000.000000000000000 ) ;
#4437 = PLANE ( 'NONE',  #37943 ) ;
#4438 = CARTESIAN_POINT ( 'NONE',  ( 10.00000000000000000, 17.67226234102874116, -33.17418723428288274 ) ) ;
#4439 = EDGE_LOOP ( 'NONE', ( #4724, #31097, #7764, #12357 ) ) ;
#4440 = EDGE_CURVE ( 'NONE', #28690, #40406, #45856, .T. ) ;
#4441 = LINE ( 'NONE', #8808, #27455 ) ;
#4442 = EDGE_CURVE ( 'NONE', #24728, #1214, #31019, .T. ) ;
#4443 = ORIENTED_EDGE ( 'NONE', *, *, #35276, .T. ) ;
#4445 = EDGE_LOOP ( 'NONE', ( #36165, #32617, #903, #8797 ) ) ;
#4444 = FACE_OUTER_BOUND ( 'NONE', #6653, .T. ) ;
#4446 = CARTESIAN_POINT ( 'NONE',  ( 11.99999999999999822, -6.903761155837269570, -77.19088730480530103 ) ) ;
#4447 = ORIENTED_EDGE ( 'NONE', *, *, #10374, .T. ) ;
#4448 = CARTESIAN_POINT ( 'NONE',  ( 10.00000000000000000, -20.41045688087876897, 72.35160999960810102 ) ) ;
#4449 = ORIENTED_EDGE ( 'NONE', *, *, #15213, .T. ) ;
#4450 = ORIENTED_EDGE ( 'NONE', *, *, #43051, .F. ) ;
#4451 = DIRECTION ( 'NONE',  ( 1.000000000000000000, -0.000000000000000000, -0.000000000000000000 ) ) ;
#4452 = CARTESIAN_POINT ( 'NONE',  ( 0.000000000000000000, 55.16347631943131802, -60.67117009219074930 ) ) ;
#4453 = LINE ( 'NONE', #753, #43424 ) ;
#4454 = CARTESIAN_POINT ( 'NONE',  ( 0.000000000000000000, 0.000000000000000000, -43.79999999999998295 ) ) ;
#4455 = FACE_OUTER_BOUND ( 'NONE', #42145, .T. ) ;
#4456 = DIRECTION ( 'NONE',  ( 0.000000000000000000, -6.982962677686266711E-15, 1.000000000000000000 ) ) ;
#4457 = DIRECTION ( 'NONE',  ( -1.000000000000000000, -0.000000000000000000, 0.000000000000000000 ) ) ;
#4458 = EDGE_CURVE ( 'NONE', #7133, #3407, #42325, .T. ) ;
#4459 = VECTOR ( 'NONE', #11922, 1000.000000000000000 ) ;
#4460 = DIRECTION ( 'NONE',  ( 0.000000000000000000, 0.000000000000000000, 1.000000000000000000 ) ) ;
#4461 = DIRECTION ( 'NONE',  ( -0.000000000000000000, -0.000000000000000000, -1.000000000000000000 ) ) ;
#4462 = CARTESIAN_POINT ( 'NONE',  ( 11.99999999999999822, 76.69515212746016175, 29.01471420065590578 ) ) ;
#4463 = CARTESIAN_POINT ( 'NONE',  ( 10.00000000000000000, -6.555932627142143865, -37.01155633439065440 ) ) ;
#4464 = ORIENTED_EDGE ( 'NONE', *, *, #3239, .T. ) ;
#4465 = FACE_OUTER_BOUND ( 'NONE', #23033, .T. ) ;
#4466 = CARTESIAN_POINT ( 'NONE',  ( -3.000000000000000000, -22.67460108101783334, 6.353146135317912169 ) ) ;
#4467 = CARTESIAN_POINT ( 'NONE',  ( 11.99999999999999822, 0.000000000000000000, 0.000000000000000000 ) ) ;
#4468 = ORIENTED_EDGE ( 'NONE', *, *, #33039, .F. ) ;
#4469 = VECTOR ( 'NONE', #821, 1000.000000000000000 ) ;
#4470 = CIRCLE ( 'NONE', #9907, 82.00000000000000000 ) ;
#4471 = LINE ( 'NONE', #41923, #22236 ) ;
#4472 = VERTEX_POINT ( 'NONE', #41885 ) ;
#4473 = DIRECTION ( 'NONE',  ( -1.000000000000000000, -0.000000000000000000, -0.000000000000000000 ) ) ;
#4474 = PRODUCT_CONTEXT ( 'NONE', #12581, 'mechanical' ) ;
#4475 = AXIS2_PLACEMENT_3D ( 'NONE', #9263, #31559, #35924 ) ;
#4476 = DIRECTION ( 'NONE',  ( -1.000000000000000000, 0.000000000000000000, -0.000000000000000000 ) ) ;
#4477 = ORIENTED_EDGE ( 'NONE', *, *, #5985, .T. ) ;
#4478 = AXIS2_PLACEMENT_3D ( 'NONE', #15766, #18932, #18701 ) ;
#4479 = CARTESIAN_POINT ( 'NONE',  ( 5.000000000000000000, -79.10210256391353312, -21.60688246758668640 ) ) ;
#4480 = ADVANCED_FACE ( 'NONE', ( #27931 ), #42846, .T. ) ;
#4481 = ORIENTED_EDGE ( 'NONE', *, *, #34973, .F. ) ;
#4482 = EDGE_CURVE ( 'NONE', #19357, #46202, #25095, .T. ) ;
#4483 = AXIS2_PLACEMENT_3D ( 'NONE', #4814, #39307, #19719 ) ;
#4484 = CARTESIAN_POINT ( 'NONE',  ( -35.37301231164799731, -117.0000000000000000, 2.500000000000000000 ) ) ;
#4485 = ADVANCED_FACE ( 'NONE', ( #1482 ), #27192, .F. ) ;
#4486 = CARTESIAN_POINT ( 'NONE',  ( 11.99999999999999822, 0.000000000000000000, 0.000000000000000000 ) ) ;
#4487 = CARTESIAN_POINT ( 'NONE',  ( 15.07208474345548055, -141.7963818439230010, -2.500000000000000000 ) ) ;
#4488 = ORIENTED_EDGE ( 'NONE', *, *, #33025, .F. ) ;
#4489 = DIRECTION ( 'NONE',  ( 0.000000000000000000, 0.000000000000000000, -1.000000000000000000 ) ) ;
#4490 = CARTESIAN_POINT ( 'NONE',  ( 11.99999999999999822, 65.58780272294076497, 36.73666225445916211 ) ) ;
#4491 = EDGE_CURVE ( 'NONE', #15455, #27599, #7140, .T. ) ;
#4492 = PLANE ( 'NONE',  #25926 ) ;
#4494 = LINE ( 'NONE', #31171, #4674 ) ;
#4493 = VECTOR ( 'NONE', #13344, 1000.000000000000000 ) ;
#4495 = EDGE_LOOP ( 'NONE', ( #10672, #36609, #47612, #9646 ) ) ;
#4496 = DIRECTION ( 'NONE',  ( -1.000000000000000000, 0.000000000000000000, -0.000000000000000000 ) ) ;
#4497 = ORIENTED_EDGE ( 'NONE', *, *, #41792, .T. ) ;
#4498 = VERTEX_POINT ( 'NONE', #19821 ) ;
#4499 = EDGE_CURVE ( 'NONE', #45945, #13250, #46208, .T. ) ;
#4500 = CYLINDRICAL_SURFACE ( 'NONE', #23123, 31.99999999999998579 ) ;
#4501 = AXIS2_PLACEMENT_3D ( 'NONE', #34406, #419, #26372 ) ;
#4502 = DIRECTION ( 'NONE',  ( 0.000000000000000000, 0.000000000000000000, 1.000000000000000000 ) ) ;
#4503 = CARTESIAN_POINT ( 'NONE',  ( 10.00000000000000000, 0.000000000000000000, 0.000000000000000000 ) ) ;
#4504 = DIRECTION ( 'NONE',  ( 0.000000000000000000, 0.4539904997395476927, -0.8910065241883674547 ) ) ;
#4505 = ORIENTED_EDGE ( 'NONE', *, *, #37871, .T. ) ;
#4506 = CARTESIAN_POINT ( 'NONE',  ( 15.00000000000000000, 24.81905959214260804, -9.408202855044828894 ) ) ;
#4507 = DIRECTION ( 'NONE',  ( -1.000000000000000000, -0.000000000000000000, 0.000000000000000000 ) ) ;
#4508 = CARTESIAN_POINT ( 'NONE',  ( 11.99999999999999822, -31.47745569255092235, -68.26794271651296242 ) ) ;
#4509 = CARTESIAN_POINT ( 'NONE',  ( 10.00000000000000000, -27.13269053701078448, -25.88420570971428702 ) ) ;
#4510 = EDGE_CURVE ( 'NONE', #36037, #34495, #45532, .T. ) ;
#4511 = PLANE ( 'NONE',  #27856 ) ;
#4512 = CIRCLE ( 'NONE', #11530, 31.99999999999998934 ) ;
#4513 = DIRECTION ( 'NONE',  ( 0.000000000000000000, 0.7071067811865437980, 0.7071067811865512365 ) ) ;
#4514 = CARTESIAN_POINT ( 'NONE',  ( 15.00000000000000000, 0.000000000000000000, 0.000000000000000000 ) ) ;
#4515 = DIRECTION ( 'NONE',  ( 0.000000000000000000, -0.9238795325112822976, -0.3826834323651006620 ) ) ;
#4516 = CARTESIAN_POINT ( 'NONE',  ( 0.000000000000000000, 0.000000000000000000, 0.000000000000000000 ) ) ;
#4517 = DIRECTION ( 'NONE',  ( -1.000000000000000000, 0.000000000000000000, -0.000000000000000000 ) ) ;
#4518 = DIRECTION ( 'NONE',  ( -1.000000000000000000, 0.000000000000000000, 0.000000000000000000 ) ) ;
#4519 = AXIS2_PLACEMENT_3D ( 'NONE', #43355, #9556, #5916 ) ;
#4520 = ORIENTED_EDGE ( 'NONE', *, *, #32367, .F. ) ;
#4521 = CARTESIAN_POINT ( 'NONE',  ( -35.37301231164799731, -123.0000000000000142, 2.500000000000000000 ) ) ;
#4522 = DIRECTION ( 'NONE',  ( 0.000000000000000000, 0.000000000000000000, 1.000000000000000000 ) ) ;
#4523 = DIRECTION ( 'NONE',  ( -1.000000000000000000, -0.000000000000000000, -0.000000000000000000 ) ) ;
#4524 = VERTEX_POINT ( 'NONE', #34505 ) ;
#4525 = CARTESIAN_POINT ( 'NONE',  ( 10.00000000000000000, 71.87247863392470038, -39.47590169984768238 ) ) ;
#4526 = EDGE_LOOP ( 'NONE', ( #15628, #28172, #13458, #48225 ) ) ;
#4527 = CIRCLE ( 'NONE', #18562, 82.00000000000000000 ) ;
#4528 = EDGE_CURVE ( 'NONE', #10250, #42048, #11823, .T. ) ;
#4529 = ORIENTED_EDGE ( 'NONE', *, *, #44797, .T. ) ;
#4531 = EDGE_CURVE ( 'NONE', #41093, #39281, #15932, .T. ) ;
#4530 = AXIS2_PLACEMENT_3D ( 'NONE', #11569, #37741, #4224 ) ;
#4532 = VERTEX_POINT ( 'NONE', #27434 ) ;
#4533 = DIRECTION ( 'NONE',  ( 0.7585478161175723821, 0.6516173805718057377, 0.000000000000000000 ) ) ;
#4534 = ORIENTED_EDGE ( 'NONE', *, *, #38239, .F. ) ;
#4535 = ADVANCED_FACE ( 'NONE', ( #4902 ), #1722, .T. ) ;
#4536 = FACE_OUTER_BOUND ( 'NONE', #34645, .T. ) ;
#4537 = EDGE_CURVE ( 'NONE', #5207, #33303, #12502, .T. ) ;
#4538 = EDGE_CURVE ( 'NONE', #32290, #34023, #4441, .T. ) ;
#4539 = CARTESIAN_POINT ( 'NONE',  ( 11.99999999999999822, 59.46389618802034960, -49.70050353004825894 ) ) ;
#4540 = DIRECTION ( 'NONE',  ( -0.6064928550163524168, -0.7950889364178789220, 0.000000000000000000 ) ) ;
#4541 = ORIENTED_EDGE ( 'NONE', *, *, #14278, .F. ) ;
#4542 = DIRECTION ( 'NONE',  ( 0.000000000000000000, -0.9510565162951543083, 0.3090169943749448977 ) ) ;
#4543 = MECHANICAL_DESIGN_GEOMETRIC_PRESENTATION_REPRESENTATION (  '', ( #41345 ), #9328 ) ;
#4544 = EDGE_LOOP ( 'NONE', ( #18045, #5491, #30306, #6998 ) ) ;
#4545 = EDGE_LOOP ( 'NONE', ( #9000, #1149, #30941, #9109 ) ) ;
#4546 = DIRECTION ( 'NONE',  ( -1.000000000000000000, 0.000000000000000000, -0.000000000000000000 ) ) ;
#4547 = CARTESIAN_POINT ( 'NONE',  ( 7.468086116107294004, -12.33868914344945189, 0.000000000000000000 ) ) ;
#4548 = AXIS2_PLACEMENT_3D ( 'NONE', #3584, #44227, #3828 ) ;
#4549 = ORIENTED_EDGE ( 'NONE', *, *, #18417, .F. ) ;
#4550 = ORIENTED_EDGE ( 'NONE', *, *, #20098, .F. ) ;
#4551 = DIRECTION ( 'NONE',  ( -1.000000000000000000, 0.000000000000000000, 0.000000000000000000 ) ) ;
#4552 = ORIENTED_EDGE ( 'NONE', *, *, #30873, .T. ) ;
#4553 = DIRECTION ( 'NONE',  ( -1.000000000000000000, -0.000000000000000000, 0.000000000000000000 ) ) ;
#4554 = CYLINDRICAL_SURFACE ( 'NONE', #36581, 31.99999999999997868 ) ;
#4555 = DIRECTION ( 'NONE',  ( -0.4279312458753000703, -0.9038112904824842087, 0.000000000000000000 ) ) ;
#4556 = DIRECTION ( 'NONE',  ( -1.000000000000000000, 0.000000000000000000, -0.000000000000000000 ) ) ;
#4557 = CARTESIAN_POINT ( 'NONE',  ( 11.99999999999999822, 0.000000000000000000, 0.000000000000000000 ) ) ;
#4558 = CARTESIAN_POINT ( 'NONE',  ( 10.00000000000000000, 0.000000000000000000, 0.000000000000000000 ) ) ;
#4559 = DIRECTION ( 'NONE',  ( -1.000000000000000000, 0.000000000000000000, 0.000000000000000000 ) ) ;
#4560 = DIRECTION ( 'NONE',  ( -1.000000000000000000, -0.000000000000000000, 0.000000000000000000 ) ) ;
#4561 = DIRECTION ( 'NONE',  ( -1.000000000000000000, 0.000000000000000000, 0.000000000000000000 ) ) ;
#4562 = DIRECTION ( 'NONE',  ( 1.000000000000000000, 0.000000000000000000, 0.000000000000000000 ) ) ;
#4563 = ADVANCED_FACE ( 'NONE', ( #741 ), #12026, .F. ) ;
#4564 = DIRECTION ( 'NONE',  ( 0.000000000000000000, 0.000000000000000000, 1.000000000000000000 ) ) ;
#4565 = VERTEX_POINT ( 'NONE', #17839 ) ;
#4566 = VERTEX_POINT ( 'NONE', #1977 ) ;
#4567 = CYLINDRICAL_SURFACE ( 'NONE', #45840, 16.00000000000000000 ) ;
#4568 = CIRCLE ( 'NONE', #18637, 31.99999999999998579 ) ;
#4569 = DIRECTION ( 'NONE',  ( -1.000000000000000000, -0.000000000000000000, 0.000000000000000000 ) ) ;
#4570 = CARTESIAN_POINT ( 'NONE',  ( 0.000000000000000000, 36.73666225445988687, -65.58780272294035285 ) ) ;
#4571 = CARTESIAN_POINT ( 'NONE',  ( -7.572224309238338336, -145.4393675041377492, 5.500000000000000000 ) ) ;
#4572 = EDGE_CURVE ( 'NONE', #10514, #15128, #17600, .T. ) ;
#4573 = VECTOR ( 'NONE', #16287, 1000.000000000000000 ) ;
#4574 = DIRECTION ( 'NONE',  ( -1.000000000000000000, -0.000000000000000000, 0.000000000000000000 ) ) ;
#4575 = CYLINDRICAL_SURFACE ( 'NONE', #29508, 31.99999999999998579 ) ;
#4576 = EDGE_CURVE ( 'NONE', #44846, #29574, #35268, .T. ) ;
#4577 = ORIENTED_EDGE ( 'NONE', *, *, #22021, .T. ) ;
#4578 = CARTESIAN_POINT ( 'NONE',  ( 10.00000000000000000, -27.05870788708213226, -26.08949754953053102 ) ) ;
#4579 = DIRECTION ( 'NONE',  ( -1.000000000000000000, 0.000000000000000000, 0.000000000000000000 ) ) ;
#4580 = AXIS2_PLACEMENT_3D ( 'NONE', #3737, #14764, #40699 ) ;
#4581 = DIRECTION ( 'NONE',  ( 0.000000000000000000, 0.000000000000000000, 1.000000000000000000 ) ) ;
#4582 = VERTEX_POINT ( 'NONE', #47466 ) ;
#4583 = AXIS2_PLACEMENT_3D ( 'NONE', #545, #23058, #12298 ) ;
#4584 = ORIENTED_EDGE ( 'NONE', *, *, #32230, .F. ) ;
#4585 = EDGE_CURVE ( 'NONE', #2093, #11149, #29008, .T. ) ;
#4586 = VERTEX_POINT ( 'NONE', #47233 ) ;
#4587 = DIRECTION ( 'NONE',  ( 0.6691306063588569053, 0.7431448254773954654, 0.000000000000000000 ) ) ;
#4588 = EDGE_CURVE ( 'NONE', #31998, #21026, #35732, .T. ) ;
#4589 = LINE ( 'NONE', #22944, #2661 ) ;
#4590 = EDGE_LOOP ( 'NONE', ( #38749, #25039, #39816, #33011 ) ) ;
#4591 = ADVANCED_FACE ( 'NONE', ( #13459 ), #43792, .T. ) ;
#4592 = CARTESIAN_POINT ( 'NONE',  ( 11.99999999999999822, 18.89407956138257205, 75.16055320797038064 ) ) ;
#4593 = CIRCLE ( 'NONE', #14771, 31.99999999999998579 ) ;
#4594 = ORIENTED_EDGE ( 'NONE', *, *, #19715, .F. ) ;
#4595 = EDGE_CURVE ( 'NONE', #15919, #13689, #39189, .T. ) ;
#4596 = ORIENTED_EDGE ( 'NONE', *, *, #44973, .F. ) ;
#4597 = CIRCLE ( 'NONE', #7743, 31.99999999999998579 ) ;
#4598 = CARTESIAN_POINT ( 'NONE',  ( -12.40464318976454727, 10.41032311384371667, -45.00000000000000000 ) ) ;
#4600 = VERTEX_POINT ( 'NONE', #28635 ) ;
#4599 = CARTESIAN_POINT ( 'NONE',  ( -3.000000000000000000, -20.55727247249748046, 16.78983467731285018 ) ) ;
#4601 = DIRECTION ( 'NONE',  ( -1.000000000000000000, -0.000000000000000000, -0.000000000000000000 ) ) ;
#4602 = ORIENTED_EDGE ( 'NONE', *, *, #33734, .F. ) ;
#4603 = DIRECTION ( 'NONE',  ( 0.000000000000000000, 0.000000000000000000, -1.000000000000000000 ) ) ;
#4604 = ORIENTED_EDGE ( 'NONE', *, *, #38140, .F. ) ;
#4605 = ORIENTED_EDGE ( 'NONE', *, *, #45502, .F. ) ;
#4606 = LINE ( 'NONE', #191, #16586 ) ;
#4607 = CARTESIAN_POINT ( 'NONE',  ( 11.99999999999999822, 0.000000000000000000, 0.000000000000000000 ) ) ;
#4608 = ORIENTED_EDGE ( 'NONE', *, *, #37578, .T. ) ;
#4609 = FACE_OUTER_BOUND ( 'NONE', #19287, .T. ) ;
#4610 = CARTESIAN_POINT ( 'NONE',  ( 11.99999999999999822, -75.16055320797043748, 18.89407956138231270 ) ) ;
#4611 = ORIENTED_EDGE ( 'NONE', *, *, #14144, .F. ) ;
#4612 = ORIENTED_EDGE ( 'NONE', *, *, #12889, .F. ) ;
#4613 = EDGE_CURVE ( 'NONE', #25392, #38067, #43330, .T. ) ;
#4614 = CYLINDRICAL_SURFACE ( 'NONE', #43073, 31.99999999999999289 ) ;
#4615 = DIRECTION ( 'NONE',  ( -1.000000000000000000, 0.000000000000000000, 0.000000000000000000 ) ) ;
#4616 = ORIENTED_EDGE ( 'NONE', *, *, #17064, .F. ) ;
#4617 = FACE_OUTER_BOUND ( 'NONE', #9249, .T. ) ;
#4618 = ORIENTED_EDGE ( 'NONE', *, *, #5634, .F. ) ;
#4619 = CARTESIAN_POINT ( 'NONE',  ( 0.000000000000000000, 0.000000000000000000, 0.000000000000000000 ) ) ;
#4620 = DIRECTION ( 'NONE',  ( -1.000000000000000000, 0.000000000000000000, 0.000000000000000000 ) ) ;
#4621 = DIRECTION ( 'NONE',  ( -1.000000000000000000, 0.000000000000000000, -0.000000000000000000 ) ) ;
#4622 = CARTESIAN_POINT ( 'NONE',  ( 13.83832728059186046, -142.6495187161941089, -2.500000000000000444 ) ) ;
#4623 = CARTESIAN_POINT ( 'NONE',  ( 0.000000000000000000, 54.21277698773752718, -55.38113227695725271 ) ) ;
#4624 = LINE ( 'NONE', #34232, #39081 ) ;
#4625 = CYLINDRICAL_SURFACE ( 'NONE', #35728, 32.00000000000000000 ) ;
#4626 = CARTESIAN_POINT ( 'NONE',  ( 15.00000000000000000, -22.67460108101782978, -6.353146135317906840 ) ) ;
#4627 = AXIS2_PLACEMENT_3D ( 'NONE', #22949, #26871, #11696 ) ;
#4628 = CARTESIAN_POINT ( 'NONE',  ( 11.99999999999999822, 58.39081064771751528, 50.95692526931350841 ) ) ;
#4629 = EDGE_LOOP ( 'NONE', ( #31717, #17587, #22411, #12628 ) ) ;
#4630 = EDGE_CURVE ( 'NONE', #5367, #29152, #14975, .T. ) ;
#4631 = VECTOR ( 'NONE', #20235, 1000.000000000000000 ) ;
#4632 = DIRECTION ( 'NONE',  ( -1.000000000000000000, -0.000000000000000000, -0.000000000000000000 ) ) ;
#4633 = FACE_OUTER_BOUND ( 'NONE', #25604, .T. ) ;
#4634 = CIRCLE ( 'NONE', #32007, 77.49899999999999523 ) ;
#4635 = DIRECTION ( 'NONE',  ( -1.000000000000000000, 0.000000000000000000, -0.000000000000000000 ) ) ;
#4636 = ORIENTED_EDGE ( 'NONE', *, *, #2628, .F. ) ;
#4637 = UNCERTAINTY_MEASURE_WITH_UNIT (LENGTH_MEASURE( 1.000000000000000082E-05 ), #47711, 'distance_accuracy_value', 'NONE');
#4638 = CARTESIAN_POINT ( 'NONE',  ( 10.00000000000000000, 41.19522573413826194, -65.64334221924865176 ) ) ;
#4639 = ORIENTED_EDGE ( 'NONE', *, *, #47082, .T. ) ;
#4640 = DIRECTION ( 'NONE',  ( 0.000000000000000000, 0.000000000000000000, 1.000000000000000000 ) ) ;
#4641 = EDGE_CURVE ( 'NONE', #34700, #41319, #6342, .T. ) ;
#4642 = DIRECTION ( 'NONE',  ( 0.000000000000000000, 0.000000000000000000, 1.000000000000000000 ) ) ;
#4643 = ORIENTED_EDGE ( 'NONE', *, *, #44488, .T. ) ;
#4644 = EDGE_CURVE ( 'NONE', #46875, #27937, #32165, .T. ) ;
#4645 = EDGE_CURVE ( 'NONE', #41493, #45717, #46764, .T. ) ;
#4646 = ADVANCED_FACE ( 'NONE', ( #28382 ), #29769, .T. ) ;
#4647 = DIRECTION ( 'NONE',  ( -1.000000000000000000, 0.000000000000000000, 0.000000000000000000 ) ) ;
#4648 = ORIENTED_EDGE ( 'NONE', *, *, #12597, .F. ) ;
#4649 = ORIENTED_EDGE ( 'NONE', *, *, #17498, .T. ) ;
#4650 = VERTEX_POINT ( 'NONE', #6360 ) ;
#4651 = EDGE_CURVE ( 'NONE', #45971, #30819, #5636, .T. ) ;
#4652 = ORIENTED_EDGE ( 'NONE', *, *, #25102, .F. ) ;
#4653 = AXIS2_PLACEMENT_3D ( 'NONE', #30400, #45310, #41903 ) ;
#4654 = DIRECTION ( 'NONE',  ( -1.000000000000000000, 0.000000000000000000, -0.000000000000000000 ) ) ;
#4655 = ORIENTED_EDGE ( 'NONE', *, *, #21828, .F. ) ;
#4656 = ORIENTED_EDGE ( 'NONE', *, *, #26930, .F. ) ;
#4657 = LINE ( 'NONE', #4894, #479 ) ;
#4658 = ORIENTED_EDGE ( 'NONE', *, *, #660, .T. ) ;
#4659 = CARTESIAN_POINT ( 'NONE',  ( 0.000000000000000000, -55.38113227695820484, 54.21277698773656084 ) ) ;
#4660 = ORIENTED_EDGE ( 'NONE', *, *, #13597, .T. ) ;
#4661 = CIRCLE ( 'NONE', #26546, 15.99999999999999822 ) ;
#4662 = ADVANCED_FACE ( 'NONE', ( #6596 ), #10022, .T. ) ;
#4663 = DIRECTION ( 'NONE',  ( 0.000000000000000000, 0.000000000000000000, 1.000000000000000000 ) ) ;
#4664 = LINE ( 'NONE', #26701, #18897 ) ;
#4665 = ORIENTED_EDGE ( 'NONE', *, *, #41445, .F. ) ;
#4666 = DIRECTION ( 'NONE',  ( -1.000000000000000000, 0.000000000000000000, 0.000000000000000000 ) ) ;
#4667 = EDGE_LOOP ( 'NONE', ( #12438, #5813, #8662, #5432 ) ) ;
#4669 = ORIENTED_EDGE ( 'NONE', *, *, #20115, .F. ) ;
#4668 = DIRECTION ( 'NONE',  ( 1.000000000000000000, 0.000000000000000000, 0.000000000000000000 ) ) ;
#4670 = DIRECTION ( 'NONE',  ( -1.000000000000000000, -0.000000000000000000, 0.000000000000000000 ) ) ;
#4671 = ORIENTED_EDGE ( 'NONE', *, *, #42094, .F. ) ;
#4672 = DIRECTION ( 'NONE',  ( 0.000000000000000000, 0.000000000000000000, 1.000000000000000000 ) ) ;
#4673 = ORIENTED_EDGE ( 'NONE', *, *, #24767, .F. ) ;
#4674 = VECTOR ( 'NONE', #30671, 1000.000000000000000 ) ;
#4675 = ORIENTED_EDGE ( 'NONE', *, *, #17689, .F. ) ;
#4676 = DIRECTION ( 'NONE',  ( 1.000000000000000000, 0.000000000000000000, 0.000000000000000000 ) ) ;
#4677 = CYLINDRICAL_SURFACE ( 'NONE', #38793, 31.99999999999998579 ) ;
#4678 = EDGE_LOOP ( 'NONE', ( #10562, #18332, #9865, #38379 ) ) ;
#4679 = DIRECTION ( 'NONE',  ( -0.000000000000000000, -0.000000000000000000, -1.000000000000000000 ) ) ;
#4680 = PLANE ( 'NONE',  #7907 ) ;
#4681 = FACE_OUTER_BOUND ( 'NONE', #41157, .T. ) ;
#4682 = DIRECTION ( 'NONE',  ( 1.000000000000000000, 0.000000000000000000, 0.000000000000000000 ) ) ;
#4683 = DIRECTION ( 'NONE',  ( -1.000000000000000000, 0.000000000000000000, 0.000000000000000000 ) ) ;
#4684 = FACE_BOUND ( 'NONE', #4938, .T. ) ;
#4685 = EDGE_CURVE ( 'NONE', #15795, #17381, #8704, .T. ) ;
#4686 = CARTESIAN_POINT ( 'NONE',  ( -3.000000000000000000, -13.04903810567647682, -19.60159698893442481 ) ) ;
#4687 = LINE ( 'NONE', #34530, #27181 ) ;
#4688 = DIRECTION ( 'NONE',  ( -1.000000000000000000, 0.000000000000000000, 0.000000000000000000 ) ) ;
#4689 = ORIENTED_EDGE ( 'NONE', *, *, #21256, .F. ) ;
#4690 = EDGE_CURVE ( 'NONE', #19610, #31364, #48373, .T. ) ;
#4691 = DIRECTION ( 'NONE',  ( 0.000000000000000000, 0.6691306063588570163, -0.7431448254773953543 ) ) ;
#4692 = CARTESIAN_POINT ( 'NONE',  ( -3.000000000000000000, 0.000000000000000000, 0.000000000000000000 ) ) ;
#4693 = DIRECTION ( 'NONE',  ( -1.000000000000000000, 0.000000000000000000, -0.000000000000000000 ) ) ;
#4694 = FACE_OUTER_BOUND ( 'NONE', #26874, .T. ) ;
#4695 = EDGE_CURVE ( 'NONE', #31823, #8701, #43099, .T. ) ;
#4696 = ORIENTED_EDGE ( 'NONE', *, *, #42211, .F. ) ;
#4697 = AXIS2_PLACEMENT_3D ( 'NONE', #24961, #3401, #21541 ) ;
#4698 = DIRECTION ( 'NONE',  ( 0.000000000000000000, -0.9510565162951565288, 0.3090169943749383474 ) ) ;
#4699 = VECTOR ( 'NONE', #46136, 1000.000000000000000 ) ;
#4700 = ORIENTED_EDGE ( 'NONE', *, *, #30300, .T. ) ;
#4701 = CARTESIAN_POINT ( 'NONE',  ( 10.00000000000000000, -35.95386929396264009, 10.96151621346475658 ) ) ;
#4702 = VECTOR ( 'NONE', #22291, 1000.000000000000000 ) ;
#4703 = ITEM_DEFINED_TRANSFORMATION ( 'NONE', 'NONE', #4580,  #11636 ) ;
#4704 = DIRECTION ( 'NONE',  ( -1.000000000000000000, -0.000000000000000000, 0.000000000000000000 ) ) ;
#4705 = ORIENTED_EDGE ( 'NONE', *, *, #12030, .T. ) ;
#4706 = EDGE_CURVE ( 'NONE', #45468, #37953, #36830, .T. ) ;
#4707 = EDGE_CURVE ( 'NONE', #44212, #1265, #7741, .T. ) ;
#4708 = CIRCLE ( 'NONE', #4741, 77.49899999999999523 ) ;
#4709 = AXIS2_PLACEMENT_3D ( 'NONE', #2731, #40195, #6892 ) ;
#4710 = DIRECTION ( 'NONE',  ( 0.000000000000000000, -0.8660254037844427044, -0.4999999999999931166 ) ) ;
#4711 = ORIENTED_EDGE ( 'NONE', *, *, #17097, .T. ) ;
#4712 = ADVANCED_FACE ( 'NONE', ( #11180 ), #12161, .T. ) ;
#4713 = CARTESIAN_POINT ( 'NONE',  ( 11.99999999999999822, 15.33399622253600647, -80.55351364060571484 ) ) ;
#4714 = ORIENTED_EDGE ( 'NONE', *, *, #35231, .F. ) ;
#4715 = LINE ( 'NONE', #31405, #16439 ) ;
#4717 = VERTEX_POINT ( 'NONE', #7970 ) ;
#4716 = FACE_OUTER_BOUND ( 'NONE', #20484, .T. ) ;
#4718 = VERTEX_POINT ( 'NONE', #3832 ) ;
#4719 = DIRECTION ( 'NONE',  ( 0.000000000000000000, 0.000000000000000000, 1.000000000000000000 ) ) ;
#4720 = DIRECTION ( 'NONE',  ( -0.9781476007338042455, -0.2079116908177664758, 0.000000000000000000 ) ) ;
#4721 = DIRECTION ( 'NONE',  ( 0.000000000000000000, 0.9876883405951382144, -0.1564344650402276493 ) ) ;
#4722 = CIRCLE ( 'NONE', #30518, 37.49900000000000233 ) ;
#4723 = DIRECTION ( 'NONE',  ( 1.000000000000000000, 0.000000000000000000, 0.000000000000000000 ) ) ;
#4724 = ORIENTED_EDGE ( 'NONE', *, *, #38571, .T. ) ;
#4725 = VECTOR ( 'NONE', #27484, 1000.000000000000000 ) ;
#4726 = DIRECTION ( 'NONE',  ( -1.000000000000000000, 0.000000000000000000, 0.000000000000000000 ) ) ;
#4727 = ORIENTED_EDGE ( 'NONE', *, *, #42945, .F. ) ;
#4728 = EDGE_LOOP ( 'NONE', ( #19114, #31430, #37216, #40262 ) ) ;
#4729 = DIRECTION ( 'NONE',  ( -1.000000000000000000, -0.000000000000000000, 0.000000000000000000 ) ) ;
#4730 = CIRCLE ( 'NONE', #3138, 77.49899999999999523 ) ;
#4731 = ORIENTED_EDGE ( 'NONE', *, *, #33585, .F. ) ;
#4732 = CIRCLE ( 'NONE', #39924, 82.00000000000000000 ) ;
#4733 = CARTESIAN_POINT ( 'NONE',  ( 10.00000000000000000, 75.54627589209943039, 17.28742895386112721 ) ) ;
#4734 = CARTESIAN_POINT ( 'NONE',  ( 11.99999999999999822, -71.91182617369207719, 28.89263327155721228 ) ) ;
#4735 = CARTESIAN_POINT ( 'NONE',  ( 0.000000000000000000, -12.26510123303234501, -35.53030884539098366 ) ) ;
#4736 = EDGE_LOOP ( 'NONE', ( #6332, #5617, #16245, #14178 ) ) ;
#4737 = CARTESIAN_POINT ( 'NONE',  ( 10.00000000000000000, 63.97538442413425486, 51.29473840253247374 ) ) ;
#4738 = CYLINDRICAL_SURFACE ( 'NONE', #13548, 77.49899999999999523 ) ;
#4739 = VECTOR ( 'NONE', #1727, 1000.000000000000000 ) ;
#4740 = CARTESIAN_POINT ( 'NONE',  ( 5.000000000000000000, 44.99326035066149387, -68.55367621811095091 ) ) ;
#4741 = AXIS2_PLACEMENT_3D ( 'NONE', #24072, #34572, #31428 ) ;
#4742 = CARTESIAN_POINT ( 'NONE',  ( 10.00000000000000000, 0.000000000000000000, 0.000000000000000000 ) ) ;
#4743 = DIRECTION ( 'NONE',  ( 1.000000000000000000, 0.000000000000000000, 0.000000000000000000 ) ) ;
#4744 = EDGE_CURVE ( 'NONE', #44883, #43819, #23554, .T. ) ;
#4745 = AXIS2_PLACEMENT_3D ( 'NONE', #5639, #1979, #16895 ) ;
#4746 = DIRECTION ( 'NONE',  ( -0.000000000000000000, 0.4999999999999919509, 0.8660254037844432595 ) ) ;
#4747 = SURFACE_STYLE_USAGE ( .BOTH. , #9610 ) ;
#4748 = CYLINDRICAL_SURFACE ( 'NONE', #26343, 77.49899999999999523 ) ;
#4749 = EDGE_CURVE ( 'NONE', #27075, #18133, #68, .T. ) ;
#4750 = DIRECTION ( 'NONE',  ( 0.000000000000000000, 0.000000000000000000, 1.000000000000000000 ) ) ;
#4751 = FACE_OUTER_BOUND ( 'NONE', #19940, .T. ) ;
#4752 = EDGE_CURVE ( 'NONE', #38891, #4419, #45670, .T. ) ;
#4753 = VERTEX_POINT ( 'NONE', #30021 ) ;
#4754 = ORIENTED_EDGE ( 'NONE', *, *, #243, .F. ) ;
#4755 = DIRECTION ( 'NONE',  ( -1.000000000000000000, 0.000000000000000000, -0.000000000000000000 ) ) ;
#4756 = CARTESIAN_POINT ( 'NONE',  ( -25.50183398199384754, -112.6408924756582053, 5.500000000000000000 ) ) ;
#4757 = VERTEX_POINT ( 'NONE', #22908 ) ;
#4758 = VERTEX_POINT ( 'NONE', #8463 ) ;
#4759 = LINE ( 'NONE', #46125, #29928 ) ;
#4760 = ORIENTED_EDGE ( 'NONE', *, *, #27976, .T. ) ;
#4761 = ORIENTED_EDGE ( 'NONE', *, *, #26148, .T. ) ;
#4762 = EDGE_CURVE ( 'NONE', #28804, #42832, #16063, .T. ) ;
#4763 = EDGE_CURVE ( 'NONE', #18839, #42776, #31380, .T. ) ;
#4764 = AXIS2_PLACEMENT_3D ( 'NONE', #30315, #15610, #33722 ) ;
#4765 = ADVANCED_FACE ( 'NONE', ( #34166 ), #639, .F. ) ;
#4766 = ORIENTED_EDGE ( 'NONE', *, *, #19000, .F. ) ;
#4767 = AXIS2_PLACEMENT_3D ( 'NONE', #336, #41701, #7451 ) ;
#4768 = AXIS2_PLACEMENT_3D ( 'NONE', #20539, #16171, #24457 ) ;
#4769 = ORIENTED_EDGE ( 'NONE', *, *, #28237, .F. ) ;
#4770 = ORIENTED_EDGE ( 'NONE', *, *, #17122, .T. ) ;
#4771 = ORIENTED_EDGE ( 'NONE', *, *, #28519, .F. ) ;
#4772 = ORIENTED_EDGE ( 'NONE', *, *, #2059, .T. ) ;
#4773 = CIRCLE ( 'NONE', #32146, 37.49900000000001654 ) ;
#4774 = AXIS2_PLACEMENT_3D ( 'NONE', #19582, #42859, #23284 ) ;
#4775 = EDGE_CURVE ( 'NONE', #15212, #15797, #37613, .T. ) ;
#4776 = DIRECTION ( 'NONE',  ( 0.000000000000000000, 0.000000000000000000, 1.000000000000000000 ) ) ;
#4777 = AXIS2_PLACEMENT_3D ( 'NONE', #25179, #21528, #14906 ) ;
#4778 = CARTESIAN_POINT ( 'NONE',  ( 0.000000000000000000, -75.11764819372145041, -2.946379043147127064 ) ) ;
#4779 = CARTESIAN_POINT ( 'NONE',  ( 0.000000000000000000, 0.000000000000000000, 0.000000000000000000 ) ) ;
#4780 = EDGE_LOOP ( 'NONE', ( #43136, #47578, #17837, #18162 ) ) ;
#4781 = CYLINDRICAL_SURFACE ( 'NONE', #36755, 42.00000000000000000 ) ;
#4782 = ORIENTED_EDGE ( 'NONE', *, *, #30065, .F. ) ;
#4783 = ORIENTED_EDGE ( 'NONE', *, *, #37222, .F. ) ;
#4784 = DIRECTION ( 'NONE',  ( -1.000000000000000000, 0.000000000000000000, -0.000000000000000000 ) ) ;
#4785 = DIRECTION ( 'NONE',  ( 0.000000000000000000, 0.000000000000000000, 1.000000000000000000 ) ) ;
#4786 = DIRECTION ( 'NONE',  ( 0.000000000000000000, -0.5877852522924624790, -0.8090169943749550008 ) ) ;
#4787 = ORIENTED_EDGE ( 'NONE', *, *, #19891, .F. ) ;
#4788 = ORIENTED_EDGE ( 'NONE', *, *, #44015, .T. ) ;
#4789 = CARTESIAN_POINT ( 'NONE',  ( 2.117611129180199558, -93.54218975225703048, 5.500000000000000000 ) ) ;
#4790 = VERTEX_POINT ( 'NONE', #44952 ) ;
#4791 = DIRECTION ( 'NONE',  ( -1.000000000000000000, 0.000000000000000000, 0.000000000000000000 ) ) ;
#4792 = CARTESIAN_POINT ( 'NONE',  ( 10.00000000000000000, -9.188173127307592836, 40.98264845739746676 ) ) ;
#4793 = DIRECTION ( 'NONE',  ( 0.000000000000000000, -0.2079116908177664480, -0.9781476007338041345 ) ) ;
#4794 = CARTESIAN_POINT ( 'NONE',  ( 15.00000000000000000, -4.261787119644963262, 26.19803753235780164 ) ) ;
#4795 = DIRECTION ( 'NONE',  ( 0.000000000000000000, 0.000000000000000000, 1.000000000000000000 ) ) ;
#4796 = CARTESIAN_POINT ( 'NONE',  ( 12.49999999999999645, 1.530808498934191127E-15, -43.79999999999998295 ) ) ;
#4797 = CARTESIAN_POINT ( 'NONE',  ( 10.00000000000000000, -58.39081064771787766, 50.95692526931307498 ) ) ;
#4798 = LINE ( 'NONE', #35129, #48438 ) ;
#4799 = LINE ( 'NONE', #35130, #20674 ) ;
#4800 = VECTOR ( 'NONE', #6678, 1000.000000000000227 ) ;
#4801 = CARTESIAN_POINT ( 'NONE',  ( 11.99999999999999822, -73.44644590900043113, -24.73286445877782924 ) ) ;
#4802 = CARTESIAN_POINT ( 'NONE',  ( 6.000000000000000000, -76.69515212746036070, 29.01471420065536932 ) ) ;
#4803 = EDGE_LOOP ( 'NONE', ( #16943, #41206, #15984, #1822 ) ) ;
#4804 = DIRECTION ( 'NONE',  ( 0.000000000000000000, -0.9876883405951359940, -0.1564344650402420822 ) ) ;
#4805 = EDGE_CURVE ( 'NONE', #1310, #33968, #6381, .T. ) ;
#4806 = DIRECTION ( 'NONE',  ( 0.000000000000000000, 0.8090169943749486725, -0.5877852522924713607 ) ) ;
#4807 = CARTESIAN_POINT ( 'NONE',  ( 10.00000000000000000, 0.000000000000000000, 0.000000000000000000 ) ) ;
#4808 = DIRECTION ( 'NONE',  ( 0.000000000000000000, 0.7604059656000276002, 0.6494480483301876550 ) ) ;
#4809 = EDGE_CURVE ( 'NONE', #21783, #19662, #42010, .T. ) ;
#4810 = EDGE_CURVE ( 'NONE', #31737, #747, #25122, .T. ) ;
#4811 = VECTOR ( 'NONE', #20026, 1000.000000000000000 ) ;
#4812 = CARTESIAN_POINT ( 'NONE',  ( 11.99999999999999822, 34.94270380257639630, 74.18225833017902460 ) ) ;
#4813 = ADVANCED_FACE ( 'NONE', ( #7512 ), #26351, .T. ) ;
#4814 = CARTESIAN_POINT ( 'NONE',  ( 0.000000000000000000, 0.000000000000000000, 0.000000000000000000 ) ) ;
#4815 = DIRECTION ( 'NONE',  ( -0.000000000000000000, -0.000000000000000000, -1.000000000000000000 ) ) ;
#4817 = ADVANCED_FACE ( 'NONE', ( #45194 ), #11661, .T. ) ;
#4816 = ORIENTED_EDGE ( 'NONE', *, *, #37750, .F. ) ;
#4818 = AXIS2_PLACEMENT_3D ( 'NONE', #29478, #14063, #6482 ) ;
#4819 = AXIS2_PLACEMENT_3D ( 'NONE', #9293, #31594, #16175 ) ;
#4820 =( LENGTH_UNIT ( ) NAMED_UNIT ( * ) SI_UNIT ( .MILLI., .METRE. ) );
#4821 = CARTESIAN_POINT ( 'NONE',  ( -6.112675177960399608, -145.7853679859090903, 2.500000000000000000 ) ) ;
#4822 = VERTEX_POINT ( 'NONE', #45420 ) ;
#4823 = EDGE_CURVE ( 'NONE', #34476, #39757, #10279, .T. ) ;
#4824 = ORIENTED_EDGE ( 'NONE', *, *, #6916, .T. ) ;
#4825 = EDGE_CURVE ( 'NONE', #42048, #34678, #20935, .T. ) ;
#4826 = ORIENTED_EDGE ( 'NONE', *, *, #37000, .F. ) ;
#4827 = LINE ( 'NONE', #19731, #28078 ) ;
#4828 = ORIENTED_EDGE ( 'NONE', *, *, #32231, .F. ) ;
#4829 = ORIENTED_EDGE ( 'NONE', *, *, #1819, .F. ) ;
#4830 = AXIS2_PLACEMENT_3D ( 'NONE', #34401, #44966, #41068 ) ;
#4831 = EDGE_CURVE ( 'NONE', #28609, #18434, #20202, .T. ) ;
#4832 = CARTESIAN_POINT ( 'NONE',  ( 10.00000000000000000, 39.47590169984845687, 71.87247863392427405 ) ) ;
#4833 = DIRECTION ( 'NONE',  ( 0.000000000000000000, 0.000000000000000000, 1.000000000000000000 ) ) ;
#4834 = ORIENTED_EDGE ( 'NONE', *, *, #19727, .F. ) ;
#4835 = ORIENTED_EDGE ( 'NONE', *, *, #32063, .T. ) ;
#4836 = COLOUR_RGB ( '', 0.66274510, 0.83137255, 0.94901961) ;
#4837 = VECTOR ( 'NONE', #6489, 1000.000000000000000 ) ;
#4838 = CARTESIAN_POINT ( 'NONE',  ( -3.000000000000000000, 0.000000000000000000, 0.000000000000000000 ) ) ;
#4840 = EDGE_LOOP ( 'NONE', ( #13629, #18206, #12768, #27217 ) ) ;
#4839 = DIRECTION ( 'NONE',  ( 1.000000000000000000, 0.000000000000000000, 0.000000000000000000 ) ) ;
#4841 = EDGE_CURVE ( 'NONE', #9394, #23424, #38828, .T. ) ;
#4842 = FACE_OUTER_BOUND ( 'NONE', #29012, .T. ) ;
#4843 = ORIENTED_EDGE ( 'NONE', *, *, #30448, .F. ) ;
#4844 = ORIENTED_EDGE ( 'NONE', *, *, #8392, .F. ) ;
#4845 = DIRECTION ( 'NONE',  ( 0.000000000000000000, 0.9135454576426005335, -0.4067366430758009299 ) ) ;
#4846 = ORIENTED_EDGE ( 'NONE', *, *, #3596, .F. ) ;
#4847 = ORIENTED_EDGE ( 'NONE', *, *, #29512, .F. ) ;
#4848 = PLANE ( 'NONE',  #20460 ) ;
#4849 = DIRECTION ( 'NONE',  ( 0.000000000000000000, -0.3090169943749350168, -0.9510565162951576390 ) ) ;
#4850 = VECTOR ( 'NONE', #8509, 1000.000000000000000 ) ;
#4851 = VERTEX_POINT ( 'NONE', #27555 ) ;
#4852 = DIRECTION ( 'NONE',  ( 0.000000000000000000, 0.000000000000000000, -1.000000000000000000 ) ) ;
#4853 = DIRECTION ( 'NONE',  ( -1.000000000000000000, 0.000000000000000000, 0.000000000000000000 ) ) ;
#4854 = CYLINDRICAL_SURFACE ( 'NONE', #28348, 77.49899999999999523 ) ;
#4855 = VERTEX_POINT ( 'NONE', #23628 ) ;
#4856 = VERTEX_POINT ( 'NONE', #42483 ) ;
#4857 =( LENGTH_UNIT ( ) NAMED_UNIT ( * ) SI_UNIT ( .MILLI., .METRE. ) );
#4858 = CARTESIAN_POINT ( 'NONE',  ( 10.00000000000000000, -14.66109333815410487, -73.73191006444587003 ) ) ;
#4859 = ORIENTED_EDGE ( 'NONE', *, *, #7422, .T. ) ;
#4860 = ADVANCED_FACE ( 'NONE', ( #38575 ), #20433, .F. ) ;
#4861 = FACE_OUTER_BOUND ( 'NONE', #35950, .T. ) ;
#4862 = ORIENTED_EDGE ( 'NONE', *, *, #48360, .T. ) ;
#4863 = VECTOR ( 'NONE', #45988, 1000.000000000000000 ) ;
#4864 = CARTESIAN_POINT ( 'NONE',  ( 10.00000000000000000, -6.736453364083292428, -36.88895765772640800 ) ) ;
#4865 = CARTESIAN_POINT ( 'NONE',  ( 10.00000000000000000, -29.81001611431024756, 22.74946021919122785 ) ) ;
#4866 = CARTESIAN_POINT ( 'NONE',  ( 10.00000000000000000, 0.000000000000000000, 0.000000000000000000 ) ) ;
#4867 = CARTESIAN_POINT ( 'NONE',  ( 6.000000000000000000, 16.65972982745045528, -80.28980883073738539 ) ) ;
#4868 = EDGE_CURVE ( 'NONE', #26745, #26652, #19551, .T. ) ;
#4869 = DIRECTION ( 'NONE',  ( 1.000000000000000000, 0.000000000000000000, 0.000000000000000000 ) ) ;
#4871 = AXIS2_PLACEMENT_3D ( 'NONE', #16549, #43695, #2815 ) ;
#4870 = CARTESIAN_POINT ( 'NONE',  ( -13.05994868825747446, -139.5943292883446532, -5.500000000000000000 ) ) ;
#4872 = DIRECTION ( 'NONE',  ( -1.000000000000000000, 0.000000000000000000, 0.000000000000000000 ) ) ;
#4873 = DIRECTION ( 'NONE',  ( -1.000000000000000000, 0.000000000000000000, 0.000000000000000000 ) ) ;
#4874 = ADVANCED_FACE ( 'NONE', ( #5040 ), #16536, .T. ) ;
#4875 = AXIS2_PLACEMENT_3D ( 'NONE', #9527, #5391, #9065 ) ;
#4876 = FACE_OUTER_BOUND ( 'NONE', #26450, .T. ) ;
#4877 = AXIS2_PLACEMENT_3D ( 'NONE', #30950, #1321, #12576 ) ;
#4878 = EDGE_LOOP ( 'NONE', ( #45223, #33983, #40826, #789 ) ) ;
#4879 = DIRECTION ( 'NONE',  ( 1.000000000000000000, 0.000000000000000000, 0.000000000000000000 ) ) ;
#4880 = VECTOR ( 'NONE', #8257, 1000.000000000000000 ) ;
#4881 = DIRECTION ( 'NONE',  ( 0.000000000000000000, 0.000000000000000000, -1.000000000000000000 ) ) ;
#4882 = CYLINDRICAL_SURFACE ( 'NONE', #1932, 16.00000000000000000 ) ;
#4883 = ORIENTED_EDGE ( 'NONE', *, *, #17913, .F. ) ;
#4884 = VERTEX_POINT ( 'NONE', #1856 ) ;
#4885 = DIRECTION ( 'NONE',  ( 0.000000000000000000, 0.2334453638559058908, -0.9723699203976764460 ) ) ;
#4886 = ORIENTED_EDGE ( 'NONE', *, *, #41076, .F. ) ;
#4887 = ORIENTED_EDGE ( 'NONE', *, *, #35298, .T. ) ;
#4888 = ORIENTED_EDGE ( 'NONE', *, *, #19613, .T. ) ;
#4889 = EDGE_LOOP ( 'NONE', ( #10513, #1409, #16048, #42720 ) ) ;
#4890 = ORIENTED_EDGE ( 'NONE', *, *, #7931, .T. ) ;
#4891 = AXIS2_PLACEMENT_3D ( 'NONE', #39505, #47777, #5977 ) ;
#4892 = DIRECTION ( 'NONE',  ( -1.000000000000000000, -0.000000000000000000, 0.000000000000000000 ) ) ;
#4893 = ORIENTED_EDGE ( 'NONE', *, *, #9828, .T. ) ;
#4894 = CARTESIAN_POINT ( 'NONE',  ( 10.00000000000000000, 33.80338159004307386, -16.23288003029461279 ) ) ;
#4895 = ORIENTED_EDGE ( 'NONE', *, *, #41729, .F. ) ;
#4896 = CARTESIAN_POINT ( 'NONE',  ( 12.50000000000000000, -132.5000000000000000, 2.500000000000000000 ) ) ;
#4897 = CIRCLE ( 'NONE', #33829, 31.99999999999998579 ) ;
#4898 = CARTESIAN_POINT ( 'NONE',  ( 0.000000000000000000, 0.000000000000000000, 0.000000000000000000 ) ) ;
#4899 = CARTESIAN_POINT ( 'NONE',  ( 0.000000000000000000, -13.04903810567647682, -19.60159698893442126 ) ) ;
#4900 = AXIS2_PLACEMENT_3D ( 'NONE', #5240, #42686, #13531 ) ;
#4901 = ORIENTED_EDGE ( 'NONE', *, *, #12488, .T. ) ;
#4902 = FACE_OUTER_BOUND ( 'NONE', #44494, .T. ) ;
#4903 = ORIENTED_EDGE ( 'NONE', *, *, #35294, .T. ) ;
#4904 = DIRECTION ( 'NONE',  ( 0.000000000000000000, 0.000000000000000000, 1.000000000000000000 ) ) ;
#4905 = EDGE_CURVE ( 'NONE', #3151, #13690, #7938, .T. ) ;
#4906 = CARTESIAN_POINT ( 'NONE',  ( 10.00000000000000000, -37.22597642581161637, 5.202137450156258502 ) ) ;
#4907 = VERTEX_POINT ( 'NONE', #2097 ) ;
#4908 = VECTOR ( 'NONE', #42486, 1000.000000000000000 ) ;
#4909 = DIRECTION ( 'NONE',  ( -1.000000000000000000, 0.000000000000000000, 0.000000000000000000 ) ) ;
#4910 = ORIENTED_EDGE ( 'NONE', *, *, #32592, .F. ) ;
#4911 = VERTEX_POINT ( 'NONE', #6018 ) ;
#4912 = EDGE_CURVE ( 'NONE', #38297, #11714, #46398, .T. ) ;
#4913 = CARTESIAN_POINT ( 'NONE',  ( 0.000000000000000000, -37.22597642581153821, -5.202137450156795850 ) ) ;
#4914 = CYLINDRICAL_SURFACE ( 'NONE', #33220, 31.99999999999999289 ) ;
#4915 = VECTOR ( 'NONE', #4296, 1000.000000000000000 ) ;
#4916 = CYLINDRICAL_SURFACE ( 'NONE', #44094, 77.49899999999999523 ) ;
#4917 = DIRECTION ( 'NONE',  ( 0.000000000000000000, 0.4539904997395413644, 0.8910065241883706744 ) ) ;
#4918 = DIRECTION ( 'NONE',  ( 0.000000000000000000, 0.000000000000000000, 1.000000000000000000 ) ) ;
#4919 = EDGE_CURVE ( 'NONE', #46849, #14154, #12625, .T. ) ;
#4920 = FACE_OUTER_BOUND ( 'NONE', #15500, .T. ) ;
#4921 = CARTESIAN_POINT ( 'NONE',  ( 10.00000000000000000, -77.19088730480518734, -6.903761155838607166 ) ) ;
#4922 = DIRECTION ( 'NONE',  ( 0.000000000000000000, 0.8526401643540897357, 0.5224985647159527957 ) ) ;
#4923 = EDGE_LOOP ( 'NONE', ( #21009, #44884, #9654, #329 ) ) ;
#4924 = DIRECTION ( 'NONE',  ( 0.000000000000000000, 0.000000000000000000, 1.000000000000000000 ) ) ;
#4925 = DIRECTION ( 'NONE',  ( 0.000000000000000000, -0.9510565162951510887, 0.3090169943749551673 ) ) ;
#4926 = CARTESIAN_POINT ( 'NONE',  ( -12.49999999999999645, 0.000000000000000000, 125.0000000000000000 ) ) ;
#4927 = EDGE_CURVE ( 'NONE', #45521, #32527, #31966, .T. ) ;
#4928 = ADVANCED_FACE ( 'NONE', ( #5519 ), #42972, .T. ) ;
#4929 = DIRECTION ( 'NONE',  ( 1.000000000000000000, 0.000000000000000000, 0.000000000000000000 ) ) ;
#4930 = DIRECTION ( 'NONE',  ( -1.000000000000000000, 0.000000000000000000, -0.000000000000000000 ) ) ;
#4932 = CIRCLE ( 'NONE', #18954, 31.99999999999999645 ) ;
#4931 = FILL_AREA_STYLE ('',( #45556 ) ) ;
#4933 = LINE ( 'NONE', #19850, #29587 ) ;
#4934 = ORIENTED_EDGE ( 'NONE', *, *, #36530, .T. ) ;
#4935 = AXIS2_PLACEMENT_3D ( 'NONE', #1508, #16671, #4691 ) ;
#4936 = VERTEX_POINT ( 'NONE', #28044 ) ;
#4937 = CARTESIAN_POINT ( 'NONE',  ( 0.000000000000000000, 0.000000000000000000, 0.000000000000000000 ) ) ;
#4938 = EDGE_LOOP ( 'NONE', ( #16511, #37210 ) ) ;
#4939 = LINE ( 'NONE', #19858, #31541 ) ;
#4940 = AXIS2_PLACEMENT_3D ( 'NONE', #41287, #18985, #11903 ) ;
#4941 = VECTOR ( 'NONE', #27372, 1000.000000000000000 ) ;
#4943 = EDGE_CURVE ( 'NONE', #409, #47967, #28268, .T. ) ;
#4942 = ITEM_DEFINED_TRANSFORMATION ( 'NONE', 'NONE', #43645,  #11636 ) ;
#4944 = DIRECTION ( 'NONE',  ( 0.000000000000000000, 0.000000000000000000, 1.000000000000000000 ) ) ;
#4945 = ORIENTED_EDGE ( 'NONE', *, *, #31457, .F. ) ;
#4946 = VECTOR ( 'NONE', #47822, 1000.000000000000000 ) ;
#4947 = CIRCLE ( 'NONE', #47152, 16.00000000000000000 ) ;
#4948 = EDGE_LOOP ( 'NONE', ( #7569, #6269, #20759, #8147 ) ) ;
#4949 = LINE ( 'NONE', #34802, #21478 ) ;
#4950 = ORIENTED_EDGE ( 'NONE', *, *, #36234, .T. ) ;
#4951 = CARTESIAN_POINT ( 'NONE',  ( 0.000000000000000000, 0.000000000000000000, 0.000000000000000000 ) ) ;
#4952 = AXIS2_PLACEMENT_3D ( 'NONE', #8317, #33527, #19545 ) ;
#4953 = EDGE_CURVE ( 'NONE', #28743, #27429, #29743, .T. ) ;
#4954 = DIRECTION ( 'NONE',  ( -1.000000000000000000, -0.000000000000000000, -0.000000000000000000 ) ) ;
#4955 = CARTESIAN_POINT ( 'NONE',  ( 0.000000000000000000, -30.41916302227164337, 71.27951684758015460 ) ) ;
#4956 = ORIENTED_EDGE ( 'NONE', *, *, #315, .F. ) ;
#4957 = DIRECTION ( 'NONE',  ( 0.000000000000000000, 0.000000000000000000, 1.000000000000000000 ) ) ;
#4958 = EDGE_CURVE ( 'NONE', #16116, #11391, #4730, .T. ) ;
#4959 = ORIENTED_EDGE ( 'NONE', *, *, #46112, .T. ) ;
#4960 = EDGE_CURVE ( 'NONE', #5392, #47811, #45923, .T. ) ;
#4961 = DIRECTION ( 'NONE',  ( 1.000000000000000000, -0.000000000000000000, -0.000000000000000000 ) ) ;
#4962 = CARTESIAN_POINT ( 'NONE',  ( 24.94940289813197509, -237.3777120880564553, -5.500000000000000000 ) ) ;
#4963 = DIRECTION ( 'NONE',  ( 1.000000000000000000, 0.000000000000000000, 0.000000000000000000 ) ) ;
#4964 = VECTOR ( 'NONE', #30575, 1000.000000000000000 ) ;
#4966 = ORIENTED_EDGE ( 'NONE', *, *, #11266, .T. ) ;
#4965 = CARTESIAN_POINT ( 'NONE',  ( 12.00000000000000000, -20.55727247249748757, -16.78983467731284662 ) ) ;
#4967 = ORIENTED_EDGE ( 'NONE', *, *, #5434, .F. ) ;
#4968 = CARTESIAN_POINT ( 'NONE',  ( 0.000000000000000000, -3.948201729842038432, -23.21447184625298021 ) ) ;
#4969 = EDGE_LOOP ( 'NONE', ( #15786, #10000, #21340, #1882 ) ) ;
#4970 = VERTEX_POINT ( 'NONE', #42237 ) ;
#4971 = VECTOR ( 'NONE', #21884, 1000.000000000000000 ) ;
#4972 = DIRECTION ( 'NONE',  ( -1.000000000000000000, 0.000000000000000000, 0.000000000000000000 ) ) ;
#4973 = AXIS2_PLACEMENT_3D ( 'NONE', #11179, #26588, #33675 ) ;
#4974 = ORIENTED_EDGE ( 'NONE', *, *, #8970, .T. ) ;
#4975 = DIRECTION ( 'NONE',  ( -0.000000000000000000, -0.3090169943749573878, 0.9510565162951503115 ) ) ;
#4976 = DIRECTION ( 'NONE',  ( -1.000000000000000000, 0.000000000000000000, -0.000000000000000000 ) ) ;
#4977 = CARTESIAN_POINT ( 'NONE',  ( 7.893099573151324044, -11.68370571044642503, 0.000000000000000000 ) ) ;
#4978 = ORIENTED_EDGE ( 'NONE', *, *, #46852, .F. ) ;
#4979 = DIRECTION ( 'NONE',  ( 0.9135454576426004225, 0.4067366430758009854, 0.000000000000000000 ) ) ;
#4980 = EDGE_CURVE ( 'NONE', #9118, #34027, #19957, .T. ) ;
#4981 = DIRECTION ( 'NONE',  ( 0.000000000000000000, 0.8526401643540935105, -0.5224985647159468005 ) ) ;
#4982 = EDGE_CURVE ( 'NONE', #17248, #25278, #37537, .T. ) ;
#4983 = EDGE_CURVE ( 'NONE', #22767, #17326, #44600, .T. ) ;
#4984 = DIRECTION ( 'NONE',  ( 0.000000000000000000, 0.9723699203976773342, -0.2334453638559025601 ) ) ;
#4985 = CARTESIAN_POINT ( 'NONE',  ( 15.00000000000000000, -26.23277895567245466, 4.042438405570107918 ) ) ;
#4986 = DIRECTION ( 'NONE',  ( 0.000000000000000000, 0.9238795325112877377, -0.3826834323650873948 ) ) ;
#4987 = VECTOR ( 'NONE', #40639, 1000.000000000000000 ) ;
#4988 = CIRCLE ( 'NONE', #10425, 31.99999999999998224 ) ;
#4989 = CARTESIAN_POINT ( 'NONE',  ( 0.000000000000000000, -16.65560815589383381, -38.55633173627028754 ) ) ;
#4990 =( LENGTH_UNIT ( ) NAMED_UNIT ( * ) SI_UNIT ( .MILLI., .METRE. ) );
#4991 = PLANE ( 'NONE',  #11503 ) ;
#4992 = CIRCLE ( 'NONE', #7316, 31.99999999999999645 ) ;
#4993 = AXIS2_PLACEMENT_3D ( 'NONE', #35714, #5373, #9510 ) ;
#4994 = CARTESIAN_POINT ( 'NONE',  ( 0.000000000000000000, -37.22597642581153821, 10.79786254984320415 ) ) ;
#4995 = PLANE ( 'NONE',  #11241 ) ;
#4996 = AXIS2_PLACEMENT_3D ( 'NONE', #20125, #20857, #27970 ) ;
#4997 = ORIENTED_EDGE ( 'NONE', *, *, #17969, .T. ) ;
#4998 = PRODUCT_RELATED_PRODUCT_CATEGORY ( 'part', '', ( #9689 ) ) ;
#4999 = CARTESIAN_POINT ( 'NONE',  ( 10.00000000000000000, 28.89263327155850902, -71.91182617369157981 ) ) ;
#5000 = ORIENTED_EDGE ( 'NONE', *, *, #269, .F. ) ;
#5001 = VERTEX_POINT ( 'NONE', #14563 ) ;
#5002 = FACE_OUTER_BOUND ( 'NONE', #22421, .T. ) ;
#5003 = CARTESIAN_POINT ( 'NONE',  ( 11.99999999999999822, 81.90746397400394585, -3.894527615416972566 ) ) ;
#5004 = VERTEX_POINT ( 'NONE', #21653 ) ;
#5005 = AXIS2_PLACEMENT_3D ( 'NONE', #46124, #16501, #31696 ) ;
#5006 = VECTOR ( 'NONE', #23283, 1000.000000000000000 ) ;
#5007 = AXIS2_PLACEMENT_3D ( 'NONE', #39002, #46103, #5237 ) ;
#5008 = AXIS2_PLACEMENT_3D ( 'NONE', #1371, #43203, #34890 ) ;
#5009 = CIRCLE ( 'NONE', #23001, 77.49899999999999523 ) ;
#5010 = ORIENTED_EDGE ( 'NONE', *, *, #46, .F. ) ;
#5011 = ORIENTED_EDGE ( 'NONE', *, *, #2529, .F. ) ;
#5012 = ADVANCED_FACE ( 'NONE', ( #29238 ), #40733, .T. ) ;
#5013 = AXIS2_PLACEMENT_3D ( 'NONE', #5326, #8988, #3687 ) ;
#5014 = AXIS2_PLACEMENT_3D ( 'NONE', #43167, #13542, #9616 ) ;
#5015 = CYLINDRICAL_SURFACE ( 'NONE', #40909, 16.00000000000000000 ) ;
#5016 = AXIS2_PLACEMENT_3D ( 'NONE', #23456, #27387, #42565 ) ;
#5017 = CARTESIAN_POINT ( 'NONE',  ( 0.000000000000000000, 0.000000000000000000, 0.000000000000000000 ) ) ;
#5018 = CIRCLE ( 'NONE', #38656, 77.49899999999999523 ) ;
#5020 = ORIENTED_EDGE ( 'NONE', *, *, #35027, .T. ) ;
#5019 = DIRECTION ( 'NONE',  ( -1.000000000000000000, -0.000000000000000000, 0.000000000000000000 ) ) ;
#5021 = EDGE_CURVE ( 'NONE', #13181, #7846, #34413, .T. ) ;
#5022 = ORIENTED_EDGE ( 'NONE', *, *, #14302, .T. ) ;
#5023 = DIRECTION ( 'NONE',  ( -1.000000000000000000, 0.000000000000000000, 0.000000000000000000 ) ) ;
#5024 = EDGE_CURVE ( 'NONE', #43844, #23166, #2382, .T. ) ;
#5025 = ORIENTED_EDGE ( 'NONE', *, *, #11406, .T. ) ;
#5026 = CIRCLE ( 'NONE', #7411, 31.99999999999999289 ) ;
#5027 = DIRECTION ( 'NONE',  ( 0.000000000000000000, -0.07845909572785224328, 0.9969173337331274087 ) ) ;
#5028 = DIRECTION ( 'NONE',  ( 0.000000000000000000, 0.000000000000000000, 1.000000000000000000 ) ) ;
#5029 = CARTESIAN_POINT ( 'NONE',  ( 15.00000000000000000, 14.60985201121729737, 18.46759930825687235 ) ) ;
#5030 = ORIENTED_EDGE ( 'NONE', *, *, #12839, .F. ) ;
#5031 = ORIENTED_EDGE ( 'NONE', *, *, #16588, .T. ) ;
#5032 = EDGE_LOOP ( 'NONE', ( #37984, #28347, #22364, #39508 ) ) ;
#5033 = DIRECTION ( 'NONE',  ( 0.000000000000000000, 0.2334453638558990629, 0.9723699203976782224 ) ) ;
#5034 = ORIENTED_EDGE ( 'NONE', *, *, #44437, .F. ) ;
#5035 = EDGE_CURVE ( 'NONE', #26639, #46150, #40019, .T. ) ;
#5036 = DIRECTION ( 'NONE',  ( -1.000000000000000000, -0.000000000000000000, -0.000000000000000000 ) ) ;
#5037 = CARTESIAN_POINT ( 'NONE',  ( 11.99999999999999822, -51.02545421589363883, 55.20638768913742922 ) ) ;
#5038 = FACE_OUTER_BOUND ( 'NONE', #46261, .T. ) ;
#5039 = DIRECTION ( 'NONE',  ( -1.000000000000000000, -0.000000000000000000, 0.000000000000000000 ) ) ;
#5040 = FACE_OUTER_BOUND ( 'NONE', #10690, .T. ) ;
#5041 = DIRECTION ( 'NONE',  ( 1.000000000000000000, -0.000000000000000000, -0.000000000000000000 ) ) ;
#5042 = CARTESIAN_POINT ( 'NONE',  ( 10.00000000000000000, 30.84782396557248418, -21.32104025579081252 ) ) ;
#5043 = EDGE_CURVE ( 'NONE', #12792, #27374, #13841, .T. ) ;
#5044 = EDGE_LOOP ( 'NONE', ( #40600, #40480, #20302, #10736 ) ) ;
#5045 = ADVANCED_FACE ( 'NONE', ( #29479 ), #44408, .T. ) ;
#5046 = CARTESIAN_POINT ( 'NONE',  ( 10.00000000000000000, 0.000000000000000000, 0.000000000000000000 ) ) ;
#5047 = DIRECTION ( 'NONE',  ( -1.000000000000000000, 0.000000000000000000, -0.000000000000000000 ) ) ;
#5048 = CYLINDRICAL_SURFACE ( 'NONE', #19703, 37.49900000000000233 ) ;
#5049 = AXIS2_PLACEMENT_3D ( 'NONE', #43091, #31858, #42366 ) ;
#5050 = DIRECTION ( 'NONE',  ( -1.000000000000000000, 0.000000000000000000, 0.000000000000000000 ) ) ;
#5051 = ORIENTED_EDGE ( 'NONE', *, *, #42354, .T. ) ;
#5052 = SURFACE_SIDE_STYLE ('',( #23638 ) ) ;
#5053 = AXIS2_PLACEMENT_3D ( 'NONE', #40769, #31832, #33427 ) ;
#5054 = AXIS2_PLACEMENT_3D ( 'NONE', #23589, #8186, #34355 ) ;
#5055 = DIRECTION ( 'NONE',  ( 0.000000000000000000, 0.000000000000000000, 1.000000000000000000 ) ) ;
#5056 = CIRCLE ( 'NONE', #19080, 77.49900000000000944 ) ;
#5057 = FACE_OUTER_BOUND ( 'NONE', #9709, .T. ) ;
#5058 = DIRECTION ( 'NONE',  ( -0.000000000000000000, -0.6691306063588670083, -0.7431448254773863615 ) ) ;
#5059 = DIRECTION ( 'NONE',  ( -1.000000000000000000, 0.000000000000000000, 0.000000000000000000 ) ) ;
#5060 = FACE_OUTER_BOUND ( 'NONE', #35917, .T. ) ;
#5061 = ADVANCED_FACE ( 'NONE', ( #32896 ), #6961, .T. ) ;
#5062 = ORIENTED_EDGE ( 'NONE', *, *, #20283, .F. ) ;
#5063 = AXIS2_PLACEMENT_3D ( 'NONE', #15071, #10913, #30000 ) ;
#5064 = CIRCLE ( 'NONE', #25336, 16.00000000000000355 ) ;
#5065 = CARTESIAN_POINT ( 'NONE',  ( 11.99999999999999822, -20.41045688087876897, 72.35160999960810102 ) ) ;
#5066 = CYLINDRICAL_SURFACE ( 'NONE', #16258, 82.00000000000000000 ) ;
#5067 = VERTEX_POINT ( 'NONE', #2553 ) ;
#5068 = CIRCLE ( 'NONE', #27632, 42.00000000000000000 ) ;
#5069 = ORIENTED_EDGE ( 'NONE', *, *, #11174, .F. ) ;
#5070 = CARTESIAN_POINT ( 'NONE',  ( 0.000000000000000000, 0.000000000000000000, 0.000000000000000000 ) ) ;
#5071 = CARTESIAN_POINT ( 'NONE',  ( 0.000000000000000000, 0.000000000000000000, 0.000000000000000000 ) ) ;
#5072 = AXIS2_PLACEMENT_3D ( 'NONE', #32900, #14070, #14312 ) ;
#5073 = ORIENTED_EDGE ( 'NONE', *, *, #33269, .F. ) ;
#5074 = VERTEX_POINT ( 'NONE', #36338 ) ;
#5075 = ORIENTED_EDGE ( 'NONE', *, *, #20999, .F. ) ;
#5076 = CARTESIAN_POINT ( 'NONE',  ( 0.000000000000000000, 44.99326035066051332, 68.55367621811160461 ) ) ;
#5077 = ORIENTED_EDGE ( 'NONE', *, *, #23805, .F. ) ;
#5078 = EDGE_LOOP ( 'NONE', ( #33661, #5446, #16805, #18478 ) ) ;
#5079 = VECTOR ( 'NONE', #35197, 1000.000000000000000 ) ;
#5080 = CARTESIAN_POINT ( 'NONE',  ( 5.000000000000002665, -74.18225833017864090, -34.94270380257719211 ) ) ;
#5081 = AXIS2_PLACEMENT_3D ( 'NONE', #41460, #33859, #15285 ) ;
#5082 = FACE_OUTER_BOUND ( 'NONE', #24638, .T. ) ;
#5083 = EDGE_CURVE ( 'NONE', #24941, #45907, #47584, .T. ) ;
#5084 = ORIENTED_EDGE ( 'NONE', *, *, #34515, .F. ) ;
#5085 = ORIENTED_EDGE ( 'NONE', *, *, #43004, .F. ) ;
#5086 = ADVANCED_FACE ( 'NONE', ( #44169 ), #10877, .T. ) ;
#5087 = CARTESIAN_POINT ( 'NONE',  ( -42.50000000000000000, 0.000000000000000000, -13.90444123027096879 ) ) ;
#5089 = ORIENTED_EDGE ( 'NONE', *, *, #19989, .F. ) ;
#5088 = CYLINDRICAL_SURFACE ( 'NONE', #21177, 77.49899999999999523 ) ;
#5090 = CARTESIAN_POINT ( 'NONE',  ( 11.99999999999999822, -72.35160999960801576, -20.41045688087902121 ) ) ;
#5091 = ORIENTED_EDGE ( 'NONE', *, *, #170, .F. ) ;
#5092 = CIRCLE ( 'NONE', #33215, 77.49899999999999523 ) ;
#5093 = AXIS2_PLACEMENT_3D ( 'NONE', #9210, #24144, #11261 ) ;
#5094 = ORIENTED_EDGE ( 'NONE', *, *, #9017, .T. ) ;
#5095 = CARTESIAN_POINT ( 'NONE',  ( -4.653126046682595884, -146.1313684676804314, -2.500000000000000000 ) ) ;
#5096 = EDGE_CURVE ( 'NONE', #39585, #4021, #47796, .T. ) ;
#5097 = ORIENTED_EDGE ( 'NONE', *, *, #15948, .T. ) ;
#5098 = ORIENTED_EDGE ( 'NONE', *, *, #19485, .T. ) ;
#5099 = DIRECTION ( 'NONE',  ( 0.000000000000000000, 0.5877852522924743583, -0.8090169943749465631 ) ) ;
#5100 = DIRECTION ( 'NONE',  ( -1.000000000000000000, 0.000000000000000000, 0.000000000000000000 ) ) ;
#5101 = ORIENTED_EDGE ( 'NONE', *, *, #17391, .T. ) ;
#5102 = AXIS2_PLACEMENT_3D ( 'NONE', #44522, #25915, #6846 ) ;
#5103 = DIRECTION ( 'NONE',  ( 1.000000000000000000, -0.000000000000000000, -0.000000000000000000 ) ) ;
#5104 = CARTESIAN_POINT ( 'NONE',  ( 10.00000000000000000, 35.92658777277511462, 10.74501242461295014 ) ) ;
#5105 = CARTESIAN_POINT ( 'NONE',  ( 23.11608002360578240, -124.4885236261218182, 5.500000000000000000 ) ) ;
#5107 = ORIENTED_EDGE ( 'NONE', *, *, #660, .F. ) ;
#5106 = CIRCLE ( 'NONE', #27784, 77.49899999999999523 ) ;
#5108 = VECTOR ( 'NONE', #41159, 1000.000000000000000 ) ;
#5109 = ORIENTED_EDGE ( 'NONE', *, *, #7633, .T. ) ;
#5110 = EDGE_CURVE ( 'NONE', #4856, #36554, #18098, .T. ) ;
#5111 = CARTESIAN_POINT ( 'NONE',  ( -10.00000000000000000, 0.000000000000000000, 0.000000000000000000 ) ) ;
#5112 = DIRECTION ( 'NONE',  ( 0.9918136447140104561, -0.1276937514489679681, 0.000000000000000000 ) ) ;
#5113 = ORIENTED_EDGE ( 'NONE', *, *, #27834, .T. ) ;
#5114 = ADVANCED_FACE ( 'NONE', ( #48077 ), #7197, .T. ) ;
#5115 = DIRECTION ( 'NONE',  ( 0.000000000000000000, 0.000000000000000000, 1.000000000000000000 ) ) ;
#5116 = EDGE_LOOP ( 'NONE', ( #41819, #6393, #34251, #44198 ) ) ;
#5117 = CARTESIAN_POINT ( 'NONE',  ( 10.00000000000000000, -8.840884882375609877, 74.65374052328647281 ) ) ;
#5118 = DIRECTION ( 'NONE',  ( 0.000000000000000000, 0.000000000000000000, 1.000000000000000000 ) ) ;
#5119 = CARTESIAN_POINT ( 'NONE',  ( 11.99999999999999822, -76.41127070299280888, 12.93880638057290788 ) ) ;
#5120 = VECTOR ( 'NONE', #33028, 1000.000000000000000 ) ;
#5121 = FACE_OUTER_BOUND ( 'NONE', #38688, .T. ) ;
#5122 = CARTESIAN_POINT ( 'NONE',  ( 0.000000000000000000, -77.19088730480528682, 6.903761155837488062 ) ) ;
#5123 = DIRECTION ( 'NONE',  ( 0.000000000000000000, 0.000000000000000000, 1.000000000000000000 ) ) ;
#5124 = EDGE_CURVE ( 'NONE', #33807, #33795, #30630, .T. ) ;
#5125 = CIRCLE ( 'NONE', #3535, 31.99999999999999289 ) ;
#5126 = CARTESIAN_POINT ( 'NONE',  ( 0.000000000000000000, 0.000000000000000000, 0.000000000000000000 ) ) ;
#5127 = DIRECTION ( 'NONE',  ( 0.000000000000000000, 0.000000000000000000, 1.000000000000000000 ) ) ;
#5128 = VERTEX_POINT ( 'NONE', #43460 ) ;
#5129 = PLANE ( 'NONE',  #32334 ) ;
#5130 = ORIENTED_EDGE ( 'NONE', *, *, #14237, .F. ) ;
#5131 = EDGE_CURVE ( 'NONE', #12683, #2237, #10178, .T. ) ;
#5132 = CIRCLE ( 'NONE', #48095, 82.00000000000000000 ) ;
#5133 = AXIS2_PLACEMENT_3D ( 'NONE', #3204, #39722, #40439 ) ;
#5134 = DIRECTION ( 'NONE',  ( 0.000000000000000000, 0.000000000000000000, 1.000000000000000000 ) ) ;
#5135 = AXIS2_PLACEMENT_3D ( 'NONE', #14569, #42430, #27511 ) ;
#5136 = DIRECTION ( 'NONE',  ( 0.000000000000000000, 0.000000000000000000, -1.000000000000000000 ) ) ;
#5137 = DIRECTION ( 'NONE',  ( 0.3311129884571304971, 0.9435911131814395114, -0.000000000000000000 ) ) ;
#5138 = AXIS2_PLACEMENT_3D ( 'NONE', #13287, #35563, #28209 ) ;
#5139 = ORIENTED_EDGE ( 'NONE', *, *, #3870, .F. ) ;
#5140 = VECTOR ( 'NONE', #37958, 1000.000000000000000 ) ;
#5141 = ORIENTED_EDGE ( 'NONE', *, *, #43982, .F. ) ;
#5142 = EDGE_CURVE ( 'NONE', #35877, #12792, #6249, .T. ) ;
#5143 = LINE ( 'NONE', #16628, #39016 ) ;
#5144 = VERTEX_POINT ( 'NONE', #11605 ) ;
#5145 = EDGE_CURVE ( 'NONE', #29746, #24346, #22687, .T. ) ;
#5146 = ORIENTED_EDGE ( 'NONE', *, *, #4752, .F. ) ;
#5147 = ORIENTED_EDGE ( 'NONE', *, *, #3993, .T. ) ;
#5148 = ORIENTED_EDGE ( 'NONE', *, *, #24466, .T. ) ;
#5149 = CIRCLE ( 'NONE', #5926, 77.49900000000000944 ) ;
#5150 = EDGE_LOOP ( 'NONE', ( #39270, #4477, #48247, #16445 ) ) ;
#5151 = AXIS2_PLACEMENT_3D ( 'NONE', #26782, #15770, #34352 ) ;
#5152 = EDGE_CURVE ( 'NONE', #13922, #22705, #7830, .T. ) ;
#5153 = AXIS2_PLACEMENT_3D ( 'NONE', #7400, #34, #14989 ) ;
#5154 = ADVANCED_FACE ( 'NONE', ( #15753 ), #3769, .F. ) ;
#5155 = LINE ( 'NONE', #23732, #13330 ) ;
#5156 = VERTEX_POINT ( 'NONE', #41958 ) ;
#5157 = CARTESIAN_POINT ( 'NONE',  ( 10.00000000000000000, -21.32104025579135964, 30.84782396557210760 ) ) ;
#5158 = EDGE_CURVE ( 'NONE', #2670, #23364, #20340, .T. ) ;
#5159 = EDGE_LOOP ( 'NONE', ( #22640, #32058, #29030, #23564 ) ) ;
#5160 = CARTESIAN_POINT ( 'NONE',  ( 11.99999999999999822, 0.000000000000000000, 0.000000000000000000 ) ) ;
#5161 = CARTESIAN_POINT ( 'NONE',  ( 0.000000000000000000, -17.67226234102801286, -33.17418723428327354 ) ) ;
#5162 = DIRECTION ( 'NONE',  ( -1.000000000000000000, 0.000000000000000000, -0.000000000000000000 ) ) ;
#5163 = ORIENTED_EDGE ( 'NONE', *, *, #21586, .F. ) ;
#5164 = DIRECTION ( 'NONE',  ( -1.000000000000000000, -0.000000000000000000, -0.000000000000000000 ) ) ;
#5165 = ORIENTED_EDGE ( 'NONE', *, *, #34918, .T. ) ;
#5166 = DIRECTION ( 'NONE',  ( 0.000000000000000000, -0.8090169943749531134, 0.5877852522924653655 ) ) ;
#5167 = DIRECTION ( 'NONE',  ( 0.000000000000000000, 0.000000000000000000, 1.000000000000000000 ) ) ;
#5168 = AXIS2_PLACEMENT_3D ( 'NONE', #20297, #34262, #41878 ) ;
#5169 = ORIENTED_EDGE ( 'NONE', *, *, #18937, .T. ) ;
#5170 = CARTESIAN_POINT ( 'NONE',  ( 0.000000000000000000, -49.70050353004846500, -59.46389618802017907 ) ) ;
#5171 = ORIENTED_EDGE ( 'NONE', *, *, #41777, .T. ) ;
#5172 = VERTEX_POINT ( 'NONE', #811 ) ;
#5173 = LINE ( 'NONE', #992, #32266 ) ;
#5174 = CARTESIAN_POINT ( 'NONE',  ( 11.99999999999999822, -63.18004540533059554, 44.88180994100355292 ) ) ;
#5175 = CARTESIAN_POINT ( 'NONE',  ( -10.00000000000000000, 0.000000000000000000, 0.000000000000000000 ) ) ;
#5176 = DIRECTION ( 'NONE',  ( 0.6575728627325955200, -0.7533909544171996098, 0.000000000000000000 ) ) ;
#5177 = DIRECTION ( 'NONE',  ( -1.000000000000000000, -0.000000000000000000, 0.000000000000000000 ) ) ;
#5178 = AXIS2_PLACEMENT_3D ( 'NONE', #7385, #37487, #17906 ) ;
#5179 = FACE_OUTER_BOUND ( 'NONE', #35692, .T. ) ;
#5180 = CARTESIAN_POINT ( 'NONE',  ( 11.99999999999999822, 2.946379043147425492, -75.11764819372145041 ) ) ;
#5181 = DIRECTION ( 'NONE',  ( -1.000000000000000000, -0.000000000000000000, -0.000000000000000000 ) ) ;
#5182 = EDGE_CURVE ( 'NONE', #28663, #40104, #4020, .T. ) ;
#5183 = CARTESIAN_POINT ( 'NONE',  ( 11.41210121379328335, -99.40233154247455616, 5.500000000000000000 ) ) ;
#5184 = CARTESIAN_POINT ( 'NONE',  ( 10.00000000000000000, -30.84782396557233142, 21.32104025579104345 ) ) ;
#5185 = DIRECTION ( 'NONE',  ( 0.000000000000000000, -0.5877852522924625900, -0.8090169943749551118 ) ) ;
#5186 = AXIS2_PLACEMENT_3D ( 'NONE', #45317, #45552, #11796 ) ;
#5187 = DIRECTION ( 'NONE',  ( -1.000000000000000000, 0.000000000000000000, 0.000000000000000000 ) ) ;
#5188 = CARTESIAN_POINT ( 'NONE',  ( 15.00000000000000000, -14.54903810567644484, 22.19967320028775504 ) ) ;
#5189 = CARTESIAN_POINT ( 'NONE',  ( 11.99999999999999822, 0.000000000000000000, 0.000000000000000000 ) ) ;
#5190 = ADVANCED_FACE ( 'NONE', ( #22851 ), #15035, .T. ) ;
#5191 = VECTOR ( 'NONE', #28200, 1000.000000000000000 ) ;
#5192 = CARTESIAN_POINT ( 'NONE',  ( 5.000000000000002665, 76.69515212746016175, 29.01471420065591289 ) ) ;
#5193 = ORIENTED_EDGE ( 'NONE', *, *, #41737, .F. ) ;
#5194 = EDGE_LOOP ( 'NONE', ( #9194, #1877, #34528, #25970 ) ) ;
#5195 = AXIS2_PLACEMENT_3D ( 'NONE', #16145, #34968, #2171 ) ;
#5196 = EDGE_CURVE ( 'NONE', #34190, #6985, #21907, .T. ) ;
#5197 = CARTESIAN_POINT ( 'NONE',  ( 10.00000000000000000, -73.44644590900043113, -24.73286445877782924 ) ) ;
#5198 = DIRECTION ( 'NONE',  ( -1.000000000000000000, -0.000000000000000000, -0.000000000000000000 ) ) ;
#5199 = APPLICATION_PROTOCOL_DEFINITION ( 'draft international standard', 'automotive_design', 1998, #9147 ) ;
#5200 = DIRECTION ( 'NONE',  ( 0.000000000000000000, -0.4539904997395351471, -0.8910065241883737830 ) ) ;
#5201 = EDGE_LOOP ( 'NONE', ( #47018, #15746, #13501, #36436 ) ) ;
#5202 = CIRCLE ( 'NONE', #15374, 31.99999999999999645 ) ;
#5203 = EDGE_CURVE ( 'NONE', #46629, #9112, #14898, .T. ) ;
#5204 = ORIENTED_EDGE ( 'NONE', *, *, #10719, .T. ) ;
#5205 = DIRECTION ( 'NONE',  ( 0.000000000000000000, 0.000000000000000000, 1.000000000000000000 ) ) ;
#5206 = AXIS2_PLACEMENT_3D ( 'NONE', #8585, #34777, #1263 ) ;
#5207 = VERTEX_POINT ( 'NONE', #15514 ) ;
#5209 = EDGE_CURVE ( 'NONE', #10969, #33189, #41463, .T. ) ;
#5208 = CARTESIAN_POINT ( 'NONE',  ( 5.000000000000002665, -81.34940948281344220, 10.30890764327356557 ) ) ;
#5210 = ORIENTED_EDGE ( 'NONE', *, *, #29303, .T. ) ;
#5211 = CARTESIAN_POINT ( 'NONE',  ( 11.99999999999999822, 30.41916302227216562, -71.27951684757994144 ) ) ;
#5212 = ORIENTED_EDGE ( 'NONE', *, *, #2759, .F. ) ;
#5213 = AXIS2_PLACEMENT_3D ( 'NONE', #17310, #40742, #46950 ) ;
#5214 = ADVANCED_FACE ( 'NONE', ( #14793 ), #23335, .T. ) ;
#5215 = CYLINDRICAL_SURFACE ( 'NONE', #8626, 16.00000000000000000 ) ;
#5216 = VERTEX_POINT ( 'NONE', #40989 ) ;
#5218 = ORIENTED_EDGE ( 'NONE', *, *, #38543, .F. ) ;
#5217 = DIRECTION ( 'NONE',  ( 0.000000000000000000, 0.000000000000000000, 1.000000000000000000 ) ) ;
#5219 = VERTEX_POINT ( 'NONE', #19182 ) ;
#5220 = EDGE_CURVE ( 'NONE', #43680, #34540, #34108, .T. ) ;
#5221 = FACE_BOUND ( 'NONE', #20496, .T. ) ;
#5222 = CARTESIAN_POINT ( 'NONE',  ( 11.99999999999999822, 0.000000000000000000, 0.000000000000000000 ) ) ;
#5223 = DIRECTION ( 'NONE',  ( -1.000000000000000000, 0.000000000000000000, 0.000000000000000000 ) ) ;
#5224 = DIRECTION ( 'NONE',  ( -1.000000000000000000, -0.000000000000000000, 0.000000000000000000 ) ) ;
#5225 = VECTOR ( 'NONE', #12181, 1000.000000000000000 ) ;
#5226 = DIRECTION ( 'NONE',  ( 0.000000000000000000, 0.6494480483301848794, -0.7604059656000299317 ) ) ;
#5227 = ORIENTED_EDGE ( 'NONE', *, *, #31435, .F. ) ;
#5228 = DIRECTION ( 'NONE',  ( -1.000000000000000000, 0.000000000000000000, -0.000000000000000000 ) ) ;
#5229 = EDGE_LOOP ( 'NONE', ( #10292, #13984, #30464, #42160 ) ) ;
#5230 = ORIENTED_EDGE ( 'NONE', *, *, #18944, .F. ) ;
#5231 = LINE ( 'NONE', #34829, #34858 ) ;
#5232 = ORIENTED_EDGE ( 'NONE', *, *, #26861, .F. ) ;
#5233 = CARTESIAN_POINT ( 'NONE',  ( 0.000000000000000000, 40.98264845739749518, 9.188173127307448951 ) ) ;
#5234 = FACE_OUTER_BOUND ( 'NONE', #33563, .T. ) ;
#5235 = DIRECTION ( 'NONE',  ( 0.000000000000000000, 0.000000000000000000, 1.000000000000000000 ) ) ;
#5236 = ORIENTED_EDGE ( 'NONE', *, *, #808, .T. ) ;
#5237 = DIRECTION ( 'NONE',  ( 0.000000000000000000, 0.000000000000000000, 1.000000000000000000 ) ) ;
#5238 = DIRECTION ( 'NONE',  ( -1.000000000000000000, -0.000000000000000000, -0.000000000000000000 ) ) ;
#5239 = CARTESIAN_POINT ( 'NONE',  ( 10.00000000000000000, 2.663952781846149254, 41.91543099594818500 ) ) ;
#5240 = CARTESIAN_POINT ( 'NONE',  ( 11.99999999999999822, 0.000000000000000000, 0.000000000000000000 ) ) ;
#5241 = FACE_OUTER_BOUND ( 'NONE', #4526, .T. ) ;
#5242 = VECTOR ( 'NONE', #44693, 1000.000000000000000 ) ;
#5243 = DIRECTION ( 'NONE',  ( -1.000000000000000000, -0.000000000000000000, 0.000000000000000000 ) ) ;
#5244 = PLANE ( 'NONE',  #34523 ) ;
#5245 = DIRECTION ( 'NONE',  ( 0.000000000000000000, 0.000000000000000000, 1.000000000000000000 ) ) ;
#5246 = AXIS2_PLACEMENT_3D ( 'NONE', #24682, #42570, #17087 ) ;
#5247 = DIRECTION ( 'NONE',  ( 0.000000000000000000, -6.938893903907228378E-15, 1.000000000000000000 ) ) ;
#5248 = FACE_OUTER_BOUND ( 'NONE', #30473, .T. ) ;
#5249 = EDGE_LOOP ( 'NONE', ( #19968, #48396, #21594, #26137 ) ) ;
#5250 = ORIENTED_EDGE ( 'NONE', *, *, #33958, .T. ) ;
#5251 = CARTESIAN_POINT ( 'NONE',  ( 0.000000000000000000, 0.000000000000000000, 0.000000000000000000 ) ) ;
#5252 = AXIS2_PLACEMENT_3D ( 'NONE', #46347, #27514, #5245 ) ;
#5253 = ORIENTED_EDGE ( 'NONE', *, *, #45217, .F. ) ;
#5254 = FACE_OUTER_BOUND ( 'NONE', #25274, .T. ) ;
#5255 = EDGE_CURVE ( 'NONE', #18838, #21898, #45606, .T. ) ;
#5256 = AXIS2_PLACEMENT_3D ( 'NONE', #16315, #35383, #8964 ) ;
#5257 = EDGE_CURVE ( 'NONE', #6838, #20356, #12101, .T. ) ;
#5258 = DIRECTION ( 'NONE',  ( -1.000000000000000000, -0.000000000000000000, 0.000000000000000000 ) ) ;
#5259 = ORIENTED_EDGE ( 'NONE', *, *, #31573, .T. ) ;
#5260 = CIRCLE ( 'NONE', #25568, 31.99999999999998224 ) ;
#5261 = ORIENTED_EDGE ( 'NONE', *, *, #20374, .F. ) ;
#5262 = EDGE_CURVE ( 'NONE', #44202, #844, #43063, .T. ) ;
#5263 = ORIENTED_EDGE ( 'NONE', *, *, #13128, .F. ) ;
#5264 = EDGE_CURVE ( 'NONE', #21229, #27047, #11797, .T. ) ;
#5265 = EDGE_CURVE ( 'NONE', #5635, #27337, #7098, .T. ) ;
#5266 = CIRCLE ( 'NONE', #17759, 37.49900000000000944 ) ;
#5267 = CARTESIAN_POINT ( 'NONE',  ( 0.000000000000000000, 5.835314593368772229, -22.81335362449846826 ) ) ;
#5268 = ORIENTED_EDGE ( 'NONE', *, *, #16498, .F. ) ;
#5269 = DIRECTION ( 'NONE',  ( -1.000000000000000000, 0.000000000000000000, 0.000000000000000000 ) ) ;
#5270 = CARTESIAN_POINT ( 'NONE',  ( 10.00000000000000000, -74.74816331893453025, 33.71516098798714722 ) ) ;
#5271 = VERTEX_POINT ( 'NONE', #11120 ) ;
#5272 = AXIS2_PLACEMENT_3D ( 'NONE', #36646, #21726, #40570 ) ;
#5273 = DIRECTION ( 'NONE',  ( 0.000000000000000000, 0.000000000000000000, 1.000000000000000000 ) ) ;
#5274 = EDGE_CURVE ( 'NONE', #20737, #29586, #26041, .T. ) ;
#5275 = ORIENTED_EDGE ( 'NONE', *, *, #25793, .F. ) ;
#5276 = DIRECTION ( 'NONE',  ( -1.000000000000000000, 0.000000000000000000, 0.000000000000000000 ) ) ;
#5277 = CARTESIAN_POINT ( 'NONE',  ( 0.000000000000000000, 21.40280677340371795, 36.13751322684426270 ) ) ;
#5278 = CARTESIAN_POINT ( 'NONE',  ( 10.00000000000000000, -51.03279382321048985, -55.19960302592120627 ) ) ;
#5279 = ORIENTED_EDGE ( 'NONE', *, *, #48082, .F. ) ;
#5280 = CIRCLE ( 'NONE', #46728, 15.99999999999999822 ) ;
#5281 = VERTEX_POINT ( 'NONE', #27505 ) ;
#5282 = DIRECTION ( 'NONE',  ( 0.000000000000000000, 0.000000000000000000, -1.000000000000000000 ) ) ;
#5283 = EDGE_LOOP ( 'NONE', ( #10288, #44873, #35700, #38505 ) ) ;
#5284 = CARTESIAN_POINT ( 'NONE',  ( 0.000000000000000000, -63.97538442413390669, -51.29473840253292849 ) ) ;
#5285 = DIRECTION ( 'NONE',  ( -1.000000000000000000, -0.000000000000000000, 0.000000000000000000 ) ) ;
#5286 = CARTESIAN_POINT ( 'NONE',  ( 10.00000000000000000, -12.42422080174614862, -35.38097989696524337 ) ) ;
#5287 = DIRECTION ( 'NONE',  ( -1.000000000000000000, 0.000000000000000000, 0.000000000000000000 ) ) ;
#5288 = DIRECTION ( 'NONE',  ( -1.000000000000000000, 0.000000000000000000, -0.000000000000000000 ) ) ;
#5289 = CARTESIAN_POINT ( 'NONE',  ( 0.000000000000000000, 0.000000000000000000, 0.000000000000000000 ) ) ;
#5290 = CYLINDRICAL_SURFACE ( 'NONE', #39297, 77.49899999999999523 ) ;
#5291 = EDGE_LOOP ( 'NONE', ( #20284, #4067, #21062, #29196 ) ) ;
#5292 = DIRECTION ( 'NONE',  ( -1.000000000000000000, -0.000000000000000000, 0.000000000000000000 ) ) ;
#5293 = CARTESIAN_POINT ( 'NONE',  ( 0.000000000000000000, 0.000000000000000000, 2.500000000000000000 ) ) ;
#5294 = AXIS2_PLACEMENT_3D ( 'NONE', #15305, #4755, #24256 ) ;
#5295 = DIRECTION ( 'NONE',  ( 0.000000000000000000, -0.5877852522924624790, -0.8090169943749551118 ) ) ;
#5296 = CARTESIAN_POINT ( 'NONE',  ( 5.000000000000002665, -34.94270380257586339, -74.18225833017926618 ) ) ;
#5297 = ORIENTED_EDGE ( 'NONE', *, *, #36242, .T. ) ;
#5298 = CARTESIAN_POINT ( 'NONE',  ( 0.000000000000000000, -56.15606465354917276, -59.75363087400133111 ) ) ;
#5299 = CARTESIAN_POINT ( 'NONE',  ( 0.000000000000000000, 8.830959090342393125, 74.65491531819122883 ) ) ;
#5300 = DIRECTION ( 'NONE',  ( -1.000000000000000000, 0.000000000000000000, 0.000000000000000000 ) ) ;
#5301 = EDGE_CURVE ( 'NONE', #4198, #20488, #42423, .T. ) ;
#5302 = CYLINDRICAL_SURFACE ( 'NONE', #45113, 42.00000000000000000 ) ;
#5303 = DIRECTION ( 'NONE',  ( -1.000000000000000000, 0.000000000000000000, 0.000000000000000000 ) ) ;
#5304 = VECTOR ( 'NONE', #2257, 1000.000000000000000 ) ;
#5305 = ORIENTED_EDGE ( 'NONE', *, *, #16689, .T. ) ;
#5306 = EDGE_CURVE ( 'NONE', #34900, #4717, #19594, .T. ) ;
#5307 = FACE_OUTER_BOUND ( 'NONE', #27252, .T. ) ;
#5308 = CARTESIAN_POINT ( 'NONE',  ( 10.00000000000000000, 33.79645857604513992, -16.45098606841138178 ) ) ;
#5309 = VERTEX_POINT ( 'NONE', #1056 ) ;
#5310 = EDGE_CURVE ( 'NONE', #10117, #30305, #23571, .T. ) ;
#5311 = AXIS2_PLACEMENT_3D ( 'NONE', #44127, #24372, #46667 ) ;
#5312 = ORIENTED_EDGE ( 'NONE', *, *, #28749, .T. ) ;
#5313 = FILL_AREA_STYLE_COLOUR ( '', #21751 ) ;
#5314 = ADVANCED_FACE ( 'NONE', ( #45869 ), #9365, .F. ) ;
#5315 = DIRECTION ( 'NONE',  ( -1.000000000000000000, 0.000000000000000000, -0.000000000000000000 ) ) ;
#5316 = ORIENTED_EDGE ( 'NONE', *, *, #17076, .T. ) ;
#5317 = ORIENTED_EDGE ( 'NONE', *, *, #45644, .F. ) ;
#5318 = VERTEX_POINT ( 'NONE', #24301 ) ;
#5319 = LINE ( 'NONE', #5805, #28868 ) ;
#5320 = EDGE_LOOP ( 'NONE', ( #14797, #43749, #7077, #45314 ) ) ;
#5321 = EDGE_CURVE ( 'NONE', #21795, #34900, #25051, .T. ) ;
#5322 = ADVANCED_FACE ( 'NONE', ( #28214 ), #35074, .T. ) ;
#5323 = CIRCLE ( 'NONE', #14716, 31.99999999999998579 ) ;
#5324 = ORIENTED_EDGE ( 'NONE', *, *, #27522, .T. ) ;
#5325 = CYLINDRICAL_SURFACE ( 'NONE', #46073, 31.99999999999998579 ) ;
#5326 = CARTESIAN_POINT ( 'NONE',  ( 50.00005079999999680, 0.000000000000000000, 0.000000000000000000 ) ) ;
#5327 = ORIENTED_EDGE ( 'NONE', *, *, #4322, .F. ) ;
#5328 = ORIENTED_EDGE ( 'NONE', *, *, #44382, .T. ) ;
#5329 = LINE ( 'NONE', #17053, #46751 ) ;
#5330 = EDGE_CURVE ( 'NONE', #44442, #12242, #28968, .T. ) ;
#5332 = EDGE_LOOP ( 'NONE', ( #23307, #33843, #24527, #47412 ) ) ;
#5331 = CARTESIAN_POINT ( 'NONE',  ( 0.000000000000000000, -4.261787119645322974, 26.19803753235775190 ) ) ;
#5333 = AXIS2_PLACEMENT_3D ( 'NONE', #11546, #34043, #525 ) ;
#5334 = DIRECTION ( 'NONE',  ( 0.000000000000000000, 0.000000000000000000, 1.000000000000000000 ) ) ;
#5335 = VERTEX_POINT ( 'NONE', #5703 ) ;
#5336 = CARTESIAN_POINT ( 'NONE',  ( 10.00000000000000000, 10.74501242461282757, 35.92658777277515014 ) ) ;
#5337 = ORIENTED_EDGE ( 'NONE', *, *, #47705, .F. ) ;
#5338 = ORIENTED_EDGE ( 'NONE', *, *, #24427, .F. ) ;
#5339 = CARTESIAN_POINT ( 'NONE',  ( 10.00000000000000000, 21.32104025579114648, 30.84782396557224970 ) ) ;
#5340 = DIRECTION ( 'NONE',  ( 0.000000000000000000, -0.8660254037844363761, 0.5000000000000039968 ) ) ;
#5341 = VERTEX_POINT ( 'NONE', #42678 ) ;
#5342 = VECTOR ( 'NONE', #32094, 1000.000000000000000 ) ;
#5343 = CARTESIAN_POINT ( 'NONE',  ( -3.000000000000000000, 8.688484142253939169, 21.88630264137371029 ) ) ;
#5344 = CARTESIAN_POINT ( 'NONE',  ( 0.000000000000000000, 0.000000000000000000, 0.000000000000000000 ) ) ;
#5345 = DIRECTION ( 'NONE',  ( 0.000000000000000000, -0.6691306063588586817, 0.7431448254773939111 ) ) ;
#5346 = ORIENTED_EDGE ( 'NONE', *, *, #20683, .T. ) ;
#5347 = ORIENTED_EDGE ( 'NONE', *, *, #35422, .F. ) ;
#5348 = FACE_OUTER_BOUND ( 'NONE', #44783, .T. ) ;
#5349 = CARTESIAN_POINT ( 'NONE',  ( 0.000000000000000000, 17.28742895386190526, -75.54627589209924565 ) ) ;
#5350 = ORIENTED_EDGE ( 'NONE', *, *, #28932, .T. ) ;
#5351 = VERTEX_POINT ( 'NONE', #19899 ) ;
#5352 = CARTESIAN_POINT ( 'NONE',  ( 10.00000000000000000, -75.54627589209931671, -17.28742895386164591 ) ) ;
#5353 = VERTEX_POINT ( 'NONE', #23826 ) ;
#5354 = DIRECTION ( 'NONE',  ( 1.000000000000000000, -0.000000000000000000, -0.000000000000000000 ) ) ;
#5355 = DIRECTION ( 'NONE',  ( 0.000000000000000000, -0.2334453638558922350, -0.9723699203976797767 ) ) ;
#5356 = CARTESIAN_POINT ( 'NONE',  ( 10.00000000000000000, 54.21277698773752718, -55.38113227695725271 ) ) ;
#5357 = CYLINDRICAL_SURFACE ( 'NONE', #33057, 37.49900000000000233 ) ;
#5358 =( NAMED_UNIT ( * ) PLANE_ANGLE_UNIT ( ) SI_UNIT ( $, .RADIAN. ) );
#5359 = CARTESIAN_POINT ( 'NONE',  ( 10.00000000000000000, 6.555932627142952995, -37.01155633439051940 ) ) ;
#5360 = EDGE_CURVE ( 'NONE', #4198, #6843, #25858, .T. ) ;
#5361 = DIRECTION ( 'NONE',  ( 0.000000000000000000, 0.000000000000000000, 1.000000000000000000 ) ) ;
#5362 = DIRECTION ( 'NONE',  ( 0.000000000000000000, 0.000000000000000000, 1.000000000000000000 ) ) ;
#5363 = EDGE_CURVE ( 'NONE', #39037, #17758, #16003, .T. ) ;
#5364 = DIRECTION ( 'NONE',  ( 1.000000000000000000, -0.000000000000000000, -0.000000000000000000 ) ) ;
#5365 = EDGE_CURVE ( 'NONE', #33821, #43969, #9137, .T. ) ;
#5366 = ORIENTED_EDGE ( 'NONE', *, *, #15708, .F. ) ;
#5367 = VERTEX_POINT ( 'NONE', #4977 ) ;
#5368 = CARTESIAN_POINT ( 'NONE',  ( 15.00000000000000000, -13.04903810567675393, -19.60159698893424718 ) ) ;
#5369 = VERTEX_POINT ( 'NONE', #1791 ) ;
#5370 = CIRCLE ( 'NONE', #25679, 31.99999999999999289 ) ;
#5371 = AXIS2_PLACEMENT_3D ( 'NONE', #2610, #10712, #48146 ) ;
#5372 = CARTESIAN_POINT ( 'NONE',  ( 11.99999999999999822, -17.28742895386031719, -75.54627589209962935 ) ) ;
#5373 = DIRECTION ( 'NONE',  ( -1.000000000000000000, -0.000000000000000000, -0.000000000000000000 ) ) ;
#5374 = VECTOR ( 'NONE', #39539, 1000.000000000000000 ) ;
#5375 = ORIENTED_EDGE ( 'NONE', *, *, #44430, .T. ) ;
#5376 = EDGE_CURVE ( 'NONE', #30369, #46765, #24297, .T. ) ;
#5377 = EDGE_CURVE ( 'NONE', #6953, #14712, #31335, .T. ) ;
#5378 = EDGE_CURVE ( 'NONE', #32480, #4066, #22718, .T. ) ;
#5379 = CARTESIAN_POINT ( 'NONE',  ( 16.30584220631899228, -140.9432449716519784, 5.500000000000000000 ) ) ;
#5380 = EDGE_LOOP ( 'NONE', ( #10296, #873, #43312, #42598 ) ) ;
#5381 = ORIENTED_EDGE ( 'NONE', *, *, #46551, .F. ) ;
#5382 = ORIENTED_EDGE ( 'NONE', *, *, #3068, .F. ) ;
#5383 = VERTEX_POINT ( 'NONE', #25200 ) ;
#5384 = ADVANCED_FACE ( 'NONE', ( #12337 ), #44627, .F. ) ;
#5385 = DIRECTION ( 'NONE',  ( -1.000000000000000000, 0.000000000000000000, 0.000000000000000000 ) ) ;
#5386 = ORIENTED_EDGE ( 'NONE', *, *, #29081, .T. ) ;
#5387 = FACE_OUTER_BOUND ( 'NONE', #33200, .T. ) ;
#5388 = ORIENTED_EDGE ( 'NONE', *, *, #33571, .T. ) ;
#5389 = DIRECTION ( 'NONE',  ( 0.6862798483830533369, 0.7273375899149812085, 0.000000000000000000 ) ) ;
#5390 = CARTESIAN_POINT ( 'NONE',  ( 11.59999999999999787, 1.420590287010929336E-15, 42.00000000000001421 ) ) ;
#5391 = DIRECTION ( 'NONE',  ( -1.000000000000000000, 0.000000000000000000, 0.000000000000000000 ) ) ;
#5392 = VERTEX_POINT ( 'NONE', #34573 ) ;
#5393 = DIRECTION ( 'NONE',  ( 0.000000000000000000, -0.9781476007338070211, -0.2079116908177532363 ) ) ;
#5394 = ORIENTED_EDGE ( 'NONE', *, *, #4491, .F. ) ;
#5395 = CARTESIAN_POINT ( 'NONE',  ( 0.000000000000000000, 0.000000000000000000, 0.000000000000000000 ) ) ;
#5396 = CARTESIAN_POINT ( 'NONE',  ( 10.00000000000000000, 0.000000000000000000, 0.000000000000000000 ) ) ;
#5397 = DIRECTION ( 'NONE',  ( 0.000000000000000000, -0.07845909572783058006, -0.9969173337331290741 ) ) ;
#5398 = ORIENTED_EDGE ( 'NONE', *, *, #44088, .T. ) ;
#5399 = VECTOR ( 'NONE', #20731, 1000.000000000000000 ) ;
#5400 = ORIENTED_EDGE ( 'NONE', *, *, #19635, .F. ) ;
#5401 = CARTESIAN_POINT ( 'NONE',  ( 11.99999999999999822, 8.830959090343430518, -74.65491531819107252 ) ) ;
#5402 = LINE ( 'NONE', #1987, #2743 ) ;
#5403 = ORIENTED_EDGE ( 'NONE', *, *, #22500, .T. ) ;
#5404 = AXIS2_PLACEMENT_3D ( 'NONE', #8982, #45955, #2130 ) ;
#5405 = DIRECTION ( 'NONE',  ( 0.000000000000000000, 0.000000000000000000, 1.000000000000000000 ) ) ;
#5406 = LINE ( 'NONE', #20563, #15714 ) ;
#5407 = FACE_OUTER_BOUND ( 'NONE', #33679, .T. ) ;
#5408 = AXIS2_PLACEMENT_3D ( 'NONE', #15824, #19250, #33689 ) ;
#5409 = ORIENTED_EDGE ( 'NONE', *, *, #30554, .T. ) ;
#5410 = AXIS2_PLACEMENT_3D ( 'NONE', #3758, #15024, #26757 ) ;
#5411 = DIRECTION ( 'NONE',  ( -0.5000000000000039968, 0.8660254037844363761, 0.000000000000000000 ) ) ;
#5412 = DIRECTION ( 'NONE',  ( 1.000000000000000000, 0.000000000000000000, 0.000000000000000000 ) ) ;
#5413 = CARTESIAN_POINT ( 'NONE',  ( 10.00000000000000000, 16.23288003029497162, 33.80338159004289622 ) ) ;
#5414 = DIRECTION ( 'NONE',  ( 0.000000000000000000, 0.000000000000000000, 1.000000000000000000 ) ) ;
#5415 = CARTESIAN_POINT ( 'NONE',  ( 0.000000000000000000, 69.42325613327439271, 34.44570377933623462 ) ) ;
#5416 = DIRECTION ( 'NONE',  ( 1.000000000000000000, -0.000000000000000000, -0.000000000000000000 ) ) ;
#5417 = ADVANCED_FACE ( 'NONE', ( #27262 ), #30945, .T. ) ;
#5418 = DIRECTION ( 'NONE',  ( -0.000000000000000000, 0.9510565162951539753, 0.3090169943749461745 ) ) ;
#5419 = CARTESIAN_POINT ( 'NONE',  ( 10.00000000000000000, -33.80338159004296017, 16.23288003029484727 ) ) ;
#5420 = CARTESIAN_POINT ( 'NONE',  ( -10.00000000000000000, 0.000000000000000000, 0.000000000000000000 ) ) ;
#5421 = ADVANCED_FACE ( 'NONE', ( #20148 ), #16480, .T. ) ;
#5422 = CYLINDRICAL_SURFACE ( 'NONE', #16290, 35.50000000000000711 ) ;
#5423 = EDGE_CURVE ( 'NONE', #46450, #44447, #37571, .T. ) ;
#5424 = VERTEX_POINT ( 'NONE', #18140 ) ;
#5425 = ORIENTED_EDGE ( 'NONE', *, *, #45655, .T. ) ;
#5426 = EDGE_CURVE ( 'NONE', #25415, #16364, #23523, .T. ) ;
#5427 = CYLINDRICAL_SURFACE ( 'NONE', #33096, 82.00000000000000000 ) ;
#5428 = EDGE_CURVE ( 'NONE', #34042, #2158, #28458, .T. ) ;
#5429 = EDGE_CURVE ( 'NONE', #40000, #30381, #8663, .T. ) ;
#5430 = CARTESIAN_POINT ( 'NONE',  ( 6.000000000000000000, 21.60688246758586928, 79.10210256391376049 ) ) ;
#5431 = DIRECTION ( 'NONE',  ( 0.000000000000000000, 0.000000000000000000, 1.000000000000000000 ) ) ;
#5432 = ORIENTED_EDGE ( 'NONE', *, *, #4912, .F. ) ;
#5433 = AXIS2_PLACEMENT_3D ( 'NONE', #13009, #13239, #5411 ) ;
#5434 = EDGE_CURVE ( 'NONE', #2104, #19636, #14135, .T. ) ;
#5435 = CYLINDRICAL_SURFACE ( 'NONE', #32775, 42.00000000000000000 ) ;
#5436 = FACE_OUTER_BOUND ( 'NONE', #12838, .T. ) ;
#5437 = CIRCLE ( 'NONE', #11689, 42.00000000000000000 ) ;
#5438 = ORIENTED_EDGE ( 'NONE', *, *, #42067, .F. ) ;
#5439 = DIRECTION ( 'NONE',  ( -1.000000000000000000, -0.000000000000000000, 0.000000000000000000 ) ) ;
#5440 = ADVANCED_FACE ( 'NONE', ( #36036 ), #21824, .F. ) ;
#5441 = CYLINDRICAL_SURFACE ( 'NONE', #26090, 31.99999999999999289 ) ;
#5442 = AXIS2_PLACEMENT_3D ( 'NONE', #26286, #39836, #33385 ) ;
#5443 = CARTESIAN_POINT ( 'NONE',  ( 0.000000000000000000, -49.70050353004846500, -59.46389618802017907 ) ) ;
#5444 = ORIENTED_EDGE ( 'NONE', *, *, #20210, .T. ) ;
#5445 = FACE_OUTER_BOUND ( 'NONE', #12976, .T. ) ;
#5446 = ORIENTED_EDGE ( 'NONE', *, *, #45510, .T. ) ;
#5447 = CARTESIAN_POINT ( 'NONE',  ( 10.00000000000000000, -16.23288003029521320, 33.80338159004277543 ) ) ;
#5448 = DIRECTION ( 'NONE',  ( 1.000000000000000000, 0.000000000000000000, 0.000000000000000000 ) ) ;
#5449 = CARTESIAN_POINT ( 'NONE',  ( 10.00000000000000000, 65.58780272294129077, -36.73666225445822420 ) ) ;
#5450 = DIRECTION ( 'NONE',  ( 0.000000000000000000, 0.000000000000000000, -1.000000000000000000 ) ) ;
#5451 = EDGE_CURVE ( 'NONE', #48002, #37265, #2982, .T. ) ;
#5452 = CARTESIAN_POINT ( 'NONE',  ( 2.500000000000000444, 8.494897427831771708, -10.00000000000000178 ) ) ;
#5453 = ORIENTED_EDGE ( 'NONE', *, *, #13441, .T. ) ;
#5454 = CARTESIAN_POINT ( 'NONE',  ( 0.000000000000000000, 6.736453364083555329, 36.88895765772635116 ) ) ;
#5455 = EDGE_LOOP ( 'NONE', ( #22838, #41930, #17871, #13620 ) ) ;
#5456 = ORIENTED_EDGE ( 'NONE', *, *, #2688, .F. ) ;
#5457 = CARTESIAN_POINT ( 'NONE',  ( 0.000000000000000000, 33.71516098798740302, 74.74816331893443078 ) ) ;
#5458 = CARTESIAN_POINT ( 'NONE',  ( -2.499999999999997780, 8.494897427831771708, 0.000000000000000000 ) ) ;
#5459 = CARTESIAN_POINT ( 'NONE',  ( 0.000000000000000000, 22.74946021919133088, 29.81001611431016229 ) ) ;
#5460 = DIRECTION ( 'NONE',  ( 0.000000000000000000, 0.000000000000000000, 1.000000000000000000 ) ) ;
#5461 = ORIENTED_EDGE ( 'NONE', *, *, #20226, .F. ) ;
#5462 = CARTESIAN_POINT ( 'NONE',  ( 11.99999999999999822, -55.38113227695820484, 54.21277698773656084 ) ) ;
#5463 = LINE ( 'NONE', #46832, #39327 ) ;
#5464 = CYLINDRICAL_SURFACE ( 'NONE', #7867, 77.49899999999999523 ) ;
#5465 = CARTESIAN_POINT ( 'NONE',  ( 11.34017801569539685, -96.04900080221412395, -2.500000000000000000 ) ) ;
#5466 = EDGE_CURVE ( 'NONE', #9826, #17470, #2263, .T. ) ;
#5468 = AXIS2_PLACEMENT_3D ( 'NONE', #36465, #3660, #29600 ) ;
#5467 = CARTESIAN_POINT ( 'NONE',  ( 0.000000000000000000, -16.45098606841102651, -33.79645857604531045 ) ) ;
#5469 = AXIS2_PLACEMENT_3D ( 'NONE', #39769, #43903, #6229 ) ;
#5470 = DIRECTION ( 'NONE',  ( 0.000000000000000000, 0.000000000000000000, -1.000000000000000000 ) ) ;
#5471 = CARTESIAN_POINT ( 'NONE',  ( 5.000000000000002665, -71.87247863392443037, 39.47590169984818687 ) ) ;
#5472 = DIRECTION ( 'NONE',  ( 0.000000000000000000, 0.000000000000000000, 1.000000000000000000 ) ) ;
#5473 = ADVANCED_FACE ( 'NONE', ( #33082 ), #36749, .F. ) ;
#5474 = VECTOR ( 'NONE', #9340, 1000.000000000000000 ) ;
#5475 = CARTESIAN_POINT ( 'NONE',  ( 10.00000000000000000, 0.000000000000000000, 0.000000000000000000 ) ) ;
#5476 = DIRECTION ( 'NONE',  ( 0.000000000000000000, 0.000000000000000000, 1.000000000000000000 ) ) ;
#5477 = EDGE_CURVE ( 'NONE', #5271, #17177, #25500, .T. ) ;
#5478 = EDGE_CURVE ( 'NONE', #17528, #36602, #6672, .T. ) ;
#5479 = STYLED_ITEM ( 'NONE', ( #40079 ), #19421 ) ;
#5480 = ORIENTED_EDGE ( 'NONE', *, *, #3126, .F. ) ;
#5481 = EDGE_LOOP ( 'NONE', ( #39773, #8652, #11031, #42965 ) ) ;
#5482 = CARTESIAN_POINT ( 'NONE',  ( 0.000000000000000000, 65.58780272294129077, -36.73666225445822420 ) ) ;
#5483 = CIRCLE ( 'NONE', #46916, 37.49900000000000944 ) ;
#5484 = ORIENTED_EDGE ( 'NONE', *, *, #22872, .T. ) ;
#5485 = ADVANCED_FACE ( 'NONE', ( #10589 ), #28926, .T. ) ;
#5486 = FACE_OUTER_BOUND ( 'NONE', #22731, .T. ) ;
#5487 = DIRECTION ( 'NONE',  ( -1.000000000000000000, 0.000000000000000000, 0.000000000000000000 ) ) ;
#5488 = EDGE_LOOP ( 'NONE', ( #7913, #40715, #15550, #23949 ) ) ;
#5489 = ORIENTED_EDGE ( 'NONE', *, *, #47854, .F. ) ;
#5490 = DIRECTION ( 'NONE',  ( -1.000000000000000000, -0.000000000000000000, -0.000000000000000000 ) ) ;
#5491 = ORIENTED_EDGE ( 'NONE', *, *, #23362, .T. ) ;
#5492 = VERTEX_POINT ( 'NONE', #47061 ) ;
#5493 = ORIENTED_EDGE ( 'NONE', *, *, #9658, .F. ) ;
#5494 = CIRCLE ( 'NONE', #11750, 42.00000000000000000 ) ;
#5495 = FACE_OUTER_BOUND ( 'NONE', #33374, .T. ) ;
#5496 = AXIS2_PLACEMENT_3D ( 'NONE', #13507, #47735, #9578 ) ;
#5497 = LINE ( 'NONE', #8443, #19518 ) ;
#5498 = LINE ( 'NONE', #43185, #34779 ) ;
#5499 = AXIS2_PLACEMENT_3D ( 'NONE', #33620, #41231, #4504 ) ;
#5500 = AXIS2_PLACEMENT_3D ( 'NONE', #30135, #3, #41875 ) ;
#5501 = VERTEX_POINT ( 'NONE', #44351 ) ;
#5502 = CYLINDRICAL_SURFACE ( 'NONE', #6275, 12.49999999999999645 ) ;
#5503 = ORIENTED_EDGE ( 'NONE', *, *, #37007, .T. ) ;
#5504 = ORIENTED_EDGE ( 'NONE', *, *, #23270, .T. ) ;
#5505 = STYLED_ITEM ( 'NONE', ( #20352 ), #19734 ) ;
#5506 = DIRECTION ( 'NONE',  ( -1.000000000000000000, 0.000000000000000000, 0.000000000000000000 ) ) ;
#5507 = CARTESIAN_POINT ( 'NONE',  ( 0.000000000000000000, 0.000000000000000000, 0.000000000000000000 ) ) ;
#5508 = AXIS2_PLACEMENT_3D ( 'NONE', #17676, #47759, #29165 ) ;
#5509 = DIRECTION ( 'NONE',  ( -1.000000000000000000, 0.000000000000000000, 0.000000000000000000 ) ) ;
#5510 = EDGE_LOOP ( 'NONE', ( #14075, #42291, #38865, #6032 ) ) ;
#5511 = ORIENTED_EDGE ( 'NONE', *, *, #14044, .F. ) ;
#5512 = CIRCLE ( 'NONE', #10995, 77.49899999999999523 ) ;
#5513 = DIRECTION ( 'NONE',  ( 0.000000000000000000, 0.7071067811865487940, -0.7071067811865462405 ) ) ;
#5514 = ORIENTED_EDGE ( 'NONE', *, *, #36182, .F. ) ;
#5515 = FACE_OUTER_BOUND ( 'NONE', #36818, .T. ) ;
#5516 = CYLINDRICAL_SURFACE ( 'NONE', #15981, 12.49999999999999645 ) ;
#5517 = CARTESIAN_POINT ( 'NONE',  ( 0.000000000000000000, 27.13269053701096922, 25.88420570971410228 ) ) ;
#5518 = DIRECTION ( 'NONE',  ( -1.000000000000000000, 0.000000000000000000, -0.000000000000000000 ) ) ;
#5519 = FACE_OUTER_BOUND ( 'NONE', #968, .T. ) ;
#5520 = DIRECTION ( 'NONE',  ( 0.000000000000000000, 0.5877852522924742473, -0.8090169943749466741 ) ) ;
#5521 = CARTESIAN_POINT ( 'NONE',  ( 10.00000000000000000, 0.000000000000000000, 0.000000000000000000 ) ) ;
#5522 = ORIENTED_EDGE ( 'NONE', *, *, #3171, .F. ) ;
#5523 = DIRECTION ( 'NONE',  ( -1.000000000000000000, -0.000000000000000000, 0.000000000000000000 ) ) ;
#5524 = DIRECTION ( 'NONE',  ( -1.000000000000000000, 0.000000000000000000, -0.000000000000000000 ) ) ;
#5525 = CARTESIAN_POINT ( 'NONE',  ( 6.000000000000000000, 40.65526001592611749, 71.21200624218811015 ) ) ;
#5526 = CARTESIAN_POINT ( 'NONE',  ( 5.000000000000000000, -15.48615015657555993, -39.04073710021360455 ) ) ;
#5527 = ORIENTED_EDGE ( 'NONE', *, *, #26749, .F. ) ;
#5528 = EDGE_CURVE ( 'NONE', #6365, #37954, #26641, .T. ) ;
#5529 = DIRECTION ( 'NONE',  ( 0.000000000000000000, 0.1564344650402243742, 0.9876883405951387696 ) ) ;
#5530 = DIRECTION ( 'NONE',  ( 0.000000000000000000, 0.000000000000000000, 1.000000000000000000 ) ) ;
#5531 = EDGE_CURVE ( 'NONE', #6602, #828, #39149, .T. ) ;
#5532 = CARTESIAN_POINT ( 'NONE',  ( 0.000000000000000000, -62.50884508063395373, -41.76106447765554464 ) ) ;
#5533 = DIRECTION ( 'NONE',  ( -1.000000000000000000, 0.000000000000000000, -0.000000000000000000 ) ) ;
#5534 = EDGE_CURVE ( 'NONE', #29887, #23982, #29997, .T. ) ;
#5535 = CIRCLE ( 'NONE', #18024, 31.99999999999999645 ) ;
#5536 = CARTESIAN_POINT ( 'NONE',  ( -3.000000000000000000, 6.762365576493310826, 25.66652317338401090 ) ) ;
#5537 = DIRECTION ( 'NONE',  ( 1.000000000000000000, 0.000000000000000000, -0.000000000000000000 ) ) ;
#5538 = EDGE_LOOP ( 'NONE', ( #39001, #32288, #10362, #8761 ) ) ;
#5539 = EDGE_CURVE ( 'NONE', #6962, #11527, #29197, .T. ) ;
#5540 = DIRECTION ( 'NONE',  ( 0.000000000000000000, 0.3090169943749411230, 0.9510565162951555296 ) ) ;
#5541 = AXIS2_PLACEMENT_3D ( 'NONE', #21601, #3216, #32142 ) ;
#5542 = CIRCLE ( 'NONE', #45390, 37.49900000000001654 ) ;
#5543 = EDGE_CURVE ( 'NONE', #16459, #10449, #17482, .T. ) ;
#5544 = ORIENTED_EDGE ( 'NONE', *, *, #9725, .F. ) ;
#5545 = DIRECTION ( 'NONE',  ( 0.000000000000000000, 0.000000000000000000, 1.000000000000000000 ) ) ;
#5546 = DIRECTION ( 'NONE',  ( -1.000000000000000000, 0.000000000000000000, -0.000000000000000000 ) ) ;
#5547 = AXIS2_PLACEMENT_3D ( 'NONE', #7132, #44341, #14487 ) ;
#5548 = VERTEX_POINT ( 'NONE', #17677 ) ;
#5549 = VECTOR ( 'NONE', #13236, 1000.000000000000000 ) ;
#5550 = AXIS2_PLACEMENT_3D ( 'NONE', #24670, #27881, #35188 ) ;
#5551 = EDGE_LOOP ( 'NONE', ( #18316, #29263, #16885, #14009 ) ) ;
#5552 = CARTESIAN_POINT ( 'NONE',  ( -0.8815729230226008184, -93.47222532549339746, 5.500000000000000000 ) ) ;
#5553 = ORIENTED_EDGE ( 'NONE', *, *, #21102, .F. ) ;
#5554 = VERTEX_POINT ( 'NONE', #37490 ) ;
#5555 = LINE ( 'NONE', #5080, #18698 ) ;
#5557 = ORIENTED_EDGE ( 'NONE', *, *, #46248, .T. ) ;
#5556 = CARTESIAN_POINT ( 'NONE',  ( 11.99999999999999822, -34.44570377933549565, -69.42325613327476219 ) ) ;
#5558 = ORIENTED_EDGE ( 'NONE', *, *, #10129, .T. ) ;
#5559 = EDGE_LOOP ( 'NONE', ( #29163, #25361 ) ) ;
#5560 = ORIENTED_EDGE ( 'NONE', *, *, #35855, .F. ) ;
#5561 = DIRECTION ( 'NONE',  ( -1.000000000000000000, 0.000000000000000000, 0.000000000000000000 ) ) ;
#5563 = VERTEX_POINT ( 'NONE', #19122 ) ;
#5562 = LINE ( 'NONE', #6061, #13365 ) ;
#5564 = CIRCLE ( 'NONE', #30579, 16.00000000000000000 ) ;
#5565 = DIRECTION ( 'NONE',  ( 0.000000000000000000, -0.6494480483301904306, 0.7604059656000252687 ) ) ;
#5566 = EDGE_CURVE ( 'NONE', #32691, #38387, #18244, .T. ) ;
#5568 = EDGE_LOOP ( 'NONE', ( #47034, #11080, #22029, #17339 ) ) ;
#5567 = AXIS2_PLACEMENT_3D ( 'NONE', #15335, #45182, #41039 ) ;
#5569 = ORIENTED_EDGE ( 'NONE', *, *, #16625, .F. ) ;
#5570 = CARTESIAN_POINT ( 'NONE',  ( 11.99999999999999822, 8.830959090343430518, -74.65491531819107252 ) ) ;
#5571 = VERTEX_POINT ( 'NONE', #40926 ) ;
#5572 = ORIENTED_EDGE ( 'NONE', *, *, #20834, .T. ) ;
#5573 = CARTESIAN_POINT ( 'NONE',  ( -10.00000000000000000, 0.000000000000000000, 0.000000000000000000 ) ) ;
#5574 = VECTOR ( 'NONE', #4666, 1000.000000000000000 ) ;
#5575 = CIRCLE ( 'NONE', #19627, 82.00000000000000000 ) ;
#5576 = DIRECTION ( 'NONE',  ( 0.000000000000000000, 0.000000000000000000, 1.000000000000000000 ) ) ;
#5577 = EDGE_CURVE ( 'NONE', #12155, #4884, #28427, .T. ) ;
#5578 = ORIENTED_EDGE ( 'NONE', *, *, #42683, .F. ) ;
#5579 = CYLINDRICAL_SURFACE ( 'NONE', #29138, 31.99999999999999289 ) ;
#5580 = DIRECTION ( 'NONE',  ( 0.000000000000000000, 0.000000000000000000, 1.000000000000000000 ) ) ;
#5581 = CARTESIAN_POINT ( 'NONE',  ( 12.50000000000000000, -132.5000000000000000, -40.00000000000000000 ) ) ;
#5582 = ADVANCED_FACE ( 'NONE', ( #22329 ), #18869, .T. ) ;
#5583 = VERTEX_POINT ( 'NONE', #41410 ) ;
#5584 = AXIS2_PLACEMENT_3D ( 'NONE', #29099, #24476, #40136 ) ;
#5585 = VERTEX_POINT ( 'NONE', #30398 ) ;
#5586 = DIRECTION ( 'NONE',  ( -1.000000000000000000, 0.000000000000000000, 0.000000000000000000 ) ) ;
#5587 = DIRECTION ( 'NONE',  ( 0.000000000000000000, 0.000000000000000000, 1.000000000000000000 ) ) ;
#5588 = ORIENTED_EDGE ( 'NONE', *, *, #43526, .T. ) ;
#5589 = CARTESIAN_POINT ( 'NONE',  ( 0.000000000000000000, 10.30890764327501152, -81.34940948281325745 ) ) ;
#5590 = ORIENTED_EDGE ( 'NONE', *, *, #32644, .T. ) ;
#5591 = CIRCLE ( 'NONE', #14995, 31.99999999999998934 ) ;
#5592 = DIRECTION ( 'NONE',  ( 0.000000000000000000, -0.8910065241883627918, -0.4539904997395569630 ) ) ;
#5593 = CARTESIAN_POINT ( 'NONE',  ( -3.000000000000000000, 24.81905959214261514, 9.408202855044825341 ) ) ;
#5594 = DIRECTION ( 'NONE',  ( -1.000000000000000000, 0.000000000000000000, 0.000000000000000000 ) ) ;
#5595 = ORIENTED_EDGE ( 'NONE', *, *, #20225, .F. ) ;
#5596 = CARTESIAN_POINT ( 'NONE',  ( 0.000000000000000000, 26.01480285779933510, -70.53064760720289428 ) ) ;
#5597 = EDGE_CURVE ( 'NONE', #44505, #13391, #22063, .T. ) ;
#5598 = EDGE_CURVE ( 'NONE', #4110, #38297, #25980, .T. ) ;
#5599 = EDGE_CURVE ( 'NONE', #17528, #36949, #30779, .T. ) ;
#5600 = DIRECTION ( 'NONE',  ( 0.000000000000000000, 0.3090169943749580539, -0.9510565162951500895 ) ) ;
#5601 = CARTESIAN_POINT ( 'NONE',  ( 0.000000000000000000, 0.000000000000000000, 0.000000000000000000 ) ) ;
#5602 = VECTOR ( 'NONE', #24681, 1000.000000000000000 ) ;
#5603 = VERTEX_POINT ( 'NONE', #7390 ) ;
#5604 = CARTESIAN_POINT ( 'NONE',  ( 0.000000000000000000, 55.38113227695783536, 54.21277698773694453 ) ) ;
#5605 = DIRECTION ( 'NONE',  ( -0.7950889364178796992, 0.6064928550163510845, 0.000000000000000000 ) ) ;
#5606 = FACE_OUTER_BOUND ( 'NONE', #10182, .T. ) ;
#5607 = CARTESIAN_POINT ( 'NONE',  ( -10.00000000000000000, 0.000000000000000000, 0.000000000000000000 ) ) ;
#5608 = ADVANCED_FACE ( 'NONE', ( #37978 ), #37246, .T. ) ;
#5609 = ORIENTED_EDGE ( 'NONE', *, *, #34361, .F. ) ;
#5610 = CIRCLE ( 'NONE', #41555, 31.99999999999999289 ) ;
#5611 = CIRCLE ( 'NONE', #19665, 16.00000000000000355 ) ;
#5612 = EDGE_LOOP ( 'NONE', ( #23396, #38233, #36485, #44859 ) ) ;
#5613 = VECTOR ( 'NONE', #43614, 1000.000000000000000 ) ;
#5614 = AXIS2_PLACEMENT_3D ( 'NONE', #43684, #21882, #25789 ) ;
#5615 = LINE ( 'NONE', #19793, #48368 ) ;
#5616 = FACE_OUTER_BOUND ( 'NONE', #30990, .T. ) ;
#5617 = ORIENTED_EDGE ( 'NONE', *, *, #28139, .T. ) ;
#5618 = AXIS2_PLACEMENT_3D ( 'NONE', #38648, #5112, #45481 ) ;
#5619 = LINE ( 'NONE', #32287, #36654 ) ;
#5620 = VECTOR ( 'NONE', #34691, 1000.000000000000000 ) ;
#5621 = VERTEX_POINT ( 'NONE', #48263 ) ;
#5622 = ORIENTED_EDGE ( 'NONE', *, *, #11274, .F. ) ;
#5623 = VERTEX_POINT ( 'NONE', #11555 ) ;
#5624 = DIRECTION ( 'NONE',  ( 0.000000000000000000, 0.000000000000000000, 1.000000000000000000 ) ) ;
#5625 = ADVANCED_FACE ( 'NONE', ( #4455 ), #34284, .T. ) ;
#5626 = VERTEX_POINT ( 'NONE', #36992 ) ;
#5627 = CARTESIAN_POINT ( 'NONE',  ( 11.99999999999999822, 0.000000000000000000, 0.000000000000000000 ) ) ;
#5628 = EDGE_LOOP ( 'NONE', ( #22431, #25233, #4766, #43478 ) ) ;
#5629 = CARTESIAN_POINT ( 'NONE',  ( 10.00000000000000000, -69.42325613327415113, -34.44570377933673910 ) ) ;
#5630 = EDGE_CURVE ( 'NONE', #40043, #43833, #14740, .T. ) ;
#5631 = AXIS2_PLACEMENT_3D ( 'NONE', #14868, #18036, #37136 ) ;
#5632 = DIRECTION ( 'NONE',  ( 0.000000000000000000, 0.8090169943749486725, -0.5877852522924713607 ) ) ;
#5633 = FACE_OUTER_BOUND ( 'NONE', #32791, .T. ) ;
#5634 = EDGE_CURVE ( 'NONE', #13603, #43495, #8899, .T. ) ;
#5635 = VERTEX_POINT ( 'NONE', #29898 ) ;
#5636 = LINE ( 'NONE', #9529, #41533 ) ;
#5637 = ORIENTED_EDGE ( 'NONE', *, *, #26568, .T. ) ;
#5638 = AXIS2_PLACEMENT_3D ( 'NONE', #26547, #8181, #4285 ) ;
#5639 = CARTESIAN_POINT ( 'NONE',  ( 10.00000000000000000, 0.000000000000000000, 0.000000000000000000 ) ) ;
#5640 = DIRECTION ( 'NONE',  ( -1.000000000000000000, -0.000000000000000000, -0.000000000000000000 ) ) ;
#5641 = DIRECTION ( 'NONE',  ( 1.000000000000000000, 0.000000000000000000, -0.000000000000000000 ) ) ;
#5642 = VERTEX_POINT ( 'NONE', #44830 ) ;
#5643 = ORIENTED_EDGE ( 'NONE', *, *, #37797, .F. ) ;
#5644 = DIRECTION ( 'NONE',  ( -0.000000000000000000, -0.000000000000000000, -1.000000000000000000 ) ) ;
#5645 = DIRECTION ( 'NONE',  ( -1.000000000000000000, -0.000000000000000000, -0.000000000000000000 ) ) ;
#5646 = ORIENTED_EDGE ( 'NONE', *, *, #8069, .F. ) ;
#5647 = CYLINDRICAL_SURFACE ( 'NONE', #19109, 31.99999999999998579 ) ;
#5648 = CYLINDRICAL_SURFACE ( 'NONE', #39975, 37.49900000000000233 ) ;
#5649 = LINE ( 'NONE', #8581, #41714 ) ;
#5650 = CARTESIAN_POINT ( 'NONE',  ( 11.99999999999999822, 0.000000000000000000, 0.000000000000000000 ) ) ;
#5651 = VECTOR ( 'NONE', #41237, 1000.000000000000000 ) ;
#5652 = EDGE_CURVE ( 'NONE', #25578, #23496, #11318, .T. ) ;
#5653 = CARTESIAN_POINT ( 'NONE',  ( 10.00000000000000000, 0.000000000000000000, 0.000000000000000000 ) ) ;
#5654 = EDGE_CURVE ( 'NONE', #19037, #14039, #22563, .T. ) ;
#5655 = DIRECTION ( 'NONE',  ( 0.000000000000000000, 0.000000000000000000, 1.000000000000000000 ) ) ;
#5656 = CARTESIAN_POINT ( 'NONE',  ( 10.00000000000000000, 77.16300072079698680, -27.74655509720590274 ) ) ;
#5657 = CARTESIAN_POINT ( 'NONE',  ( 0.000000000000000000, -13.04903810567675038, 19.60159698893425428 ) ) ;
#5658 = CARTESIAN_POINT ( 'NONE',  ( 0.000000000000000000, -55.20638768913724448, -51.02545421589383068 ) ) ;
#5659 = VECTOR ( 'NONE', #44915, 1000.000000000000000 ) ;
#5660 = CARTESIAN_POINT ( 'NONE',  ( 11.99999999999999822, -77.49459641780886443, 0.8261519478428549501 ) ) ;
#5661 = FACE_OUTER_BOUND ( 'NONE', #14431, .T. ) ;
#5662 =( LENGTH_UNIT ( ) NAMED_UNIT ( * ) SI_UNIT ( .MILLI., .METRE. ) );
#5663 = CYLINDRICAL_SURFACE ( 'NONE', #37419, 82.00000000000000000 ) ;
#5664 = CARTESIAN_POINT ( 'NONE',  ( 18.80329974962065265, -105.8248132807389084, 5.500000000000000000 ) ) ;
#5665 = ORIENTED_EDGE ( 'NONE', *, *, #36527, .T. ) ;
#5666 = ADVANCED_FACE ( 'NONE', ( #3468 ), #33800, .F. ) ;
#5667 = ORIENTED_EDGE ( 'NONE', *, *, #11888, .F. ) ;
#5668 = CARTESIAN_POINT ( 'NONE',  ( 15.00000000000000000, -23.29833615347104470, 3.418703333116808629 ) ) ;
#5669 = FACE_OUTER_BOUND ( 'NONE', #47908, .T. ) ;
#5670 = CARTESIAN_POINT ( 'NONE',  ( 11.99999999999999822, 31.47745569255140552, 68.26794271651274926 ) ) ;
#5671 = ORIENTED_EDGE ( 'NONE', *, *, #3924, .T. ) ;
#5672 = CIRCLE ( 'NONE', #11153, 14.09999999999999964 ) ;
#5673 = AXIS2_PLACEMENT_3D ( 'NONE', #11055, #29893, #21820 ) ;
#5674 = CARTESIAN_POINT ( 'NONE',  ( 10.00000000000000000, 4.992566952384984269, 37.16516213103279398 ) ) ;
#5675 = AXIS2_PLACEMENT_3D ( 'NONE', #29049, #43981, #36631 ) ;
#5676 = VERTEX_POINT ( 'NONE', #15231 ) ;
#5677 = LINE ( 'NONE', #9342, #39374 ) ;
#5678 = ORIENTED_EDGE ( 'NONE', *, *, #29615, .T. ) ;
#5679 = DIRECTION ( 'NONE',  ( 0.000000000000000000, 0.000000000000000000, -1.000000000000000000 ) ) ;
#5680 = AXIS2_PLACEMENT_3D ( 'NONE', #31190, #45142, #45874 ) ;
#5681 = FACE_OUTER_BOUND ( 'NONE', #28482, .T. ) ;
#5682 = AXIS2_PLACEMENT_3D ( 'NONE', #37117, #3589, #41054 ) ;
#5683 = DIRECTION ( 'NONE',  ( -0.000000000000000000, -0.8660254037844427044, 0.4999999999999929501 ) ) ;
#5684 = ORIENTED_EDGE ( 'NONE', *, *, #1530, .F. ) ;
#5685 = CARTESIAN_POINT ( 'NONE',  ( 23.11608002360578240, -124.4885236261218182, -5.500000000000000000 ) ) ;
#5686 = ORIENTED_EDGE ( 'NONE', *, *, #33838, .F. ) ;
#5687 = EDGE_CURVE ( 'NONE', #17817, #26988, #23739, .T. ) ;
#5688 = EDGE_CURVE ( 'NONE', #41344, #44547, #7145, .T. ) ;
#5689 = DIRECTION ( 'NONE',  ( 0.000000000000000000, 0.000000000000000000, 1.000000000000000000 ) ) ;
#5690 = EDGE_CURVE ( 'NONE', #13195, #2592, #45812, .T. ) ;
#5691 = CARTESIAN_POINT ( 'NONE',  ( 0.000000000000000000, -74.74816331893404708, -33.71516098798818462 ) ) ;
#5692 = DIRECTION ( 'NONE',  ( 0.000000000000000000, -0.9510565162951503115, 0.3090169943749573878 ) ) ;
#5694 = ORIENTED_EDGE ( 'NONE', *, *, #6574, .T. ) ;
#5693 = DIRECTION ( 'NONE',  ( -1.000000000000000000, 0.000000000000000000, 0.000000000000000000 ) ) ;
#5695 = ORIENTED_EDGE ( 'NONE', *, *, #41246, .T. ) ;
#5696 = DIRECTION ( 'NONE',  ( 0.000000000000000000, 0.000000000000000000, 1.000000000000000000 ) ) ;
#5697 = ORIENTED_EDGE ( 'NONE', *, *, #36367, .T. ) ;
#5698 = EDGE_CURVE ( 'NONE', #26745, #38886, #5649, .T. ) ;
#5699 = DIRECTION ( 'NONE',  ( -1.000000000000000000, -0.000000000000000000, -0.000000000000000000 ) ) ;
#5700 = VERTEX_POINT ( 'NONE', #46048 ) ;
#5701 = CARTESIAN_POINT ( 'NONE',  ( 10.00000000000000000, -31.47745569255189224, 68.26794271651249346 ) ) ;
#5702 = DIRECTION ( 'NONE',  ( 0.000000000000000000, 0.000000000000000000, 1.000000000000000000 ) ) ;
#5703 = CARTESIAN_POINT ( 'NONE',  ( 12.50000000000000000, -132.5000000000000000, -2.500000000000000000 ) ) ;
#5704 = ORIENTED_EDGE ( 'NONE', *, *, #31177, .T. ) ;
#5705 = CARTESIAN_POINT ( 'NONE',  ( 10.00000000000000000, -35.92658777277502935, -10.74501242461320594 ) ) ;
#5706 = AXIS2_PLACEMENT_3D ( 'NONE', #39512, #10353, #25270 ) ;
#5707 = FACE_OUTER_BOUND ( 'NONE', #9682, .T. ) ;
#5708 = CARTESIAN_POINT ( 'NONE',  ( 10.00000000000000000, 0.000000000000000000, 0.000000000000000000 ) ) ;
#5709 = EDGE_CURVE ( 'NONE', #15060, #34499, #20592, .T. ) ;
#5710 = AXIS2_PLACEMENT_3D ( 'NONE', #483, #10775, #37440 ) ;
#5711 = CARTESIAN_POINT ( 'NONE',  ( 0.000000000000000000, 10.30890764327501863, -81.34940948281325745 ) ) ;
#5712 = LINE ( 'NONE', #32387, #6738 ) ;
#5713 = AXIS2_PLACEMENT_3D ( 'NONE', #528, #26713, #20814 ) ;
#5714 = CARTESIAN_POINT ( 'NONE',  ( 10.00000000000000000, 14.67089635893713684, 73.72996012237443608 ) ) ;
#5715 = EDGE_CURVE ( 'NONE', #18510, #39232, #16421, .T. ) ;
#5716 = DIRECTION ( 'NONE',  ( 0.000000000000000000, 0.000000000000000000, -1.000000000000000000 ) ) ;
#5718 = FACE_OUTER_BOUND ( 'NONE', #42996, .T. ) ;
#5717 = APPLICATION_CONTEXT ( 'automotive_design' ) ;
#5719 = CIRCLE ( 'NONE', #16683, 16.00000000000000000 ) ;
#5720 = DIRECTION ( 'NONE',  ( -1.000000000000000000, -0.000000000000000000, 0.000000000000000000 ) ) ;
#5721 = DIRECTION ( 'NONE',  ( 1.000000000000000000, 0.000000000000000000, 0.000000000000000000 ) ) ;
#5722 = VECTOR ( 'NONE', #13180, 1000.000000000000000 ) ;
#5723 = VERTEX_POINT ( 'NONE', #9083 ) ;
#5724 = EDGE_CURVE ( 'NONE', #20650, #8981, #22167, .T. ) ;
#5725 = ORIENTED_EDGE ( 'NONE', *, *, #40549, .F. ) ;
#5726 = CARTESIAN_POINT ( 'NONE',  ( 15.00000000000000000, -14.54903810567644484, 22.19967320028775504 ) ) ;
#5727 = EDGE_LOOP ( 'NONE', ( #17634, #31035, #39140, #28125 ) ) ;
#5728 = CARTESIAN_POINT ( 'NONE',  ( 5.000000000000000000, -35.47612816024506088, -22.48208911017539435 ) ) ;
#5729 = VECTOR ( 'NONE', #17453, 1000.000000000000000 ) ;
#5730 = CARTESIAN_POINT ( 'NONE',  ( 0.000000000000000000, 0.000000000000000000, -43.79999999999998295 ) ) ;
#5731 = ORIENTED_EDGE ( 'NONE', *, *, #46316, .T. ) ;
#5732 = EDGE_CURVE ( 'NONE', #25011, #5981, #26859, .T. ) ;
#5733 = EDGE_LOOP ( 'NONE', ( #2894, #20657, #21930, #1720 ) ) ;
#5734 = FACE_OUTER_BOUND ( 'NONE', #32633, .T. ) ;
#5735 = ORIENTED_EDGE ( 'NONE', *, *, #44041, .T. ) ;
#5736 = AXIS2_PLACEMENT_3D ( 'NONE', #9816, #44064, #10544 ) ;
#5737 = EDGE_LOOP ( 'NONE', ( #9581, #5000, #46264, #37084 ) ) ;
#5738 = ORIENTED_EDGE ( 'NONE', *, *, #32337, .T. ) ;
#5739 = VECTOR ( 'NONE', #36939, 1000.000000000000000 ) ;
#5740 = CARTESIAN_POINT ( 'NONE',  ( 15.00000000000000000, 18.84667830672605859, 18.68964196561243796 ) ) ;
#5741 = ADVANCED_FACE ( 'NONE', ( #20092 ), #15944, .T. ) ;
#5742 = DIRECTION ( 'NONE',  ( -1.000000000000000000, -0.000000000000000000, 0.000000000000000000 ) ) ;
#5743 = AXIS2_PLACEMENT_3D ( 'NONE', #11044, #44335, #33320 ) ;
#5744 = FACE_BOUND ( 'NONE', #42512, .T. ) ;
#5745 = VECTOR ( 'NONE', #24036, 1000.000000000000000 ) ;
#5746 = ORIENTED_EDGE ( 'NONE', *, *, #13295, .T. ) ;
#5747 = EDGE_CURVE ( 'NONE', #9118, #21044, #37796, .T. ) ;
#5748 = CARTESIAN_POINT ( 'NONE',  ( 0.000000000000000000, 0.000000000000000000, 0.000000000000000000 ) ) ;
#5749 = AXIS2_PLACEMENT_3D ( 'NONE', #47639, #6538, #10203 ) ;
#5750 = VECTOR ( 'NONE', #23643, 1000.000000000000000 ) ;
#5751 = ORIENTED_EDGE ( 'NONE', *, *, #29832, .T. ) ;
#5752 = ADVANCED_FACE ( 'NONE', ( #16908 ), #34774, .T. ) ;
#5753 = DIRECTION ( 'NONE',  ( -1.000000000000000000, 0.000000000000000000, 0.000000000000000000 ) ) ;
#5754 = DIRECTION ( 'NONE',  ( 1.000000000000000000, -0.000000000000000000, -0.000000000000000000 ) ) ;
#5755 = FACE_OUTER_BOUND ( 'NONE', #35617, .T. ) ;
#5756 = CIRCLE ( 'NONE', #2621, 82.00000000000000000 ) ;
#5757 = CIRCLE ( 'NONE', #22164, 37.49900000000000944 ) ;
#5758 = ORIENTED_EDGE ( 'NONE', *, *, #29347, .T. ) ;
#5759 = ORIENTED_EDGE ( 'NONE', *, *, #23600, .F. ) ;
#5760 = DIRECTION ( 'NONE',  ( -1.000000000000000000, -0.000000000000000000, -0.000000000000000000 ) ) ;
#5761 = ORIENTED_EDGE ( 'NONE', *, *, #40237, .F. ) ;
#5762 = ADVANCED_FACE ( 'NONE', ( #27446 ), #16194, .T. ) ;
#5763 = VECTOR ( 'NONE', #5177, 1000.000000000000000 ) ;
#5764 = PLANE ( 'NONE',  #17590 ) ;
#5765 = VECTOR ( 'NONE', #4704, 1000.000000000000000 ) ;
#5766 = CARTESIAN_POINT ( 'NONE',  ( 5.000000000000002665, 34.94270380257741948, -74.18225833017852722 ) ) ;
#5767 = CARTESIAN_POINT ( 'NONE',  ( 10.00000000000000000, 37.48860685352291000, -0.8828120875901940279 ) ) ;
#5768 = DIRECTION ( 'NONE',  ( -1.000000000000000000, -0.000000000000000000, 0.000000000000000000 ) ) ;
#5769 = FACE_OUTER_BOUND ( 'NONE', #1633, .T. ) ;
#5770 = AXIS2_PLACEMENT_3D ( 'NONE', #14939, #30840, #7824 ) ;
#5771 = CARTESIAN_POINT ( 'NONE',  ( 4.999999999999999112, -40.68715046381937128, 10.41901085202062660 ) ) ;
#5772 = CARTESIAN_POINT ( 'NONE',  ( -3.702536634196095910, 8.043911037661889196, 42.00000000000001421 ) ) ;
#5773 = LINE ( 'NONE', #6022, #30083 ) ;
#5774 = DIRECTION ( 'NONE',  ( 0.000000000000000000, -0.8090169943749531134, 0.5877852522924654766 ) ) ;
#5775 = DIRECTION ( 'NONE',  ( -1.000000000000000000, -0.000000000000000000, -0.000000000000000000 ) ) ;
#5776 = ORIENTED_EDGE ( 'NONE', *, *, #12444, .T. ) ;
#5777 = VERTEX_POINT ( 'NONE', #39177 ) ;
#5778 = FACE_OUTER_BOUND ( 'NONE', #5150, .T. ) ;
#5779 = FACE_OUTER_BOUND ( 'NONE', #5159, .T. ) ;
#5780 = DIRECTION ( 'NONE',  ( 0.000000000000000000, 0.07845909572784529051, -0.9969173337331279638 ) ) ;
#5781 = DIRECTION ( 'NONE',  ( 0.000000000000000000, 0.000000000000000000, 1.000000000000000000 ) ) ;
#5783 = AXIS2_PLACEMENT_3D ( 'NONE', #33233, #40573, #48159 ) ;
#5782 = CARTESIAN_POINT ( 'NONE',  ( 10.00000000000000000, 37.22597642581150268, 5.202137450157037435 ) ) ;
#5784 = ORIENTED_EDGE ( 'NONE', *, *, #18304, .F. ) ;
#5785 = CIRCLE ( 'NONE', #17504, 31.99999999999999289 ) ;
#5786 = CARTESIAN_POINT ( 'NONE',  ( 10.00000000000000000, 0.000000000000000000, 0.000000000000000000 ) ) ;
#5787 = DIRECTION ( 'NONE',  ( 0.000000000000000000, 0.8090169943749446757, 0.5877852522924769119 ) ) ;
#5788 = ORIENTED_EDGE ( 'NONE', *, *, #35521, .T. ) ;
#5789 = AXIS2_PLACEMENT_3D ( 'NONE', #3772, #587, #7685 ) ;
#5791 = CIRCLE ( 'NONE', #44871, 15.99999999999999467 ) ;
#5790 = DIRECTION ( 'NONE',  ( -1.000000000000000000, 0.000000000000000000, 0.000000000000000000 ) ) ;
#5792 = CIRCLE ( 'NONE', #22963, 42.00000000000000000 ) ;
#5793 = VERTEX_POINT ( 'NONE', #1991 ) ;
#5794 = PRODUCT_DEFINITION_SHAPE ( 'NONE', 'NONE',  #12192 ) ;
#5795 = FILL_AREA_STYLE ('',( #43890 ) ) ;
#5796 = CARTESIAN_POINT ( 'NONE',  ( 0.000000000000000000, 16.65972982745045528, -80.28980883073738539 ) ) ;
#5797 = ORIENTED_EDGE ( 'NONE', *, *, #35027, .F. ) ;
#5798 = ORIENTED_EDGE ( 'NONE', *, *, #3741, .F. ) ;
#5799 = ORIENTED_EDGE ( 'NONE', *, *, #29284, .F. ) ;
#5800 = AXIS2_PLACEMENT_3D ( 'NONE', #40812, #18289, #166 ) ;
#5801 = AXIS2_PLACEMENT_3D ( 'NONE', #44843, #3976, #34063 ) ;
#5802 = CIRCLE ( 'NONE', #12064, 31.99999999999998579 ) ;
#5803 = ORIENTED_EDGE ( 'NONE', *, *, #3360, .F. ) ;
#5804 = AXIS2_PLACEMENT_3D ( 'NONE', #8544, #26441, #11273 ) ;
#5805 = CARTESIAN_POINT ( 'NONE',  ( 10.00000000000000000, 59.46389618801964616, 49.70050353004912580 ) ) ;
#5806 = ORIENTED_EDGE ( 'NONE', *, *, #16234, .T. ) ;
#5807 = AXIS2_PLACEMENT_3D ( 'NONE', #41210, #37517, #34085 ) ;
#5808 = ORIENTED_EDGE ( 'NONE', *, *, #3989, .T. ) ;
#5809 = ADVANCED_FACE ( 'NONE', ( #4681 ), #35505, .T. ) ;
#5810 = DIRECTION ( 'NONE',  ( -1.000000000000000000, 0.000000000000000000, 0.000000000000000000 ) ) ;
#5811 = DIRECTION ( 'NONE',  ( 0.000000000000000000, -0.9135454576426055295, -0.4067366430757899942 ) ) ;
#5812 = ORIENTED_EDGE ( 'NONE', *, *, #11873, .F. ) ;
#5813 = ORIENTED_EDGE ( 'NONE', *, *, #31030, .F. ) ;
#5814 = ADVANCED_FACE ( 'NONE', ( #5407 ), #31124, .F. ) ;
#5815 = ORIENTED_EDGE ( 'NONE', *, *, #30132, .F. ) ;
#5816 = DIRECTION ( 'NONE',  ( 1.000000000000000000, 0.000000000000000000, 0.000000000000000000 ) ) ;
#5818 = ORIENTED_EDGE ( 'NONE', *, *, #35905, .F. ) ;
#5817 = LINE ( 'NONE', #31529, #20367 ) ;
#5820 = FACE_OUTER_BOUND ( 'NONE', #30672, .T. ) ;
#5819 = AXIS2_PLACEMENT_3D ( 'NONE', #18337, #28869, #24958 ) ;
#5821 = ORIENTED_EDGE ( 'NONE', *, *, #40835, .T. ) ;
#5822 = VERTEX_POINT ( 'NONE', #26969 ) ;
#5823 = ORIENTED_EDGE ( 'NONE', *, *, #1501, .T. ) ;
#5824 = CARTESIAN_POINT ( 'NONE',  ( -10.00000000000000000, 0.000000000000000000, 0.000000000000000000 ) ) ;
#5825 = ORIENTED_EDGE ( 'NONE', *, *, #23074, .T. ) ;
#5826 = EDGE_CURVE ( 'NONE', #40027, #23243, #41901, .T. ) ;
#5827 = FACE_OUTER_BOUND ( 'NONE', #25533, .T. ) ;
#5828 = AXIS2_PLACEMENT_3D ( 'NONE', #15167, #41587, #30093 ) ;
#5829 = DIRECTION ( 'NONE',  ( 0.000000000000000000, 0.000000000000000000, 1.000000000000000000 ) ) ;
#5830 = CIRCLE ( 'NONE', #36312, 31.99999999999998579 ) ;
#5831 = ADVANCED_FACE ( 'NONE', ( #8823 ), #38218, .T. ) ;
#5832 = CARTESIAN_POINT ( 'NONE',  ( 0.000000000000000000, -21.40280677340398086, 36.13751322684410638 ) ) ;
#5833 = CARTESIAN_POINT ( 'NONE',  ( 10.00000000000000000, -10.96151621346514382, 35.95386929396252640 ) ) ;
#5834 = CIRCLE ( 'NONE', #1018, 31.99999999999999645 ) ;
#5835 = CARTESIAN_POINT ( 'NONE',  ( 11.99999999999999822, 81.34940948281349904, -10.30890764327296161 ) ) ;
#5836 = VERTEX_POINT ( 'NONE', #35256 ) ;
#5837 = ORIENTED_EDGE ( 'NONE', *, *, #25334, .T. ) ;
#5838 = FACE_OUTER_BOUND ( 'NONE', #27016, .T. ) ;
#5839 = CYLINDRICAL_SURFACE ( 'NONE', #11063, 16.00000000000000000 ) ;
#5840 = ORIENTED_EDGE ( 'NONE', *, *, #33575, .T. ) ;
#5841 = CIRCLE ( 'NONE', #39449, 31.99999999999998934 ) ;
#5842 = CARTESIAN_POINT ( 'NONE',  ( 6.000000000000000000, 3.894527615419050903, -81.90746397400384637 ) ) ;
#5843 = ORIENTED_EDGE ( 'NONE', *, *, #27190, .T. ) ;
#5844 = AXIS2_PLACEMENT_3D ( 'NONE', #31574, #46498, #1955 ) ;
#5845 = CARTESIAN_POINT ( 'NONE',  ( 11.99999999999999822, 77.19088730480524418, 6.903761155838049390 ) ) ;
#5846 = CARTESIAN_POINT ( 'NONE',  ( 22.08297821871651934, -111.8242998470044540, 2.500000000000000000 ) ) ;
#5847 = DIRECTION ( 'NONE',  ( 0.000000000000000000, 0.8910065241883656784, 0.4539904997395511899 ) ) ;
#5848 = CARTESIAN_POINT ( 'NONE',  ( 5.999999999999999112, 63.97538442413498672, -51.29473840253155004 ) ) ;
#5849 = AXIS2_PLACEMENT_3D ( 'NONE', #31087, #23718, #9040 ) ;
#5850 = EDGE_CURVE ( 'NONE', #29983, #25935, #1736, .T. ) ;
#5851 = DIRECTION ( 'NONE',  ( 0.000000000000000000, 0.000000000000000000, 1.000000000000000000 ) ) ;
#5852 = DIRECTION ( 'NONE',  ( -0.000000000000000000, 0.1045284632676570929, -0.9945218953682730678 ) ) ;
#5853 = ORIENTED_EDGE ( 'NONE', *, *, #22758, .T. ) ;
#5854 = CARTESIAN_POINT ( 'NONE',  ( 0.000000000000000000, -29.81001611430991360, -22.74946021919165418 ) ) ;
#5855 = DIRECTION ( 'NONE',  ( -1.000000000000000000, 0.000000000000000000, -0.000000000000000000 ) ) ;
#5856 = DIRECTION ( 'NONE',  ( -0.2867529058022035837, 0.9580045777625452175, 0.000000000000000000 ) ) ;
#5857 = DIRECTION ( 'NONE',  ( 1.000000000000000000, 0.000000000000000000, 0.000000000000000000 ) ) ;
#5858 = ORIENTED_EDGE ( 'NONE', *, *, #39558, .F. ) ;
#5859 = ORIENTED_EDGE ( 'NONE', *, *, #4960, .T. ) ;
#5860 = CIRCLE ( 'NONE', #41806, 16.00000000000000000 ) ;
#5861 = ADVANCED_FACE ( 'NONE', ( #39429 ), #47480, .T. ) ;
#5862 = AXIS2_PLACEMENT_3D ( 'NONE', #3806, #46746, #47856 ) ;
#5863 = VECTOR ( 'NONE', #12303, 1000.000000000000000 ) ;
#5864 = ADVANCED_FACE ( 'NONE', ( #29110 ), #21047, .T. ) ;
#5865 = DIRECTION ( 'NONE',  ( -1.000000000000000000, -0.000000000000000000, -0.000000000000000000 ) ) ;
#5866 = CARTESIAN_POINT ( 'NONE',  ( 10.00000000000000000, 33.00180498840072829, -17.80606268964504935 ) ) ;
#5867 = EDGE_CURVE ( 'NONE', #43255, #34359, #2439, .T. ) ;
#5868 = ORIENTED_EDGE ( 'NONE', *, *, #20704, .F. ) ;
#5869 = AXIS2_PLACEMENT_3D ( 'NONE', #10860, #18440, #29216 ) ;
#5870 = AXIS2_PLACEMENT_3D ( 'NONE', #28544, #29007, #28290 ) ;
#5871 = CARTESIAN_POINT ( 'NONE',  ( 0.000000000000000000, -27.13269053701114331, 25.88420570971391754 ) ) ;
#5872 = ORIENTED_EDGE ( 'NONE', *, *, #45236, .F. ) ;
#5873 = ORIENTED_EDGE ( 'NONE', *, *, #2453, .T. ) ;
#5874 = ORIENTED_EDGE ( 'NONE', *, *, #25487, .F. ) ;
#5875 = ADVANCED_FACE ( 'NONE', ( #9796 ), #40149, .F. ) ;
#5876 = AXIS2_PLACEMENT_3D ( 'NONE', #6731, #10396, #47589 ) ;
#5877 = ADVANCED_FACE ( 'NONE', ( #6374 ), #21539, .T. ) ;
#5878 = ADVANCED_FACE ( 'NONE', ( #43093 ), #43806, .F. ) ;
#5879 = CARTESIAN_POINT ( 'NONE',  ( 11.99999999999999822, -12.93880638057369659, 76.41127070299266677 ) ) ;
#5880 = VERTEX_POINT ( 'NONE', #47245 ) ;
#5881 = LINE ( 'NONE', #17830, #20780 ) ;
#5882 = ORIENTED_EDGE ( 'NONE', *, *, #31157, .T. ) ;
#5883 = DIRECTION ( 'NONE',  ( -1.000000000000000000, -0.000000000000000000, -0.000000000000000000 ) ) ;
#5884 = CIRCLE ( 'NONE', #44200, 31.99999999999999289 ) ;
#5885 = EDGE_CURVE ( 'NONE', #7382, #8218, #4992, .T. ) ;
#5886 = LINE ( 'NONE', #46989, #10593 ) ;
#5887 = CARTESIAN_POINT ( 'NONE',  ( 10.00000000000000000, -62.50329211542407393, -41.76937507738853839 ) ) ;
#5888 = ORIENTED_EDGE ( 'NONE', *, *, #40747, .T. ) ;
#5889 = DIRECTION ( 'NONE',  ( -1.000000000000000000, -0.000000000000000000, -0.000000000000000000 ) ) ;
#5890 = ORIENTED_EDGE ( 'NONE', *, *, #15873, .T. ) ;
#5891 = CARTESIAN_POINT ( 'NONE',  ( 11.99999999999999822, -63.18004540532995605, -44.88180994100445531 ) ) ;
#5892 = VECTOR ( 'NONE', #13069, 1000.000000000000000 ) ;
#5893 = DIRECTION ( 'NONE',  ( 0.000000000000000000, 0.000000000000000000, -1.000000000000000000 ) ) ;
#5894 = DIRECTION ( 'NONE',  ( -1.000000000000000000, 0.000000000000000000, 0.000000000000000000 ) ) ;
#5895 = ORIENTED_EDGE ( 'NONE', *, *, #43508, .T. ) ;
#5896 = VERTEX_POINT ( 'NONE', #2928 ) ;
#5897 = DIRECTION ( 'NONE',  ( 1.000000000000000000, 0.000000000000000000, 0.000000000000000000 ) ) ;
#5898 = CARTESIAN_POINT ( 'NONE',  ( 10.00000000000000000, -27.05870788708213226, -26.08949754953053102 ) ) ;
#5899 = EDGE_LOOP ( 'NONE', ( #25906, #16174, #28832, #23449 ) ) ;
#5900 = DIRECTION ( 'NONE',  ( -1.000000000000000000, 0.000000000000000000, 0.000000000000000000 ) ) ;
#5901 = DIRECTION ( 'NONE',  ( -1.000000000000000000, 0.000000000000000000, 0.000000000000000000 ) ) ;
#5902 = CARTESIAN_POINT ( 'NONE',  ( 11.99999999999999822, -65.59268652807237743, 36.72794159290217664 ) ) ;
#5903 = CARTESIAN_POINT ( 'NONE',  ( 11.99999999999999822, -20.40083707022935400, 72.35432306680478121 ) ) ;
#5904 = CYLINDRICAL_SURFACE ( 'NONE', #24764, 82.00000000000000000 ) ;
#5905 = VERTEX_POINT ( 'NONE', #44050 ) ;
#5906 = VECTOR ( 'NONE', #47042, 1000.000000000000000 ) ;
#5907 = VECTOR ( 'NONE', #22630, 1000.000000000000000 ) ;
#5908 = DIRECTION ( 'NONE',  ( 0.08130631524010120681, -0.9966891607226784355, 0.000000000000000000 ) ) ;
#5909 = CARTESIAN_POINT ( 'NONE',  ( -3.000000000000000000, -1.278221433540502217, 26.51162292216071847 ) ) ;
#5910 = VECTOR ( 'NONE', #14434, 1000.000000000000000 ) ;
#5911 = CYLINDRICAL_SURFACE ( 'NONE', #9605, 82.00000000000000000 ) ;
#5912 = DIRECTION ( 'NONE',  ( -1.000000000000000000, -0.000000000000000000, -0.000000000000000000 ) ) ;
#5913 = DIRECTION ( 'NONE',  ( -0.4796670183876317051, 0.8774505977381972244, 0.000000000000000000 ) ) ;
#5914 = LINE ( 'NONE', #39194, #20232 ) ;
#5915 = VECTOR ( 'NONE', #43201, 1000.000000000000000 ) ;
#5916 = DIRECTION ( 'NONE',  ( 1.000000000000000000, 0.000000000000000000, 0.000000000000000000 ) ) ;
#5917 = CIRCLE ( 'NONE', #23899, 77.49899999999999523 ) ;
#5918 = VERTEX_POINT ( 'NONE', #13720 ) ;
#5919 = ADVANCED_FACE ( 'NONE', ( #10035 ), #9544, .T. ) ;
#5920 = VERTEX_POINT ( 'NONE', #17616 ) ;
#5921 = ADVANCED_FACE ( 'NONE', ( #39679 ), #28649, .T. ) ;
#5922 = DIRECTION ( 'NONE',  ( 0.000000000000000000, 0.000000000000000000, -1.000000000000000000 ) ) ;
#5923 = DIRECTION ( 'NONE',  ( -0.7533909544171997208, -0.6575728627325955200, 0.000000000000000000 ) ) ;
#5924 = ADVANCED_FACE ( 'NONE', ( #32558 ), #13950, .T. ) ;
#5925 = VERTEX_POINT ( 'NONE', #25191 ) ;
#5926 = AXIS2_PLACEMENT_3D ( 'NONE', #6560, #21491, #47195 ) ;
#5927 = DIRECTION ( 'NONE',  ( 0.000000000000000000, 0.1564344650402242909, 0.9876883405951387696 ) ) ;
#5928 = ADVANCED_FACE ( 'NONE', ( #40392 ), #47702, .T. ) ;
#5929 = ORIENTED_EDGE ( 'NONE', *, *, #19813, .F. ) ;
#5930 = ORIENTED_EDGE ( 'NONE', *, *, #8418, .T. ) ;
#5931 = CARTESIAN_POINT ( 'NONE',  ( 11.99999999999999822, -68.27212725128298132, 31.46837873494953541 ) ) ;
#5932 = ORIENTED_EDGE ( 'NONE', *, *, #2688, .T. ) ;
#5933 = DIRECTION ( 'NONE',  ( -1.000000000000000000, 0.000000000000000000, 0.000000000000000000 ) ) ;
#5934 = ORIENTED_EDGE ( 'NONE', *, *, #17328, .F. ) ;
#5935 = DIRECTION ( 'NONE',  ( -1.000000000000000000, 0.000000000000000000, 0.000000000000000000 ) ) ;
#5936 = VERTEX_POINT ( 'NONE', #32086 ) ;
#5937 = EDGE_CURVE ( 'NONE', #44520, #26821, #25304, .T. ) ;
#5938 = EDGE_CURVE ( 'NONE', #18327, #5156, #3158, .T. ) ;
#5939 = DIRECTION ( 'NONE',  ( -1.000000000000000000, -0.000000000000000000, 0.000000000000000000 ) ) ;
#5940 = LINE ( 'NONE', #2028, #36757 ) ;
#5941 = VERTEX_POINT ( 'NONE', #7807 ) ;
#5943 = ORIENTED_EDGE ( 'NONE', *, *, #4510, .T. ) ;
#5942 = LINE ( 'NONE', #2480, #30920 ) ;
#5944 = ORIENTED_EDGE ( 'NONE', *, *, #25904, .F. ) ;
#5945 = CIRCLE ( 'NONE', #33282, 31.99999999999998579 ) ;
#5946 = CARTESIAN_POINT ( 'NONE',  ( 11.99999999999999822, 66.50666863322055633, -39.78640506895536078 ) ) ;
#5947 = CIRCLE ( 'NONE', #44997, 15.99999999999999822 ) ;
#5948 = LINE ( 'NONE', #21329, #18310 ) ;
#5949 = CARTESIAN_POINT ( 'NONE',  ( 15.00000000000000000, 23.59884966291521380, -12.14883922797262805 ) ) ;
#5950 = EDGE_CURVE ( 'NONE', #15783, #22304, #35485, .T. ) ;
#5952 = ORIENTED_EDGE ( 'NONE', *, *, #22880, .T. ) ;
#5951 = FACE_OUTER_BOUND ( 'NONE', #23753, .T. ) ;
#5953 = CYLINDRICAL_SURFACE ( 'NONE', #27002, 82.00000000000000000 ) ;
#5954 = ORIENTED_EDGE ( 'NONE', *, *, #8328, .F. ) ;
#5955 = CARTESIAN_POINT ( 'NONE',  ( 0.000000000000000000, -81.90746397400393164, 3.894527615417586741 ) ) ;
#5956 = ORIENTED_EDGE ( 'NONE', *, *, #1034, .F. ) ;
#5957 = SHAPE_REPRESENTATION ( 'BR-543', ( #13179, #6922, #28027, #43645, #40528, #25654, #4580, #45994, #44410, #24110, #10839, #30372, #22534, #38188, #17083, #38971, #36601 ), #34258 ) ;
#5958 = DIRECTION ( 'NONE',  ( 1.000000000000000000, 0.000000000000000000, 0.000000000000000000 ) ) ;
#5959 = CYLINDRICAL_SURFACE ( 'NONE', #4323, 31.99999999999999289 ) ;
#5960 = AXIS2_PLACEMENT_3D ( 'NONE', #20572, #1999, #5185 ) ;
#5961 = DIRECTION ( 'NONE',  ( -1.000000000000000000, 0.000000000000000000, 0.000000000000000000 ) ) ;
#5962 = CARTESIAN_POINT ( 'NONE',  ( 19.12409105625795291, -101.5943176906707919, 5.500000000000000000 ) ) ;
#5963 = ORIENTED_EDGE ( 'NONE', *, *, #28703, .T. ) ;
#5964 = DIRECTION ( 'NONE',  ( -1.000000000000000000, 0.000000000000000000, -0.000000000000000000 ) ) ;
#5965 = AXIS2_PLACEMENT_3D ( 'NONE', #21668, #37073, #18476 ) ;
#5966 = LINE ( 'NONE', #1795, #2588 ) ;
#5967 = DIRECTION ( 'NONE',  ( -1.000000000000000000, -0.000000000000000000, -0.000000000000000000 ) ) ;
#5968 = DIRECTION ( 'NONE',  ( -1.000000000000000000, -0.000000000000000000, 0.000000000000000000 ) ) ;
#5969 = AXIS2_PLACEMENT_3D ( 'NONE', #27634, #35701, #1450 ) ;
#5970 = CARTESIAN_POINT ( 'NONE',  ( 19.12409105625795291, -101.5943176906707919, 5.500000000000000000 ) ) ;
#5971 = ORIENTED_EDGE ( 'NONE', *, *, #33757, .T. ) ;
#5972 = CARTESIAN_POINT ( 'NONE',  ( 0.000000000000000000, 0.000000000000000000, -1.199999999999999956 ) ) ;
#5973 = FACE_BOUND ( 'NONE', #25646, .T. ) ;
#5974 = CARTESIAN_POINT ( 'NONE',  ( -10.00000000000000000, 0.000000000000000000, 0.000000000000000000 ) ) ;
#5975 = LINE ( 'NONE', #38588, #37901 ) ;
#5976 = ORIENTED_EDGE ( 'NONE', *, *, #40959, .T. ) ;
#5977 = DIRECTION ( 'NONE',  ( 0.000000000000000000, 0.000000000000000000, 1.000000000000000000 ) ) ;
#5978 = CARTESIAN_POINT ( 'NONE',  ( 11.99999999999999822, 0.000000000000000000, 0.000000000000000000 ) ) ;
#5979 = AXIS2_PLACEMENT_3D ( 'NONE', #21891, #21169, #3282 ) ;
#5980 = EDGE_LOOP ( 'NONE', ( #38335, #35686, #23336, #34280 ) ) ;
#5981 = VERTEX_POINT ( 'NONE', #40862 ) ;
#5982 = DIRECTION ( 'NONE',  ( 0.000000000000000000, -0.000000000000000000, -1.000000000000000000 ) ) ;
#5983 = ORIENTED_EDGE ( 'NONE', *, *, #16758, .T. ) ;
#5984 = CARTESIAN_POINT ( 'NONE',  ( 0.000000000000000000, -71.21200624218825226, 40.65526001592589722 ) ) ;
#5985 = EDGE_CURVE ( 'NONE', #14256, #1784, #22737, .T. ) ;
#5986 = CIRCLE ( 'NONE', #7508, 16.00000000000000355 ) ;
#5987 = CARTESIAN_POINT ( 'NONE',  ( 10.00000000000000000, 0.000000000000000000, 0.000000000000000000 ) ) ;
#5988 = EDGE_CURVE ( 'NONE', #21754, #36710, #26661, .T. ) ;
#5989 = ORIENTED_EDGE ( 'NONE', *, *, #18980, .F. ) ;
#5990 = AXIS2_PLACEMENT_3D ( 'NONE', #41713, #26778, #23113 ) ;
#5991 = CARTESIAN_POINT ( 'NONE',  ( 11.99999999999999822, -70.53064760720297954, -26.01480285779911839 ) ) ;
#5992 = AXIS2_PLACEMENT_3D ( 'NONE', #9320, #35511, #12524 ) ;
#5993 = VERTEX_POINT ( 'NONE', #48204 ) ;
#5994 = AXIS2_PLACEMENT_3D ( 'NONE', #16409, #23502, #38937 ) ;
#5995 = VERTEX_POINT ( 'NONE', #11252 ) ;
#5996 = EDGE_CURVE ( 'NONE', #4855, #40825, #37668, .T. ) ;
#5997 = EDGE_CURVE ( 'NONE', #19709, #42613, #33144, .T. ) ;
#5998 = CIRCLE ( 'NONE', #40408, 12.49999999999999645 ) ;
#5999 = DIRECTION ( 'NONE',  ( -0.000000000000000000, 0.7431448254773945772, 0.6691306063588579045 ) ) ;
#6000 = EDGE_CURVE ( 'NONE', #28111, #14239, #14918, .T. ) ;
#6001 = CARTESIAN_POINT ( 'NONE',  ( 12.69589495141918611, -96.69089767102708777, -5.500000000000000000 ) ) ;
#6003 = ORIENTED_EDGE ( 'NONE', *, *, #20846, .F. ) ;
#6002 = CARTESIAN_POINT ( 'NONE',  ( 0.000000000000000000, 21.60688246758696707, -79.10210256391346206 ) ) ;
#6004 = VERTEX_POINT ( 'NONE', #37919 ) ;
#6005 = DIRECTION ( 'NONE',  ( -1.000000000000000000, 0.000000000000000000, 0.000000000000000000 ) ) ;
#6006 = ORIENTED_EDGE ( 'NONE', *, *, #39525, .T. ) ;
#6007 = CYLINDRICAL_SURFACE ( 'NONE', #39763, 37.49900000000000233 ) ;
#6008 = DIRECTION ( 'NONE',  ( 0.000000000000000000, 0.1564344650402312298, -0.9876883405951375483 ) ) ;
#6009 = CARTESIAN_POINT ( 'NONE',  ( 10.00000000000000000, -21.40280677340398441, 36.13751322684410638 ) ) ;
#6010 = EDGE_CURVE ( 'NONE', #14267, #6565, #40615, .T. ) ;
#6011 = VECTOR ( 'NONE', #7249, 1000.000000000000000 ) ;
#6012 = ORIENTED_EDGE ( 'NONE', *, *, #9922, .T. ) ;
#6013 = DIRECTION ( 'NONE',  ( -0.000000000000000000, -0.000000000000000000, -1.000000000000000000 ) ) ;
#6014 = EDGE_LOOP ( 'NONE', ( #45785, #28980, #21540, #44916 ) ) ;
#6015 = FACE_BOUND ( 'NONE', #26383, .T. ) ;
#6016 = CARTESIAN_POINT ( 'NONE',  ( 0.000000000000000000, 0.000000000000000000, 125.0000000000000000 ) ) ;
#6017 = CARTESIAN_POINT ( 'NONE',  ( 10.00000000000000000, -37.48860685352290290, -0.8828120875904512665 ) ) ;
#6018 = CARTESIAN_POINT ( 'NONE',  ( 10.00000000000000000, 76.66974797899852945, -11.30684508768257679 ) ) ;
#6019 = CARTESIAN_POINT ( 'NONE',  ( 6.000000000000000000, -21.60688246758530795, -79.10210256391388839 ) ) ;
#6020 = DIRECTION ( 'NONE',  ( -1.000000000000000000, 0.000000000000000000, -0.000000000000000000 ) ) ;
#6021 = DIRECTION ( 'NONE',  ( -1.000000000000000000, 0.000000000000000000, 0.000000000000000000 ) ) ;
#6022 = CARTESIAN_POINT ( 'NONE',  ( 10.00000000000000000, -21.32104025579091910, -30.84782396557241313 ) ) ;
#6023 = LINE ( 'NONE', #20941, #21247 ) ;
#6024 = DIRECTION ( 'NONE',  ( -1.000000000000000000, -0.000000000000000000, -0.000000000000000000 ) ) ;
#6025 = ORIENTED_EDGE ( 'NONE', *, *, #42098, .F. ) ;
#6026 = AXIS2_PLACEMENT_3D ( 'NONE', #29178, #29437, #43876 ) ;
#6027 = PRESENTATION_STYLE_ASSIGNMENT (( #16547 ) ) ;
#6028 = DIRECTION ( 'NONE',  ( -0.000000000000000000, 0.2079116908177543743, 0.9781476007338066880 ) ) ;
#6029 = CARTESIAN_POINT ( 'NONE',  ( 10.00000000000000000, -35.53030884539094103, 12.26510123303246935 ) ) ;
#6030 = AXIS2_PLACEMENT_3D ( 'NONE', #42499, #31495, #35140 ) ;
#6031 = CARTESIAN_POINT ( 'NONE',  ( 48.80839716909466830, -10.37454508288725208, 5.500000000000000000 ) ) ;
#6032 = ORIENTED_EDGE ( 'NONE', *, *, #27106, .T. ) ;
#6033 = CARTESIAN_POINT ( 'NONE',  ( 5.999999999999999112, -44.99326035066101781, 68.55367621811126355 ) ) ;
#6034 = LINE ( 'NONE', #24856, #1881 ) ;
#6035 = ORIENTED_EDGE ( 'NONE', *, *, #36120, .F. ) ;
#6036 = EDGE_CURVE ( 'NONE', #33795, #34978, #29837, .T. ) ;
#6037 = LINE ( 'NONE', #21179, #37896 ) ;
#6038 = ADVANCED_FACE ( 'NONE', ( #22506 ), #22982, .T. ) ;
#6039 = ORIENTED_EDGE ( 'NONE', *, *, #25522, .T. ) ;
#6040 = CYLINDRICAL_SURFACE ( 'NONE', #36900, 31.99999999999999289 ) ;
#6041 = EDGE_CURVE ( 'NONE', #32445, #37684, #2659, .T. ) ;
#6042 = ORIENTED_EDGE ( 'NONE', *, *, #18779, .F. ) ;
#6043 = CIRCLE ( 'NONE', #2878, 11.59999999999999787 ) ;
#6044 = VERTEX_POINT ( 'NONE', #41118 ) ;
#6045 = VECTOR ( 'NONE', #4496, 1000.000000000000000 ) ;
#6046 = EDGE_CURVE ( 'NONE', #32651, #10384, #8132, .T. ) ;
#6047 = EDGE_LOOP ( 'NONE', ( #23411, #40956, #17910, #45231 ) ) ;
#6048 = EDGE_CURVE ( 'NONE', #21073, #19357, #19061, .T. ) ;
#6049 = CIRCLE ( 'NONE', #44324, 16.00000000000000000 ) ;
#6050 = DIRECTION ( 'NONE',  ( -0.000000000000000000, 0.8090169943749504489, -0.5877852522924689183 ) ) ;
#6051 = VERTEX_POINT ( 'NONE', #18811 ) ;
#6052 = ORIENTED_EDGE ( 'NONE', *, *, #35081, .T. ) ;
#6053 = VECTOR ( 'NONE', #3481, 1000.000000000000000 ) ;
#6054 = DIRECTION ( 'NONE',  ( -1.000000000000000000, 0.000000000000000000, 0.000000000000000000 ) ) ;
#6056 = VERTEX_POINT ( 'NONE', #7080 ) ;
#6055 = CARTESIAN_POINT ( 'NONE',  ( 0.000000000000000000, 0.000000000000000000, 0.000000000000000000 ) ) ;
#6057 = ORIENTED_EDGE ( 'NONE', *, *, #6163, .T. ) ;
#6058 = ORIENTED_EDGE ( 'NONE', *, *, #42374, .T. ) ;
#6059 = ORIENTED_EDGE ( 'NONE', *, *, #6753, .T. ) ;
#6060 = CARTESIAN_POINT ( 'NONE',  ( 0.000000000000000000, -33.71516098798685590, -74.74816331893465815 ) ) ;
#6061 = CARTESIAN_POINT ( 'NONE',  ( 15.00000000000000000, 16.83928648764922542, -16.46020748918050458 ) ) ;
#6062 = CIRCLE ( 'NONE', #20096, 31.99999999999999289 ) ;
#6063 = EDGE_CURVE ( 'NONE', #2200, #37092, #5802, .T. ) ;
#6064 = CARTESIAN_POINT ( 'NONE',  ( 0.000000000000000000, 77.49459641780886443, 0.8261519478433866359 ) ) ;
#6065 = ORIENTED_EDGE ( 'NONE', *, *, #1721, .F. ) ;
#6066 = ORIENTED_EDGE ( 'NONE', *, *, #42432, .F. ) ;
#6067 = ORIENTED_EDGE ( 'NONE', *, *, #31711, .T. ) ;
#6068 = DIRECTION ( 'NONE',  ( 1.000000000000000000, -0.000000000000000000, 0.000000000000000000 ) ) ;
#6069 = ORIENTED_EDGE ( 'NONE', *, *, #15539, .F. ) ;
#6070 = DIRECTION ( 'NONE',  ( 0.000000000000000000, 0.000000000000000000, 1.000000000000000000 ) ) ;
#6071 = LINE ( 'NONE', #47169, #21775 ) ;
#6072 = CARTESIAN_POINT ( 'NONE',  ( -3.000000000000000000, -23.29833615347104825, -3.418703333116803744 ) ) ;
#6073 = DIRECTION ( 'NONE',  ( 1.000000000000000000, 0.000000000000000000, -0.000000000000000000 ) ) ;
#6074 = CYLINDRICAL_SURFACE ( 'NONE', #33855, 16.00000000000000000 ) ;
#6075 = ADVANCED_FACE ( 'NONE', ( #3399 ), #44293, .T. ) ;
#6076 = DIRECTION ( 'NONE',  ( -1.000000000000000000, -0.000000000000000000, 0.000000000000000000 ) ) ;
#6077 = ADVANCED_FACE ( 'NONE', ( #18587 ), #33508, .F. ) ;
#6078 = DIRECTION ( 'NONE',  ( 0.000000000000000000, 0.000000000000000000, 1.000000000000000000 ) ) ;
#6079 = VECTOR ( 'NONE', #31666, 1000.000000000000000 ) ;
#6080 = EDGE_LOOP ( 'NONE', ( #10535, #30872, #4258, #29737 ) ) ;
#6081 = CARTESIAN_POINT ( 'NONE',  ( 10.00000000000000000, -39.47590169984896136, 71.87247863392398983 ) ) ;
#6082 = ORIENTED_EDGE ( 'NONE', *, *, #24203, .T. ) ;
#6083 = CARTESIAN_POINT ( 'NONE',  ( 10.00000000000000000, 65.58780272294129077, -36.73666225445822420 ) ) ;
#6084 = DIRECTION ( 'NONE',  ( 0.000000000000000000, 0.000000000000000000, 1.000000000000000000 ) ) ;
#6085 = CARTESIAN_POINT ( 'NONE',  ( 0.000000000000000000, 5.835314593368772229, -22.81335362449846826 ) ) ;
#6086 = ORIENTED_EDGE ( 'NONE', *, *, #41245, .T. ) ;
#6087 = CYLINDRICAL_SURFACE ( 'NONE', #44772, 77.49899999999999523 ) ;
#6088 = LINE ( 'NONE', #21000, #15829 ) ;
#6089 = DIRECTION ( 'NONE',  ( 0.000000000000000000, 0.000000000000000000, 1.000000000000000000 ) ) ;
#6090 = ADVANCED_FACE ( 'NONE', ( #11003 ), #25920, .T. ) ;
#6091 = VERTEX_POINT ( 'NONE', #12228 ) ;
#6092 = CIRCLE ( 'NONE', #18547, 82.00000000000000000 ) ;
#6093 = DIRECTION ( 'NONE',  ( -0.000000000000000000, -1.000000000000000000, -0.000000000000000000 ) ) ;
#6094 = DIRECTION ( 'NONE',  ( -1.000000000000000000, 0.000000000000000000, 0.000000000000000000 ) ) ;
#6095 = FACE_OUTER_BOUND ( 'NONE', #36393, .T. ) ;
#6096 = EDGE_CURVE ( 'NONE', #29406, #45717, #38159, .T. ) ;
#6097 = DIRECTION ( 'NONE',  ( 0.000000000000000000, 0.000000000000000000, 1.000000000000000000 ) ) ;
#6098 = EDGE_CURVE ( 'NONE', #38630, #13774, #30044, .T. ) ;
#6099 = EDGE_LOOP ( 'NONE', ( #14607, #1835, #34984, #42576 ) ) ;
#6100 = ORIENTED_EDGE ( 'NONE', *, *, #35931, .T. ) ;
#6101 = CIRCLE ( 'NONE', #20940, 31.99999999999998579 ) ;
#6102 = EDGE_CURVE ( 'NONE', #40367, #13990, #8297, .T. ) ;
#6103 = ORIENTED_EDGE ( 'NONE', *, *, #3986, .T. ) ;
#6104 = CYLINDRICAL_SURFACE ( 'NONE', #15535, 42.00000000000000000 ) ;
#6105 = DIRECTION ( 'NONE',  ( 0.000000000000000000, 0.000000000000000000, 1.000000000000000000 ) ) ;
#6106 = VERTEX_POINT ( 'NONE', #20271 ) ;
#6107 = ORIENTED_EDGE ( 'NONE', *, *, #41198, .F. ) ;
#6108 = AXIS2_PLACEMENT_3D ( 'NONE', #37603, #29772, #14855 ) ;
#6109 = DIRECTION ( 'NONE',  ( 0.000000000000000000, -0.9238795325112906243, 0.3826834323650804004 ) ) ;
#6110 = ORIENTED_EDGE ( 'NONE', *, *, #41387, .T. ) ;
#6111 = ORIENTED_EDGE ( 'NONE', *, *, #32777, .F. ) ;
#6112 = ORIENTED_EDGE ( 'NONE', *, *, #10790, .F. ) ;
#6113 = CARTESIAN_POINT ( 'NONE',  ( 0.000000000000000000, 8.830959090342393125, 74.65491531819122883 ) ) ;
#6114 = ORIENTED_EDGE ( 'NONE', *, *, #36049, .T. ) ;
#6115 = CYLINDRICAL_SURFACE ( 'NONE', #40356, 42.00000000000000000 ) ;
#6116 = EDGE_LOOP ( 'NONE', ( #10696, #27103, #45299, #8951 ) ) ;
#6117 = DIRECTION ( 'NONE',  ( -1.000000000000000000, 0.000000000000000000, 0.000000000000000000 ) ) ;
#6118 = DIRECTION ( 'NONE',  ( 0.000000000000000000, 0.000000000000000000, -1.000000000000000000 ) ) ;
#6119 = DIRECTION ( 'NONE',  ( 0.000000000000000000, 0.000000000000000000, -1.000000000000000000 ) ) ;
#6120 = VERTEX_POINT ( 'NONE', #5119 ) ;
#6121 = CARTESIAN_POINT ( 'NONE',  ( -42.50000000000000000, 0.000000000000000000, 0.000000000000000000 ) ) ;
#6122 = ORIENTED_EDGE ( 'NONE', *, *, #30960, .F. ) ;
#6123 = AXIS2_PLACEMENT_3D ( 'NONE', #29297, #10702, #33445 ) ;
#6124 = DIRECTION ( 'NONE',  ( -1.000000000000000000, -0.000000000000000000, -0.000000000000000000 ) ) ;
#6125 = CARTESIAN_POINT ( 'NONE',  ( 30.50000000000000000, -120.0000000000000000, 2.500000000000000000 ) ) ;
#6126 = ORIENTED_EDGE ( 'NONE', *, *, #37923, .T. ) ;
#6127 = VERTEX_POINT ( 'NONE', #4402 ) ;
#6128 = FACE_OUTER_BOUND ( 'NONE', #45641, .T. ) ;
#6129 = CARTESIAN_POINT ( 'NONE',  ( 11.99999999999999822, 39.78640506895698792, -66.50666863321958999 ) ) ;
#6130 = ORIENTED_EDGE ( 'NONE', *, *, #41494, .T. ) ;
#6131 = EDGE_CURVE ( 'NONE', #20243, #30855, #18291, .T. ) ;
#6132 = DIRECTION ( 'NONE',  ( -1.000000000000000000, 0.000000000000000000, 0.000000000000000000 ) ) ;
#6133 = FACE_OUTER_BOUND ( 'NONE', #37331, .T. ) ;
#6134 = CARTESIAN_POINT ( 'NONE',  ( -10.00000000000000000, 0.000000000000000000, 0.000000000000000000 ) ) ;
#6135 = CYLINDRICAL_SURFACE ( 'NONE', #14828, 42.00000000000000000 ) ;
#6136 = DIRECTION ( 'NONE',  ( -0.1045284632676436315, -0.9945218953682742891, 0.000000000000000000 ) ) ;
#6137 = DIRECTION ( 'NONE',  ( 0.7585478161175706058, 0.6516173805718080692, -0.000000000000000000 ) ) ;
#6138 = FACE_OUTER_BOUND ( 'NONE', #42443, .T. ) ;
#6139 = VECTOR ( 'NONE', #23208, 1000.000000000000000 ) ;
#6140 = FACE_OUTER_BOUND ( 'NONE', #38172, .T. ) ;
#6141 = CARTESIAN_POINT ( 'NONE',  ( -10.00000000000000000, 0.000000000000000000, 0.000000000000000000 ) ) ;
#6142 = SURFACE_STYLE_USAGE ( .BOTH. , #32568 ) ;
#6143 = EDGE_CURVE ( 'NONE', #34627, #31027, #43321, .T. ) ;
#6145 = CIRCLE ( 'NONE', #18641, 77.49899999999999523 ) ;
#6144 = DIRECTION ( 'NONE',  ( 0.000000000000000000, 0.8910065241883690090, -0.4539904997395446395 ) ) ;
#6146 = DIRECTION ( 'NONE',  ( 0.000000000000000000, 0.000000000000000000, 1.000000000000000000 ) ) ;
#6147 = EDGE_CURVE ( 'NONE', #29882, #41810, #15637, .T. ) ;
#6148 = VERTEX_POINT ( 'NONE', #4622 ) ;
#6149 = EDGE_CURVE ( 'NONE', #18061, #5554, #25338, .T. ) ;
#6150 = ADVANCED_FACE ( 'NONE', ( #42076 ), #27152, .T. ) ;
#6151 = ORIENTED_EDGE ( 'NONE', *, *, #1083, .F. ) ;
#6152 = EDGE_CURVE ( 'NONE', #708, #42399, #38897, .T. ) ;
#6153 = CARTESIAN_POINT ( 'NONE',  ( 10.00000000000000000, 35.92658777277525672, -10.74501242461245809 ) ) ;
#6154 = ADVANCED_FACE ( 'NONE', ( #19524 ), #9025, .T. ) ;
#6155 = CONTEXT_DEPENDENT_SHAPE_REPRESENTATION ( #33231, #10902 ) ;
#6156 = EDGE_CURVE ( 'NONE', #47410, #43520, #38399, .T. ) ;
#6157 = LINE ( 'NONE', #13029, #35456 ) ;
#6158 = EDGE_LOOP ( 'NONE', ( #13545, #11494, #1073, #17586 ) ) ;
#6159 = AXIS2_PLACEMENT_3D ( 'NONE', #38469, #11571, #34066 ) ;
#6160 = CARTESIAN_POINT ( 'NONE',  ( 0.000000000000000000, 24.81905959214274660, -9.408202855044498492 ) ) ;
#6161 = ORIENTED_EDGE ( 'NONE', *, *, #33289, .F. ) ;
#6162 = DIRECTION ( 'NONE',  ( -1.000000000000000000, 0.000000000000000000, 0.000000000000000000 ) ) ;
#6163 = EDGE_CURVE ( 'NONE', #30318, #14976, #22216, .T. ) ;
#6164 = ORIENTED_EDGE ( 'NONE', *, *, #23312, .T. ) ;
#6165 = FILL_AREA_STYLE ('',( #44326 ) ) ;
#6166 = ORIENTED_EDGE ( 'NONE', *, *, #19290, .T. ) ;
#6167 = DIRECTION ( 'NONE',  ( 1.000000000000000000, 0.000000000000000000, 0.000000000000000000 ) ) ;
#6168 = ORIENTED_EDGE ( 'NONE', *, *, #15923, .F. ) ;
#6169 = AXIS2_PLACEMENT_3D ( 'NONE', #40637, #3430, #16324 ) ;
#6170 = LINE ( 'NONE', #24771, #26612 ) ;
#6171 = ORIENTED_EDGE ( 'NONE', *, *, #14198, .T. ) ;
#6172 = DIRECTION ( 'NONE',  ( -1.000000000000000000, 0.000000000000000000, 0.000000000000000000 ) ) ;
#6173 = ORIENTED_EDGE ( 'NONE', *, *, #10395, .F. ) ;
#6174 = CIRCLE ( 'NONE', #43694, 16.00000000000000000 ) ;
#6175 = AXIS2_PLACEMENT_3D ( 'NONE', #26837, #7521, #876 ) ;
#6176 = AXIS2_PLACEMENT_3D ( 'NONE', #42050, #15389, #12199 ) ;
#6177 = DIRECTION ( 'NONE',  ( -0.9827303690289279636, -0.1850432970638682117, 0.000000000000000000 ) ) ;
#6178 = CARTESIAN_POINT ( 'NONE',  ( 4.999999999999999112, -9.188173127307592836, 40.98264845739746676 ) ) ;
#6179 = CARTESIAN_POINT ( 'NONE',  ( 5.000000000000000000, 35.47612816024556537, -22.48208911017461631 ) ) ;
#6180 = DIRECTION ( 'NONE',  ( 0.000000000000000000, -0.8910065241883723397, 0.4539904997395382003 ) ) ;
#6181 = CARTESIAN_POINT ( 'NONE',  ( 20.85212586905262100, -130.9402397935870965, 5.500000000000000000 ) ) ;
#6182 = VERTEX_POINT ( 'NONE', #5356 ) ;
#6183 = CARTESIAN_POINT ( 'NONE',  ( 0.000000000000000000, -39.78640506895652607, 66.50666863321986000 ) ) ;
#6184 = ORIENTED_EDGE ( 'NONE', *, *, #25293, .T. ) ;
#6185 = VERTEX_POINT ( 'NONE', #16603 ) ;
#6186 = CARTESIAN_POINT ( 'NONE',  ( 0.000000000000000000, 6.903761155838878061, -77.19088730480517313 ) ) ;
#6187 = VERTEX_POINT ( 'NONE', #1682 ) ;
#6188 = EDGE_CURVE ( 'NONE', #41290, #25709, #31555, .T. ) ;
#6189 = VECTOR ( 'NONE', #5600, 1000.000000000000227 ) ;
#6190 = CARTESIAN_POINT ( 'NONE',  ( 10.00000000000000000, -14.67089635893658794, -73.72996012237454977 ) ) ;
#6191 = DIRECTION ( 'NONE',  ( 0.000000000000000000, -0.5000000000000046629, 0.8660254037844359321 ) ) ;
#6192 = CARTESIAN_POINT ( 'NONE',  ( 10.00000000000000000, 35.95386929396241271, 10.96151621346552751 ) ) ;
#6193 = VERTEX_POINT ( 'NONE', #45489 ) ;
#6194 = CARTESIAN_POINT ( 'NONE',  ( 11.41210121379328335, -99.40233154247455616, 5.500000000000000000 ) ) ;
#6195 = PRODUCT ( 'Shift Fork Lever Arm', 'Shift Fork Lever Arm', '', ( #34306 ) ) ;
#6196 = EDGE_CURVE ( 'NONE', #47392, #34754, #28477, .T. ) ;
#6197 = DIRECTION ( 'NONE',  ( 0.000000000000000000, 0.1564344650402312020, -0.9876883405951376593 ) ) ;
#6198 = CARTESIAN_POINT ( 'NONE',  ( 10.00000000000000000, 77.19088730480524418, 6.903761155838049390 ) ) ;
#6199 = PRESENTATION_LAYER_ASSIGNMENT (  '', '', ( #42921 ) ) ;
#6200 = CARTESIAN_POINT ( 'NONE',  ( 0.000000000000000000, 74.65491531819118620, -8.830959090342659579 ) ) ;
#6201 = DIRECTION ( 'NONE',  ( 0.000000000000000000, 0.000000000000000000, 1.000000000000000000 ) ) ;
#6202 = VERTEX_POINT ( 'NONE', #26906 ) ;
#6203 = CARTESIAN_POINT ( 'NONE',  ( 0.000000000000000000, -74.65491531819111515, -8.830959090343204920 ) ) ;
#6204 = CARTESIAN_POINT ( 'NONE',  ( 10.00000000000000000, -27.05870788708250885, 26.08949754953014022 ) ) ;
#6205 = CARTESIAN_POINT ( 'NONE',  ( 32.50000000000000000, -120.0000000000000000, 2.500000000000000000 ) ) ;
#6206 = CARTESIAN_POINT ( 'NONE',  ( 10.00000000000000000, -63.97538442413389248, -51.29473840253292138 ) ) ;
#6207 = CARTESIAN_POINT ( 'NONE',  ( 0.000000000000000000, 21.32104025579114648, 30.84782396557224970 ) ) ;
#6208 = DIRECTION ( 'NONE',  ( -1.000000000000000000, 0.000000000000000000, 0.000000000000000000 ) ) ;
#6209 = EDGE_CURVE ( 'NONE', #13885, #5905, #19857, .T. ) ;
#6210 = ORIENTED_EDGE ( 'NONE', *, *, #19225, .T. ) ;
#6211 = EDGE_CURVE ( 'NONE', #25900, #22480, #34714, .T. ) ;
#6212 = ORIENTED_EDGE ( 'NONE', *, *, #37907, .T. ) ;
#6213 = VECTOR ( 'NONE', #12285, 1000.000000000000000 ) ;
#6214 = DIRECTION ( 'NONE',  ( -1.000000000000000000, 0.000000000000000000, 0.000000000000000000 ) ) ;
#6215 = AXIS2_PLACEMENT_3D ( 'NONE', #40111, #6575, #41807 ) ;
#6216 = ORIENTED_EDGE ( 'NONE', *, *, #40316, .F. ) ;
#6217 = CARTESIAN_POINT ( 'NONE',  ( 10.00000000000000000, -33.79645857604525361, 16.45098606841114730 ) ) ;
#6218 = VECTOR ( 'NONE', #37393, 1000.000000000000000 ) ;
#6219 = DIRECTION ( 'NONE',  ( 0.000000000000000000, 0.000000000000000000, -1.000000000000000000 ) ) ;
#6220 = ORIENTED_EDGE ( 'NONE', *, *, #23365, .T. ) ;
#6221 = EDGE_CURVE ( 'NONE', #23379, #7626, #44886, .T. ) ;
#6222 = CIRCLE ( 'NONE', #19495, 16.00000000000000355 ) ;
#6223 = DIRECTION ( 'NONE',  ( 0.000000000000000000, 0.000000000000000000, 1.000000000000000000 ) ) ;
#6224 = ORIENTED_EDGE ( 'NONE', *, *, #22597, .T. ) ;
#6225 = VERTEX_POINT ( 'NONE', #39124 ) ;
#6226 = ORIENTED_EDGE ( 'NONE', *, *, #14825, .T. ) ;
#6227 = DIRECTION ( 'NONE',  ( -1.000000000000000000, -0.000000000000000000, 0.000000000000000000 ) ) ;
#6228 = ORIENTED_EDGE ( 'NONE', *, *, #3364, .F. ) ;
#6229 = DIRECTION ( 'NONE',  ( 0.000000000000000000, 0.3090169943749410120, 0.9510565162951557516 ) ) ;
#6230 = DIRECTION ( 'NONE',  ( -1.000000000000000000, 0.000000000000000000, 0.000000000000000000 ) ) ;
#6231 = ORIENTED_EDGE ( 'NONE', *, *, #27827, .F. ) ;
#6232 = LINE ( 'NONE', #46630, #42284 ) ;
#6233 = EDGE_LOOP ( 'NONE', ( #31527, #32537, #36133, #16754 ) ) ;
#6234 = EDGE_LOOP ( 'NONE', ( #33759, #39607, #4754, #4705 ) ) ;
#6235 = CARTESIAN_POINT ( 'NONE',  ( -3.000000000000000000, -19.89357724625003598, 12.59942793731059574 ) ) ;
#6236 = DIRECTION ( 'NONE',  ( -1.000000000000000000, 0.000000000000000000, -0.000000000000000000 ) ) ;
#6237 = DIRECTION ( 'NONE',  ( 0.000000000000000000, -0.4539904997395350361, -0.8910065241883738940 ) ) ;
#6238 = VECTOR ( 'NONE', #12518, 999.9999999999998863 ) ;
#6239 = EDGE_CURVE ( 'NONE', #6864, #27731, #10475, .T. ) ;
#6240 = ORIENTED_EDGE ( 'NONE', *, *, #48178, .F. ) ;
#6241 = VECTOR ( 'NONE', #22418, 1000.000000000000000 ) ;
#6242 = FACE_OUTER_BOUND ( 'NONE', #609, .T. ) ;
#6243 = ORIENTED_EDGE ( 'NONE', *, *, #26144, .F. ) ;
#6244 = DIRECTION ( 'NONE',  ( 1.000000000000000000, 0.000000000000000000, -0.000000000000000000 ) ) ;
#6246 = EDGE_CURVE ( 'NONE', #30662, #40104, #24424, .T. ) ;
#6245 = AXIS2_PLACEMENT_3D ( 'NONE', #38977, #35535, #16694 ) ;
#6247 = LINE ( 'NONE', #5766, #8190 ) ;
#6248 = DIRECTION ( 'NONE',  ( 0.000000000000000000, 0.000000000000000000, 1.000000000000000000 ) ) ;
#6249 = LINE ( 'NONE', #17487, #28937 ) ;
#6250 = LINE ( 'NONE', #39289, #29214 ) ;
#6251 = EDGE_CURVE ( 'NONE', #3694, #18975, #26158, .T. ) ;
#6252 = CARTESIAN_POINT ( 'NONE',  ( 0.000000000000000000, 78.73519480814955784, 22.90783923731656557 ) ) ;
#6253 = CIRCLE ( 'NONE', #26574, 31.99999999999999289 ) ;
#6254 = DIRECTION ( 'NONE',  ( 0.6575728627325955200, -0.7533909544171997208, 0.000000000000000000 ) ) ;
#6255 = FACE_OUTER_BOUND ( 'NONE', #2970, .T. ) ;
#6256 = DIRECTION ( 'NONE',  ( -0.000000000000000000, -0.000000000000000000, -1.000000000000000000 ) ) ;
#6257 = DIRECTION ( 'NONE',  ( 1.000000000000000000, 0.000000000000000000, 0.000000000000000000 ) ) ;
#6258 = VERTEX_POINT ( 'NONE', #21480 ) ;
#6259 = CIRCLE ( 'NONE', #15645, 31.99999999999998579 ) ;
#6260 = DIRECTION ( 'NONE',  ( 0.000000000000000000, 0.000000000000000000, 1.000000000000000000 ) ) ;
#6261 = PLANE ( 'NONE',  #37673 ) ;
#6262 = DIRECTION ( 'NONE',  ( 0.000000000000000000, 0.000000000000000000, 1.000000000000000000 ) ) ;
#6263 = ADVANCED_FACE ( 'NONE', ( #16857 ), #2615, .T. ) ;
#6264 = EDGE_CURVE ( 'NONE', #9557, #18553, #13655, .T. ) ;
#6265 = DIRECTION ( 'NONE',  ( -1.000000000000000000, -0.000000000000000000, -0.000000000000000000 ) ) ;
#6266 = DIRECTION ( 'NONE',  ( 1.000000000000000000, -0.000000000000000000, -0.000000000000000000 ) ) ;
#6267 = DIRECTION ( 'NONE',  ( 0.000000000000000000, 0.9135454576426060846, -0.4067366430757888285 ) ) ;
#6268 = EDGE_CURVE ( 'NONE', #21081, #39544, #12096, .T. ) ;
#6269 = ORIENTED_EDGE ( 'NONE', *, *, #32753, .F. ) ;
#6270 = DIRECTION ( 'NONE',  ( -1.000000000000000000, 0.000000000000000000, 0.000000000000000000 ) ) ;
#6271 = FACE_OUTER_BOUND ( 'NONE', #6080, .T. ) ;
#6272 = ORIENTED_EDGE ( 'NONE', *, *, #24466, .F. ) ;
#6273 = VERTEX_POINT ( 'NONE', #20764 ) ;
#6274 = ADVANCED_FACE ( 'NONE', ( #46723 ), #47186, .T. ) ;
#6275 = AXIS2_PLACEMENT_3D ( 'NONE', #27792, #42717, #6005 ) ;
#6276 = EDGE_LOOP ( 'NONE', ( #38206, #21022, #47282, #39099 ) ) ;
#6277 = CIRCLE ( 'NONE', #42998, 31.99999999999998579 ) ;
#6278 = VERTEX_POINT ( 'NONE', #43523 ) ;
#6279 = VECTOR ( 'NONE', #24449, 999.9999999999998863 ) ;
#6280 = CARTESIAN_POINT ( 'NONE',  ( 11.99999999999999822, -41.19522573413780009, 65.64334221924896440 ) ) ;
#6281 = EDGE_LOOP ( 'NONE', ( #10052, #25733, #43902, #30184 ) ) ;
#6282 =( GEOMETRIC_REPRESENTATION_CONTEXT ( 3 ) GLOBAL_UNCERTAINTY_ASSIGNED_CONTEXT ( ( #37936 ) ) GLOBAL_UNIT_ASSIGNED_CONTEXT ( ( #9344, #42651, #9110 ) ) REPRESENTATION_CONTEXT ( 'NONE', 'WORKASPACE' ) );
#6283 = AXIS2_PLACEMENT_3D ( 'NONE', #12624, #27554, #32895 ) ;
#6284 = EDGE_LOOP ( 'NONE', ( #36652, #41436, #33837, #12563 ) ) ;
#6285 = CIRCLE ( 'NONE', #20347, 37.49900000000001654 ) ;
#6286 = CARTESIAN_POINT ( 'NONE',  ( 0.000000000000000000, -6.555932627142676772, 37.01155633439056203 ) ) ;
#6288 = VERTEX_POINT ( 'NONE', #29059 ) ;
#6287 = CARTESIAN_POINT ( 'NONE',  ( 11.99999999999999822, -50.95692526931372157, 58.39081064771733054 ) ) ;
#6289 = VERTEX_POINT ( 'NONE', #35444 ) ;
#6290 = VERTEX_POINT ( 'NONE', #40085 ) ;
#6291 = VERTEX_POINT ( 'NONE', #13662 ) ;
#6292 = DIRECTION ( 'NONE',  ( -1.000000000000000000, -0.000000000000000000, 0.000000000000000000 ) ) ;
#6293 = CARTESIAN_POINT ( 'NONE',  ( -12.50000000000000000, -132.5000000000000000, 40.00000000000000000 ) ) ;
#6294 = DIRECTION ( 'NONE',  ( -1.000000000000000000, 0.000000000000000000, 0.000000000000000000 ) ) ;
#6295 = ORIENTED_EDGE ( 'NONE', *, *, #33489, .T. ) ;
#6296 = ORIENTED_EDGE ( 'NONE', *, *, #22115, .T. ) ;
#6297 = DIRECTION ( 'NONE',  ( 0.9848077530122080203, -0.1736481776669309696, 0.000000000000000000 ) ) ;
#6298 = CARTESIAN_POINT ( 'NONE',  ( 10.00000000000000000, -37.22597642581153821, -5.202137450156795850 ) ) ;
#6299 = EDGE_CURVE ( 'NONE', #28619, #21334, #9978, .T. ) ;
#6300 = DIRECTION ( 'NONE',  ( -1.000000000000000000, 0.000000000000000000, 0.000000000000000000 ) ) ;
#6301 = FACE_OUTER_BOUND ( 'NONE', #16047, .T. ) ;
#6302 = DIRECTION ( 'NONE',  ( -1.000000000000000000, 0.000000000000000000, -0.000000000000000000 ) ) ;
#6303 = EDGE_CURVE ( 'NONE', #2489, #2128, #13178, .T. ) ;
#6304 = EDGE_CURVE ( 'NONE', #1546, #7292, #43362, .T. ) ;
#6305 = CARTESIAN_POINT ( 'NONE',  ( 10.00000000000000000, -35.95386929396248377, -10.96151621346525751 ) ) ;
#6306 = EDGE_CURVE ( 'NONE', #24194, #44863, #22247, .T. ) ;
#6307 = VECTOR ( 'NONE', #33398, 1000.000000000000227 ) ;
#6308 = CARTESIAN_POINT ( 'NONE',  ( 0.000000000000000000, 0.000000000000000000, 0.000000000000000000 ) ) ;
#6309 = ORIENTED_EDGE ( 'NONE', *, *, #4204, .F. ) ;
#6310 = VECTOR ( 'NONE', #12791, 1000.000000000000000 ) ;
#6311 = EDGE_CURVE ( 'NONE', #11482, #7668, #46951, .T. ) ;
#6312 = FACE_OUTER_BOUND ( 'NONE', #45710, .T. ) ;
#6313 = VERTEX_POINT ( 'NONE', #10216 ) ;
#6314 = AXIS2_PLACEMENT_3D ( 'NONE', #17423, #20880, #32381 ) ;
#6315 = CIRCLE ( 'NONE', #35196, 42.00000000000000000 ) ;
#6316 = CARTESIAN_POINT ( 'NONE',  ( 50.00005079999999680, 12.24744871391589207, -2.499999999999994671 ) ) ;
#6317 = CYLINDRICAL_SURFACE ( 'NONE', #27091, 42.00000000000000000 ) ;
#6318 = DIRECTION ( 'NONE',  ( 0.000000000000000000, -0.8526401643540860720, -0.5224985647159589019 ) ) ;
#6319 = CARTESIAN_POINT ( 'NONE',  ( 12.00000000000000000, 16.61724383029361718, -20.69703378468927113 ) ) ;
#6320 = AXIS2_PLACEMENT_3D ( 'NONE', #23506, #8342, #42119 ) ;
#6321 = ADVANCED_FACE ( 'NONE', ( #36408, #32033 ), #28337, .F. ) ;
#6322 = VECTOR ( 'NONE', #45868, 1000.000000000000000 ) ;
#6323 = DIRECTION ( 'NONE',  ( 1.000000000000000000, -0.000000000000000000, 0.000000000000000000 ) ) ;
#6324 = CARTESIAN_POINT ( 'NONE',  ( -3.000000000000000000, -1.278221433540502217, 26.51162292216071847 ) ) ;
#6325 = AXIS2_PLACEMENT_3D ( 'NONE', #8758, #16132, #31064 ) ;
#6326 = LINE ( 'NONE', #2624, #12060 ) ;
#6327 = FACE_OUTER_BOUND ( 'NONE', #18303, .T. ) ;
#6328 = EDGE_CURVE ( 'NONE', #28147, #13467, #26935, .T. ) ;
#6329 = CARTESIAN_POINT ( 'NONE',  ( 0.000000000000000000, 0.000000000000000000, -125.0000000000000000 ) ) ;
#6330 = ORIENTED_EDGE ( 'NONE', *, *, #43881, .F. ) ;
#6331 = ORIENTED_EDGE ( 'NONE', *, *, #8245, .F. ) ;
#6332 = ORIENTED_EDGE ( 'NONE', *, *, #14991, .T. ) ;
#6333 = EDGE_CURVE ( 'NONE', #40761, #32236, #42588, .T. ) ;
#6334 = ORIENTED_EDGE ( 'NONE', *, *, #44137, .T. ) ;
#6335 = DIRECTION ( 'NONE',  ( 0.000000000000000000, -0.9135454576426010886, 0.4067366430757998752 ) ) ;
#6336 = CARTESIAN_POINT ( 'NONE',  ( 10.00000000000000178, 0.000000000000000000, 0.000000000000000000 ) ) ;
#6337 = ORIENTED_EDGE ( 'NONE', *, *, #6587, .F. ) ;
#6338 = AXIS2_PLACEMENT_3D ( 'NONE', #15946, #31371, #24018 ) ;
#6339 = EDGE_CURVE ( 'NONE', #33751, #3180, #14137, .T. ) ;
#6340 = CIRCLE ( 'NONE', #46972, 12.49999999999999645 ) ;
#6341 = LINE ( 'NONE', #29082, #35887 ) ;
#6342 = CIRCLE ( 'NONE', #14163, 31.99999999999998579 ) ;
#6343 = VECTOR ( 'NONE', #43779, 1000.000000000000000 ) ;
#6344 = ORIENTED_EDGE ( 'NONE', *, *, #34800, .T. ) ;
#6345 = ORIENTED_EDGE ( 'NONE', *, *, #32887, .F. ) ;
#6346 = VERTEX_POINT ( 'NONE', #22204 ) ;
#6347 = VECTOR ( 'NONE', #47236, 1000.000000000000000 ) ;
#6348 = AXIS2_PLACEMENT_3D ( 'NONE', #44049, #28395, #21046 ) ;
#6349 = CARTESIAN_POINT ( 'NONE',  ( -10.00000000000000000, 0.000000000000000000, 0.000000000000000000 ) ) ;
#6350 = AXIS2_PLACEMENT_3D ( 'NONE', #25849, #36634, #25132 ) ;
#6351 = ORIENTED_EDGE ( 'NONE', *, *, #19007, .T. ) ;
#6352 = DIRECTION ( 'NONE',  ( -1.000000000000000000, 0.000000000000000000, -0.000000000000000000 ) ) ;
#6353 = ORIENTED_EDGE ( 'NONE', *, *, #45997, .T. ) ;
#6354 = EDGE_CURVE ( 'NONE', #28804, #23663, #4300, .T. ) ;
#6355 = CARTESIAN_POINT ( 'NONE',  ( 15.00000000000000000, -18.13022148937242761, 15.02647892043569122 ) ) ;
#6356 = CARTESIAN_POINT ( 'NONE',  ( -10.00000000000000000, 0.000000000000000000, 0.000000000000000000 ) ) ;
#6357 = CARTESIAN_POINT ( 'NONE',  ( 5.000000000000000000, -51.29473840253177741, -63.97538442413482329 ) ) ;
#6358 = ORIENTED_EDGE ( 'NONE', *, *, #37322, .F. ) ;
#6359 = EDGE_CURVE ( 'NONE', #27340, #24200, #32419, .T. ) ;
#6360 = CARTESIAN_POINT ( 'NONE',  ( -34.02017708624680381, -130.1428571428571388, 2.500000000000000000 ) ) ;
#6361 = VERTEX_POINT ( 'NONE', #21718 ) ;
#6362 = EDGE_LOOP ( 'NONE', ( #16592, #33775, #7676, #27983 ) ) ;
#6363 = CARTESIAN_POINT ( 'NONE',  ( 0.000000000000000000, -24.73286445877654671, -73.44644590900084324 ) ) ;
#6364 = CARTESIAN_POINT ( 'NONE',  ( 12.00000000000000355, 0.000000000000000000, 0.000000000000000000 ) ) ;
#6365 = VERTEX_POINT ( 'NONE', #33693 ) ;
#6366 = ORIENTED_EDGE ( 'NONE', *, *, #9945, .F. ) ;
#6367 = EDGE_CURVE ( 'NONE', #26225, #24099, #44920, .T. ) ;
#6368 = CARTESIAN_POINT ( 'NONE',  ( 10.00000000000000000, -37.48860685352290290, -0.8828120875904512665 ) ) ;
#6369 = DIRECTION ( 'NONE',  ( -1.000000000000000000, 0.000000000000000000, -0.000000000000000000 ) ) ;
#6370 = VERTEX_POINT ( 'NONE', #3101 ) ;
#6371 = ORIENTED_EDGE ( 'NONE', *, *, #13322, .T. ) ;
#6372 = CARTESIAN_POINT ( 'NONE',  ( 0.000000000000000000, -4.992566952384716927, -37.16516213103282951 ) ) ;
#6373 = DIRECTION ( 'NONE',  ( -1.000000000000000000, -0.000000000000000000, 0.000000000000000000 ) ) ;
#6374 = FACE_OUTER_BOUND ( 'NONE', #40652, .T. ) ;
#6375 = CARTESIAN_POINT ( 'NONE',  ( 10.00000000000000000, -22.48208911017525580, 35.47612816024516036 ) ) ;
#6377 = AXIS2_PLACEMENT_3D ( 'NONE', #12519, #35019, #31127 ) ;
#6376 = DIRECTION ( 'NONE',  ( -1.000000000000000000, -0.000000000000000000, 0.000000000000000000 ) ) ;
#6378 = VECTOR ( 'NONE', #26092, 1000.000000000000000 ) ;
#6379 = LINE ( 'NONE', #14688, #36440 ) ;
#6380 = CARTESIAN_POINT ( 'NONE',  ( -235.0000123116479926, -123.0000000000000284, 2.500000000000000000 ) ) ;
#6381 = CIRCLE ( 'NONE', #33717, 12.50000000000000000 ) ;
#6382 = AXIS2_PLACEMENT_3D ( 'NONE', #41814, #46199, #38627 ) ;
#6383 = LINE ( 'NONE', #21290, #4170 ) ;
#6384 = CARTESIAN_POINT ( 'NONE',  ( -10.00000000000000000, 0.000000000000000000, 0.000000000000000000 ) ) ;
#6385 = DIRECTION ( 'NONE',  ( -0.000000000000000000, -1.156482317317870936E-15, -1.000000000000000000 ) ) ;
#6386 = DIRECTION ( 'NONE',  ( 0.000000000000000000, 0.000000000000000000, 1.000000000000000000 ) ) ;
#6387 = DIRECTION ( 'NONE',  ( -1.000000000000000000, -0.000000000000000000, -0.000000000000000000 ) ) ;
#6388 = VECTOR ( 'NONE', #11119, 1000.000000000000000 ) ;
#6389 = DIRECTION ( 'NONE',  ( -1.000000000000000000, 0.000000000000000000, 0.000000000000000000 ) ) ;
#6390 = AXIS2_PLACEMENT_3D ( 'NONE', #5160, #31352, #12733 ) ;
#6391 = DIRECTION ( 'NONE',  ( 1.000000000000000000, 0.000000000000000000, 0.000000000000000000 ) ) ;
#6392 = EDGE_LOOP ( 'NONE', ( #11950, #34082, #34418, #1382 ) ) ;
#6393 = ORIENTED_EDGE ( 'NONE', *, *, #38974, .T. ) ;
#6394 = EDGE_CURVE ( 'NONE', #47670, #25818, #27746, .T. ) ;
#6395 = LINE ( 'NONE', #18609, #39884 ) ;
#6396 = ORIENTED_EDGE ( 'NONE', *, *, #4953, .F. ) ;
#6397 = CARTESIAN_POINT ( 'NONE',  ( -10.00000000000000000, 0.000000000000000000, 0.000000000000000000 ) ) ;
#6398 = ORIENTED_EDGE ( 'NONE', *, *, #12184, .T. ) ;
#6399 = DIRECTION ( 'NONE',  ( 0.000000000000000000, 0.000000000000000000, 1.000000000000000000 ) ) ;
#6400 = EDGE_LOOP ( 'NONE', ( #26030, #10190, #21142, #41324 ) ) ;
#6401 = DIRECTION ( 'NONE',  ( 0.000000000000000000, 0.9945218953682731788, -0.1045284632676558162 ) ) ;
#6402 = ORIENTED_EDGE ( 'NONE', *, *, #13836, .F. ) ;
#6403 = CARTESIAN_POINT ( 'NONE',  ( 10.00000000000000000, 38.55633173627034438, -16.65560815589369881 ) ) ;
#6404 = ORIENTED_EDGE ( 'NONE', *, *, #40347, .T. ) ;
#6405 = EDGE_CURVE ( 'NONE', #47714, #15972, #18532, .T. ) ;
#6406 = CARTESIAN_POINT ( 'NONE',  ( 0.000000000000000000, 8.966570791700698706, 81.50828551894228724 ) ) ;
#6407 = AXIS2_PLACEMENT_3D ( 'NONE', #39221, #20607, #39473 ) ;
#6408 = VERTEX_POINT ( 'NONE', #40804 ) ;
#6409 = ORIENTED_EDGE ( 'NONE', *, *, #27106, .F. ) ;
#6410 = EDGE_CURVE ( 'NONE', #19329, #21447, #15998, .T. ) ;
#6411 = DIRECTION ( 'NONE',  ( 0.000000000000000000, -0.000000000000000000, 1.000000000000000000 ) ) ;
#6412 = AXIS2_PLACEMENT_3D ( 'NONE', #4025, #18928, #41470 ) ;
#6413 = DIRECTION ( 'NONE',  ( 0.5200609990132993854, 0.8541291221503274356, 0.000000000000000000 ) ) ;
#6414 = LINE ( 'NONE', #6179, #19254 ) ;
#6416 = EDGE_LOOP ( 'NONE', ( #6224, #35957, #42529, #14503 ) ) ;
#6415 = CARTESIAN_POINT ( 'NONE',  ( -10.00000000000000000, 0.000000000000000000, 0.000000000000000000 ) ) ;
#6417 = DIRECTION ( 'NONE',  ( 0.000000000000000000, 0.3826834323650907810, -0.9238795325112864054 ) ) ;
#6418 = ORIENTED_EDGE ( 'NONE', *, *, #20389, .T. ) ;
#6419 = LINE ( 'NONE', #25236, #21713 ) ;
#6420 = ORIENTED_EDGE ( 'NONE', *, *, #19768, .T. ) ;
#6421 = EDGE_LOOP ( 'NONE', ( #19900, #47515, #17849, #4464 ) ) ;
#6422 = EDGE_CURVE ( 'NONE', #36912, #41773, #8164, .T. ) ;
#6423 = CARTESIAN_POINT ( 'NONE',  ( 0.000000000000000000, -40.68715046381921496, -10.41901085202121280 ) ) ;
#6424 = DIRECTION ( 'NONE',  ( 0.000000000000000000, 0.000000000000000000, 1.000000000000000000 ) ) ;
#6425 = EDGE_LOOP ( 'NONE', ( #36637, #32832, #34219, #43736 ) ) ;
#6426 = DIRECTION ( 'NONE',  ( -1.000000000000000000, -0.000000000000000000, 0.000000000000000000 ) ) ;
#6427 = EDGE_CURVE ( 'NONE', #38433, #37023, #38682, .T. ) ;
#6428 = DIRECTION ( 'NONE',  ( 0.000000000000000000, 0.000000000000000000, 1.000000000000000000 ) ) ;
#6429 = CARTESIAN_POINT ( 'NONE',  ( 10.00000000000000000, -55.38113227695820484, 54.21277698773656084 ) ) ;
#6430 = ORIENTED_EDGE ( 'NONE', *, *, #41673, .T. ) ;
#6431 = CARTESIAN_POINT ( 'NONE',  ( 0.000000000000000000, 22.07842321921481243, 8.187992925817422218 ) ) ;
#6432 = DIRECTION ( 'NONE',  ( -1.000000000000000000, -0.000000000000000000, -0.000000000000000000 ) ) ;
#6433 = DIRECTION ( 'NONE',  ( 0.9781476007338069101, 0.000000000000000000, -0.2079116908177528755 ) ) ;
#6434 = DIRECTION ( 'NONE',  ( -0.9997280174009349762, 0.02332147558787823691, 0.000000000000000000 ) ) ;
#6435 = ORIENTED_EDGE ( 'NONE', *, *, #41297, .F. ) ;
#6436 = CARTESIAN_POINT ( 'NONE',  ( 10.00000000000000000, 0.000000000000000000, 0.000000000000000000 ) ) ;
#6437 = DIRECTION ( 'NONE',  ( 0.000000000000000000, -0.1564344650402382242, 0.9876883405951366601 ) ) ;
#6438 = DIRECTION ( 'NONE',  ( 1.000000000000000000, 0.000000000000000000, 0.000000000000000000 ) ) ;
#6439 = CARTESIAN_POINT ( 'NONE',  ( 10.00000000000000000, 0.000000000000000000, 0.000000000000000000 ) ) ;
#6440 = ADVANCED_FACE ( 'NONE', ( #37615 ), #4091, .T. ) ;
#6441 = DIRECTION ( 'NONE',  ( 0.000000000000000000, 0.1564344650402311743, -0.9876883405951377704 ) ) ;
#6442 = DIRECTION ( 'NONE',  ( 0.000000000000000000, 0.5877852522924689183, -0.8090169943749504489 ) ) ;
#6443 = ORIENTED_EDGE ( 'NONE', *, *, #26048, .F. ) ;
#6444 = VERTEX_POINT ( 'NONE', #32968 ) ;
#6445 = FACE_OUTER_BOUND ( 'NONE', #10484, .T. ) ;
#6446 = ORIENTED_EDGE ( 'NONE', *, *, #13047, .T. ) ;
#6447 = DIRECTION ( 'NONE',  ( 0.000000000000000000, -6.938893903907228378E-15, 1.000000000000000000 ) ) ;
#6448 = AXIS2_PLACEMENT_3D ( 'NONE', #46517, #23500, #8805 ) ;
#6449 = DIRECTION ( 'NONE',  ( 0.000000000000000000, 0.5224985647159499091, -0.8526401643540916231 ) ) ;
#6450 = VECTOR ( 'NONE', #19305, 1000.000000000000000 ) ;
#6451 = VERTEX_POINT ( 'NONE', #47892 ) ;
#6452 = EDGE_CURVE ( 'NONE', #9450, #17448, #7264, .T. ) ;
#6453 = CIRCLE ( 'NONE', #46321, 82.00000000000000000 ) ;
#6454 = EDGE_CURVE ( 'NONE', #27530, #26745, #19890, .T. ) ;
#6455 = LINE ( 'NONE', #46854, #244 ) ;
#6456 = EDGE_LOOP ( 'NONE', ( #18719, #29465, #34263, #24472 ) ) ;
#6457 = EDGE_CURVE ( 'NONE', #13942, #20542, #5841, .T. ) ;
#6458 = DIRECTION ( 'NONE',  ( -0.000000000000000000, -0.000000000000000000, -1.000000000000000000 ) ) ;
#6459 = ORIENTED_EDGE ( 'NONE', *, *, #35350, .T. ) ;
#6460 = CARTESIAN_POINT ( 'NONE',  ( 0.000000000000000000, -55.19960302592104284, 51.03279382321070301 ) ) ;
#6461 = DIRECTION ( 'NONE',  ( 0.000000000000000000, -0.9510565162951565288, 0.3090169943749382919 ) ) ;
#6462 = CIRCLE ( 'NONE', #33813, 42.00000000000000000 ) ;
#6463 = VERTEX_POINT ( 'NONE', #3843 ) ;
#6464 = CARTESIAN_POINT ( 'NONE',  ( 11.99999999999999822, 63.18004540533030422, 44.88180994100399346 ) ) ;
#6465 = VECTOR ( 'NONE', #4473, 1000.000000000000000 ) ;
#6466 = ADVANCED_FACE ( 'NONE', ( #18755 ), #157, .T. ) ;
#6467 = VERTEX_POINT ( 'NONE', #44965 ) ;
#6468 = EDGE_CURVE ( 'NONE', #12529, #20404, #17555, .T. ) ;
#6469 = EDGE_CURVE ( 'NONE', #7278, #16579, #23820, .T. ) ;
#6470 = CARTESIAN_POINT ( 'NONE',  ( 11.99999999999999822, -2.956366410620109519, -75.11725578898472122 ) ) ;
#6471 = CYLINDRICAL_SURFACE ( 'NONE', #10078, 31.99999999999998579 ) ;
#6472 = CARTESIAN_POINT ( 'NONE',  ( -10.00000000000000000, 0.000000000000000000, 0.000000000000000000 ) ) ;
#6473 = AXIS2_PLACEMENT_3D ( 'NONE', #44602, #45094, #44366 ) ;
#6474 = ORIENTED_EDGE ( 'NONE', *, *, #9300, .T. ) ;
#6475 = PLANE ( 'NONE',  #41218 ) ;
#6476 = ORIENTED_EDGE ( 'NONE', *, *, #13604, .T. ) ;
#6477 = VERTEX_POINT ( 'NONE', #48147 ) ;
#6478 = CIRCLE ( 'NONE', #1805, 77.49900000000000944 ) ;
#6479 = CARTESIAN_POINT ( 'NONE',  ( 6.000000000000000000, 3.894527615417885169, 81.90746397400390322 ) ) ;
#6480 = CARTESIAN_POINT ( 'NONE',  ( 0.000000000000000000, 2.543863470248399761, 81.96053171279903893 ) ) ;
#6481 = AXIS2_PLACEMENT_3D ( 'NONE', #23442, #41823, #4852 ) ;
#6482 = DIRECTION ( 'NONE',  ( 0.000000000000000000, 0.000000000000000000, 1.000000000000000000 ) ) ;
#6483 = DIRECTION ( 'NONE',  ( 1.000000000000000000, 0.000000000000000000, 0.000000000000000000 ) ) ;
#6484 = DIRECTION ( 'NONE',  ( 0.000000000000000000, -1.000000000000000000, 0.000000000000000000 ) ) ;
#6485 = VECTOR ( 'NONE', #48386, 1000.000000000000000 ) ;
#6486 = CARTESIAN_POINT ( 'NONE',  ( 0.000000000000000000, -22.48208911017525580, 35.47612816024516036 ) ) ;
#6487 = CYLINDRICAL_SURFACE ( 'NONE', #20344, 31.99999999999998579 ) ;
#6488 = CARTESIAN_POINT ( 'NONE',  ( 10.00000000000000000, 0.000000000000000000, 0.000000000000000000 ) ) ;
#6489 = DIRECTION ( 'NONE',  ( 1.000000000000000000, -0.000000000000000000, -0.000000000000000000 ) ) ;
#6490 = DIRECTION ( 'NONE',  ( 0.000000000000000000, 0.000000000000000000, 1.000000000000000000 ) ) ;
#6491 = ORIENTED_EDGE ( 'NONE', *, *, #10060, .F. ) ;
#6492 = AXIS2_PLACEMENT_3D ( 'NONE', #9368, #16483, #39736 ) ;
#6493 = DIRECTION ( 'NONE',  ( -1.000000000000000000, -0.000000000000000000, 0.000000000000000000 ) ) ;
#6494 = CIRCLE ( 'NONE', #39301, 37.49900000000001654 ) ;
#6495 = LINE ( 'NONE', #21414, #940 ) ;
#6496 = DIRECTION ( 'NONE',  ( -1.000000000000000000, 0.000000000000000000, 0.000000000000000000 ) ) ;
#6497 = CARTESIAN_POINT ( 'NONE',  ( 0.000000000000000000, -74.18225833017864090, -34.94270380257719211 ) ) ;
#6498 = DIRECTION ( 'NONE',  ( 0.000000000000000000, 0.9510565162951536422, 0.3090169943749471182 ) ) ;
#6499 = DIRECTION ( 'NONE',  ( 0.000000000000000000, 0.5877852522924685852, 0.8090169943749507819 ) ) ;
#6500 = ORIENTED_EDGE ( 'NONE', *, *, #32399, .T. ) ;
#6501 = LINE ( 'NONE', #47389, #32455 ) ;
#6502 = AXIS2_PLACEMENT_3D ( 'NONE', #17383, #25937, #44785 ) ;
#6503 = DIRECTION ( 'NONE',  ( 0.000000000000000000, 0.4539904997395414754, 0.8910065241883706744 ) ) ;
#6504 = ORIENTED_EDGE ( 'NONE', *, *, #34702, .F. ) ;
#6505 = ORIENTED_EDGE ( 'NONE', *, *, #42634, .F. ) ;
#6506 = AXIS2_PLACEMENT_3D ( 'NONE', #39913, #39687, #9322 ) ;
#6507 = EDGE_CURVE ( 'NONE', #46808, #34289, #29547, .T. ) ;
#6508 = ORIENTED_EDGE ( 'NONE', *, *, #27807, .F. ) ;
#6509 = CIRCLE ( 'NONE', #21355, 77.49900000000000944 ) ;
#6510 = CIRCLE ( 'NONE', #40888, 42.00000000000000000 ) ;
#6511 = EDGE_CURVE ( 'NONE', #43483, #24537, #10943, .T. ) ;
#6512 = LINE ( 'NONE', #43951, #26506 ) ;
#6513 = ORIENTED_EDGE ( 'NONE', *, *, #11266, .F. ) ;
#6514 = ADVANCED_FACE ( 'NONE', ( #20893 ), #19972, .T. ) ;
#6515 = VECTOR ( 'NONE', #5058, 1000.000000000000000 ) ;
#6516 = AXIS2_PLACEMENT_3D ( 'NONE', #21127, #2775, #10126 ) ;
#6517 = AXIS2_PLACEMENT_3D ( 'NONE', #9676, #39067, #5530 ) ;
#6518 = CYLINDRICAL_SURFACE ( 'NONE', #39468, 37.49900000000000233 ) ;
#6519 = CYLINDRICAL_SURFACE ( 'NONE', #29678, 82.00000000000000000 ) ;
#6520 = EDGE_CURVE ( 'NONE', #44447, #37633, #6625, .T. ) ;
#6521 = AXIS2_PLACEMENT_3D ( 'NONE', #6698, #21628, #22352 ) ;
#6522 = DIRECTION ( 'NONE',  ( -0.000000000000000000, 0.4999999999999921174, -0.8660254037844432595 ) ) ;
#6523 = VERTEX_POINT ( 'NONE', #2277 ) ;
#6524 = LINE ( 'NONE', #37344, #17214 ) ;
#6525 = ORIENTED_EDGE ( 'NONE', *, *, #39348, .T. ) ;
#6526 = ORIENTED_EDGE ( 'NONE', *, *, #26275, .T. ) ;
#6527 = AXIS2_PLACEMENT_3D ( 'NONE', #26680, #41605, #22523 ) ;
#6528 = EDGE_CURVE ( 'NONE', #2585, #21915, #879, .T. ) ;
#6529 = CARTESIAN_POINT ( 'NONE',  ( 19.29194287201271862, -133.5026271600380880, -5.500000000000000000 ) ) ;
#6531 = ORIENTED_EDGE ( 'NONE', *, *, #35711, .F. ) ;
#6530 = LINE ( 'NONE', #28801, #43060 ) ;
#6532 = DIRECTION ( 'NONE',  ( 0.000000000000000000, 0.000000000000000000, 1.000000000000000000 ) ) ;
#6533 = ORIENTED_EDGE ( 'NONE', *, *, #35034, .T. ) ;
#6534 = ORIENTED_EDGE ( 'NONE', *, *, #35331, .F. ) ;
#6535 = CARTESIAN_POINT ( 'NONE',  ( -10.00000000000000000, 0.000000000000000000, 0.000000000000000000 ) ) ;
#6536 = ORIENTED_EDGE ( 'NONE', *, *, #10271, .F. ) ;
#6537 = DIRECTION ( 'NONE',  ( -1.000000000000000000, 0.000000000000000000, 0.000000000000000000 ) ) ;
#6538 = DIRECTION ( 'NONE',  ( -1.000000000000000000, -0.000000000000000000, -0.000000000000000000 ) ) ;
#6539 = EDGE_LOOP ( 'NONE', ( #35893, #31986, #26321, #29072 ) ) ;
#6540 = DIRECTION ( 'NONE',  ( -1.000000000000000000, -0.000000000000000000, -0.000000000000000000 ) ) ;
#6541 = CYLINDRICAL_SURFACE ( 'NONE', #47142, 31.99999999999998579 ) ;
#6542 = CIRCLE ( 'NONE', #12800, 42.00000000000000000 ) ;
#6543 = EDGE_CURVE ( 'NONE', #41290, #40106, #46502, .T. ) ;
#6544 = DIRECTION ( 'NONE',  ( -1.000000000000000000, -0.000000000000000000, 0.000000000000000000 ) ) ;
#6545 = ORIENTED_EDGE ( 'NONE', *, *, #37260, .T. ) ;
#6546 = FACE_OUTER_BOUND ( 'NONE', #18308, .T. ) ;
#6547 = ORIENTED_EDGE ( 'NONE', *, *, #24470, .F. ) ;
#6548 = VECTOR ( 'NONE', #19462, 1000.000000000000000 ) ;
#6549 = VECTOR ( 'NONE', #3831, 1000.000000000000000 ) ;
#6550 = CIRCLE ( 'NONE', #32342, 31.99999999999998224 ) ;
#6551 = DIRECTION ( 'NONE',  ( -1.000000000000000000, 0.000000000000000000, 0.000000000000000000 ) ) ;
#6552 = CARTESIAN_POINT ( 'NONE',  ( -0.9515373497862389396, -96.47140937769621871, 5.500000000000000000 ) ) ;
#6553 = FACE_OUTER_BOUND ( 'NONE', #4318, .T. ) ;
#6554 = DIRECTION ( 'NONE',  ( 0.000000000000000000, 0.000000000000000000, 1.000000000000000000 ) ) ;
#6555 = CARTESIAN_POINT ( 'NONE',  ( 0.000000000000000000, -77.49459641780886443, 0.8261519478428377417 ) ) ;
#6556 = AXIS2_PLACEMENT_3D ( 'NONE', #24763, #39934, #35283 ) ;
#6557 = AXIS2_PLACEMENT_3D ( 'NONE', #9151, #24084, #36299 ) ;
#6558 = DIRECTION ( 'NONE',  ( 0.000000000000000000, 0.1564344650402243742, 0.9876883405951387696 ) ) ;
#6559 = DIRECTION ( 'NONE',  ( 0.000000000000000000, 0.000000000000000000, 1.000000000000000000 ) ) ;
#6560 = CARTESIAN_POINT ( 'NONE',  ( 0.000000000000000000, 0.000000000000000000, 0.000000000000000000 ) ) ;
#6561 = AXIS2_PLACEMENT_3D ( 'NONE', #38454, #12753, #1259 ) ;
#6562 = VECTOR ( 'NONE', #19546, 1000.000000000000000 ) ;
#6563 = CARTESIAN_POINT ( 'NONE',  ( 10.00000000000000000, 74.65491531819118620, -8.830959090342659579 ) ) ;
#6564 = CIRCLE ( 'NONE', #31598, 16.00000000000000000 ) ;
#6565 = VERTEX_POINT ( 'NONE', #8238 ) ;
#6566 = ORIENTED_EDGE ( 'NONE', *, *, #32592, .T. ) ;
#6567 = ORIENTED_EDGE ( 'NONE', *, *, #43111, .T. ) ;
#6568 = EDGE_CURVE ( 'NONE', #18661, #41940, #15581, .T. ) ;
#6569 = PLANE ( 'NONE',  #24928 ) ;
#6570 = CARTESIAN_POINT ( 'NONE',  ( -26.29030328629083968, -123.6496510949466341, 5.500000000000000000 ) ) ;
#6571 = ORIENTED_EDGE ( 'NONE', *, *, #20567, .T. ) ;
#6572 = EDGE_CURVE ( 'NONE', #5905, #22595, #31634, .T. ) ;
#6573 = CIRCLE ( 'NONE', #26105, 42.00000000000000000 ) ;
#6574 = EDGE_CURVE ( 'NONE', #1101, #9926, #37870, .T. ) ;
#6575 = DIRECTION ( 'NONE',  ( -1.000000000000000000, 0.000000000000000000, 0.000000000000000000 ) ) ;
#6576 = AXIS2_PLACEMENT_3D ( 'NONE', #21345, #24303, #14680 ) ;
#6577 = VECTOR ( 'NONE', #20709, 1000.000000000000114 ) ;
#6578 = EDGE_LOOP ( 'NONE', ( #20952, #45917, #31199, #13156 ) ) ;
#6579 = VERTEX_POINT ( 'NONE', #7983 ) ;
#6580 = ORIENTED_EDGE ( 'NONE', *, *, #30120, .F. ) ;
#6581 = AXIS2_PLACEMENT_3D ( 'NONE', #32820, #35787, #17171 ) ;
#6582 = ADVANCED_FACE ( 'NONE', ( #46169 ), #22919, .T. ) ;
#6583 = DIRECTION ( 'NONE',  ( 0.000000000000000000, 0.000000000000000000, 1.000000000000000000 ) ) ;
#6584 = CIRCLE ( 'NONE', #9729, 82.00000000000000000 ) ;
#6585 = ORIENTED_EDGE ( 'NONE', *, *, #43924, .F. ) ;
#6586 = DIRECTION ( 'NONE',  ( 0.000000000000000000, -0.8090169943749402348, -0.5877852522924830181 ) ) ;
#6587 = EDGE_CURVE ( 'NONE', #19725, #28510, #17197, .T. ) ;
#6588 = EDGE_LOOP ( 'NONE', ( #801, #12507, #1276, #31279 ) ) ;
#6589 = AXIS2_PLACEMENT_3D ( 'NONE', #31311, #20032, #30568 ) ;
#6590 = CARTESIAN_POINT ( 'NONE',  ( 10.00000000000000000, -46.53671651293991118, 59.03961581697383565 ) ) ;
#6591 = CIRCLE ( 'NONE', #8166, 37.49900000000000233 ) ;
#6592 = FACE_OUTER_BOUND ( 'NONE', #235, .T. ) ;
#6593 = DIRECTION ( 'NONE',  ( 1.000000000000000000, -0.000000000000000000, -0.000000000000000000 ) ) ;
#6595 = ORIENTED_EDGE ( 'NONE', *, *, #23769, .F. ) ;
#6594 = VECTOR ( 'NONE', #11990, 1000.000000000000000 ) ;
#6596 = FACE_OUTER_BOUND ( 'NONE', #19497, .T. ) ;
#6597 = VERTEX_POINT ( 'NONE', #30759 ) ;
#6598 = LINE ( 'NONE', #21992, #8607 ) ;
#6599 = EDGE_CURVE ( 'NONE', #21733, #3134, #5975, .T. ) ;
#6600 = DIRECTION ( 'NONE',  ( 0.000000000000000000, 0.9876883405951381034, -0.1564344650402276216 ) ) ;
#6601 = ORIENTED_EDGE ( 'NONE', *, *, #20273, .F. ) ;
#6602 = VERTEX_POINT ( 'NONE', #45437 ) ;
#6603 = CARTESIAN_POINT ( 'NONE',  ( -8.452893869119503023, -12.51233732111638375, -1.199999999999999956 ) ) ;
#6604 = LINE ( 'NONE', #26834, #19928 ) ;
#6605 = ORIENTED_EDGE ( 'NONE', *, *, #48184, .T. ) ;
#6606 = ORIENTED_EDGE ( 'NONE', *, *, #4144, .F. ) ;
#6607 = FACE_OUTER_BOUND ( 'NONE', #36212, .T. ) ;
#6608 = LINE ( 'NONE', #47701, #17267 ) ;
#6609 = DIRECTION ( 'NONE',  ( 0.000000000000000000, 0.000000000000000000, 1.000000000000000000 ) ) ;
#6610 = DIRECTION ( 'NONE',  ( 0.000000000000000000, -0.8090169943749532244, 0.5877852522924652545 ) ) ;
#6611 = DIRECTION ( 'NONE',  ( 0.000000000000000000, -0.1564344650402381687, 0.9876883405951365491 ) ) ;
#6612 = EDGE_CURVE ( 'NONE', #30788, #44254, #41820, .T. ) ;
#6613 = CARTESIAN_POINT ( 'NONE',  ( 0.000000000000000000, -75.11764819372145041, -2.946379043147127064 ) ) ;
#6614 = CARTESIAN_POINT ( 'NONE',  ( 11.99999999999999822, 80.28980883073781172, -16.65972982744850128 ) ) ;
#6615 = CIRCLE ( 'NONE', #29295, 82.00000000000000000 ) ;
#6616 = AXIS2_PLACEMENT_3D ( 'NONE', #35091, #42696, #9153 ) ;
#6617 = DIRECTION ( 'NONE',  ( -1.000000000000000000, -0.000000000000000000, 0.000000000000000000 ) ) ;
#6618 = DIRECTION ( 'NONE',  ( -0.000000000000000000, -0.9135454576426006446, 0.4067366430758008744 ) ) ;
#6619 = DIRECTION ( 'NONE',  ( 0.000000000000000000, 0.000000000000000000, 1.000000000000000000 ) ) ;
#6620 = PLANE ( 'NONE',  #45155 ) ;
#6621 = ORIENTED_EDGE ( 'NONE', *, *, #21255, .T. ) ;
#6622 = ORIENTED_EDGE ( 'NONE', *, *, #14535, .T. ) ;
#6623 = VERTEX_POINT ( 'NONE', #19251 ) ;
#6624 = AXIS2_PLACEMENT_3D ( 'NONE', #18498, #41032, #41266 ) ;
#6625 = CIRCLE ( 'NONE', #25380, 32.00000000000000000 ) ;
#6626 = EDGE_CURVE ( 'NONE', #26799, #41107, #35562, .T. ) ;
#6627 = CARTESIAN_POINT ( 'NONE',  ( 0.000000000000000000, 55.16347631943042984, 60.67117009219156643 ) ) ;
#6628 = AXIS2_PLACEMENT_3D ( 'NONE', #47794, #28960, #37277 ) ;
#6629 = EDGE_CURVE ( 'NONE', #16756, #29948, #38106, .T. ) ;
#6630 = AXIS2_PLACEMENT_3D ( 'NONE', #40445, #10584, #44347 ) ;
#6631 = ORIENTED_EDGE ( 'NONE', *, *, #34301, .T. ) ;
#6632 = CARTESIAN_POINT ( 'NONE',  ( 0.000000000000000000, 68.67312586195046720, -35.91791733033402068 ) ) ;
#6633 = ORIENTED_EDGE ( 'NONE', *, *, #31194, .T. ) ;
#6634 = ADVANCED_FACE ( 'NONE', ( #19473 ), #45683, .F. ) ;
#6636 = ORIENTED_EDGE ( 'NONE', *, *, #606, .F. ) ;
#6635 = EDGE_CURVE ( 'NONE', #24182, #45282, #1958, .T. ) ;
#6637 = ADVANCED_FACE ( 'NONE', ( #38338 ), #652, .T. ) ;
#6638 = APPLICATION_CONTEXT ( 'automotive_design' ) ;
#6639 = LINE ( 'NONE', #7107, #12536 ) ;
#6640 = ORIENTED_EDGE ( 'NONE', *, *, #23097, .T. ) ;
#6641 = DIRECTION ( 'NONE',  ( 0.000000000000000000, -0.9876883405951394357, 0.1564344650402205716 ) ) ;
#6642 = EDGE_LOOP ( 'NONE', ( #43292, #15147, #23849, #11945 ) ) ;
#6643 = DIRECTION ( 'NONE',  ( 0.000000000000000000, 1.000000000000000000, 3.491481338843133750E-15 ) ) ;
#6644 = AXIS2_PLACEMENT_3D ( 'NONE', #43037, #39122, #5592 ) ;
#6645 = ORIENTED_EDGE ( 'NONE', *, *, #5131, .F. ) ;
#6646 = FACE_OUTER_BOUND ( 'NONE', #47628, .T. ) ;
#6647 = DIRECTION ( 'NONE',  ( 0.000000000000000000, 0.000000000000000000, 1.000000000000000000 ) ) ;
#6648 = ORIENTED_EDGE ( 'NONE', *, *, #32023, .T. ) ;
#6649 = VECTOR ( 'NONE', #19644, 1000.000000000000000 ) ;
#6650 = CARTESIAN_POINT ( 'NONE',  ( 0.000000000000000000, -63.18004540533059554, 44.88180994100355292 ) ) ;
#6651 = EDGE_LOOP ( 'NONE', ( #39538, #36206 ) ) ;
#6652 = CARTESIAN_POINT ( 'NONE',  ( 0.000000000000000000, 0.000000000000000000, 0.000000000000000000 ) ) ;
#6653 = EDGE_LOOP ( 'NONE', ( #1824, #10538, #17823, #16848 ) ) ;
#6654 = CARTESIAN_POINT ( 'NONE',  ( 0.000000000000000000, -75.54627589209955829, 17.28742895386058009 ) ) ;
#6655 = ORIENTED_EDGE ( 'NONE', *, *, #11804, .F. ) ;
#6656 = CARTESIAN_POINT ( 'NONE',  ( -12.50000000000000000, -132.5000000000000000, 2.500000000000000000 ) ) ;
#6657 = CARTESIAN_POINT ( 'NONE',  ( -12.50000000000000000, -107.5000000000000000, -40.00000000000000000 ) ) ;
#6658 = CARTESIAN_POINT ( 'NONE',  ( 0.000000000000000000, 34.44570377933695227, -69.42325613327405165 ) ) ;
#6659 = ADVANCED_FACE ( 'NONE', ( #22073 ), #18150, .T. ) ;
#6660 = CARTESIAN_POINT ( 'NONE',  ( 0.000000000000000000, -3.925862922255855647, -41.81611651403866858 ) ) ;
#6661 = AXIS2_PLACEMENT_3D ( 'NONE', #28506, #10132, #36076 ) ;
#6662 = AXIS2_PLACEMENT_3D ( 'NONE', #41009, #33172, #33883 ) ;
#6663 = VERTEX_POINT ( 'NONE', #10601 ) ;
#6664 = DIRECTION ( 'NONE',  ( 0.6575728627325957421, -0.7533909544171994987, 0.000000000000000000 ) ) ;
#6665 = VERTEX_POINT ( 'NONE', #6206 ) ;
#6666 = EDGE_LOOP ( 'NONE', ( #44708, #36141, #4847, #6100 ) ) ;
#6667 = DIRECTION ( 'NONE',  ( -1.000000000000000000, -0.000000000000000000, 0.000000000000000000 ) ) ;
#6668 = LINE ( 'NONE', #18398, #48061 ) ;
#6669 = FACE_OUTER_BOUND ( 'NONE', #32545, .T. ) ;
#6670 = CIRCLE ( 'NONE', #15271, 82.00000000000000000 ) ;
#6671 = DIRECTION ( 'NONE',  ( -1.000000000000000000, 0.000000000000000000, -0.000000000000000000 ) ) ;
#6672 = LINE ( 'NONE', #44109, #43824 ) ;
#6673 = ORIENTED_EDGE ( 'NONE', *, *, #10947, .F. ) ;
#6674 = EDGE_CURVE ( 'NONE', #12729, #23160, #40459, .T. ) ;
#6675 = AXIS2_PLACEMENT_3D ( 'NONE', #24838, #17730, #47366 ) ;
#6676 = DIRECTION ( 'NONE',  ( 1.000000000000000000, 0.000000000000000000, 0.000000000000000000 ) ) ;
#6677 = AXIS2_PLACEMENT_3D ( 'NONE', #8804, #32301, #17348 ) ;
#6678 = DIRECTION ( 'NONE',  ( -0.8541291221503265474, 0.5200609990133007177, 0.000000000000000000 ) ) ;
#6679 = FACE_OUTER_BOUND ( 'NONE', #14679, .T. ) ;
#6680 = EDGE_LOOP ( 'NONE', ( #33457, #43610, #43331, #24165, #18798, #35762, #30907, #43194 ) ) ;
#6681 = AXIS2_PLACEMENT_3D ( 'NONE', #47770, #6683, #47069 ) ;
#6682 = CYLINDRICAL_SURFACE ( 'NONE', #25462, 31.99999999999999289 ) ;
#6683 = DIRECTION ( 'NONE',  ( -1.000000000000000000, -0.000000000000000000, -0.000000000000000000 ) ) ;
#6684 = FACE_OUTER_BOUND ( 'NONE', #16270, .T. ) ;
#6685 = DIRECTION ( 'NONE',  ( -1.000000000000000000, -0.000000000000000000, 0.000000000000000000 ) ) ;
#6686 = CYLINDRICAL_SURFACE ( 'NONE', #4891, 42.00000000000000000 ) ;
#6687 = FACE_OUTER_BOUND ( 'NONE', #18730, .T. ) ;
#6688 = DIRECTION ( 'NONE',  ( -1.000000000000000000, -0.000000000000000000, -0.000000000000000000 ) ) ;
#6689 = CARTESIAN_POINT ( 'NONE',  ( 15.00000000000000000, -10.45096189432344502, -21.10159698893425784 ) ) ;
#6690 = ORIENTED_EDGE ( 'NONE', *, *, #34104, .T. ) ;
#6691 = ORIENTED_EDGE ( 'NONE', *, *, #11289, .T. ) ;
#6692 = CIRCLE ( 'NONE', #21529, 31.99999999999998934 ) ;
#6693 = LINE ( 'NONE', #33354, #16797 ) ;
#6694 = VERTEX_POINT ( 'NONE', #39981 ) ;
#6695 = EDGE_CURVE ( 'NONE', #19747, #37030, #3599, .T. ) ;
#6696 = DIRECTION ( 'NONE',  ( -1.000000000000000000, 0.000000000000000000, 0.000000000000000000 ) ) ;
#6697 = EDGE_CURVE ( 'NONE', #34109, #35947, #25027, .T. ) ;
#6698 = CARTESIAN_POINT ( 'NONE',  ( -10.00000000000000000, 0.000000000000000000, 0.000000000000000000 ) ) ;
#6699 = ORIENTED_EDGE ( 'NONE', *, *, #46549, .F. ) ;
#6700 = VECTOR ( 'NONE', #42161, 1000.000000000000000 ) ;
#6701 = ADVANCED_FACE ( 'NONE', ( #47322 ), #17918, .F. ) ;
#6702 = CARTESIAN_POINT ( 'NONE',  ( 11.99999999999999822, -6.903761155837269570, -77.19088730480530103 ) ) ;
#6703 = CIRCLE ( 'NONE', #32489, 31.99999999999999289 ) ;
#6705 = ADVANCED_FACE ( 'NONE', ( #43641 ), #32845, .T. ) ;
#6704 = VERTEX_POINT ( 'NONE', #3227 ) ;
#6706 = AXIS2_PLACEMENT_3D ( 'NONE', #28922, #24068, #32605 ) ;
#6707 = CARTESIAN_POINT ( 'NONE',  ( -3.000000000000000000, 0.000000000000000000, 0.000000000000000000 ) ) ;
#6708 = ORIENTED_EDGE ( 'NONE', *, *, #2932, .F. ) ;
#6709 = CARTESIAN_POINT ( 'NONE',  ( 11.99999999999999822, -55.19960302592104284, 51.03279382321070301 ) ) ;
#6710 = DIRECTION ( 'NONE',  ( 0.000000000000000000, -0.1045284632676449221, 0.9945218953682741780 ) ) ;
#6711 = ORIENTED_EDGE ( 'NONE', *, *, #25405, .F. ) ;
#6712 = DIRECTION ( 'NONE',  ( 1.000000000000000000, 0.000000000000000000, 0.000000000000000000 ) ) ;
#6713 = CIRCLE ( 'NONE', #13743, 31.99999999999999645 ) ;
#6714 = VERTEX_POINT ( 'NONE', #47543 ) ;
#6715 = LINE ( 'NONE', #43673, #5374 ) ;
#6716 = DIRECTION ( 'NONE',  ( 0.000000000000000000, 0.000000000000000000, 1.000000000000000000 ) ) ;
#6717 = DIRECTION ( 'NONE',  ( 0.000000000000000000, 0.000000000000000000, 1.000000000000000000 ) ) ;
#6718 = CIRCLE ( 'NONE', #14521, 37.49900000000000233 ) ;
#6719 = VERTEX_POINT ( 'NONE', #9869 ) ;
#6720 = CARTESIAN_POINT ( 'NONE',  ( 0.000000000000000000, 16.65560815589464028, -38.55633173626993226 ) ) ;
#6721 = VERTEX_POINT ( 'NONE', #17694 ) ;
#6722 = ORIENTED_EDGE ( 'NONE', *, *, #35044, .F. ) ;
#6723 = CARTESIAN_POINT ( 'NONE',  ( 0.000000000000000000, 0.000000000000000000, 0.000000000000000000 ) ) ;
#6724 = DIRECTION ( 'NONE',  ( -1.000000000000000000, 0.000000000000000000, 0.000000000000000000 ) ) ;
#6725 = CARTESIAN_POINT ( 'NONE',  ( 0.000000000000000000, 0.000000000000000000, 0.000000000000000000 ) ) ;
#6726 = CARTESIAN_POINT ( 'NONE',  ( -2.500000000000000000, 16.00000000000000000, -10.00000000000000178 ) ) ;
#6727 = ORIENTED_EDGE ( 'NONE', *, *, #39568, .F. ) ;
#6728 = CARTESIAN_POINT ( 'NONE',  ( 0.000000000000000000, -26.08949754953005495, -27.05870788708258701 ) ) ;
#6729 = COLOUR_RGB ( '', 0.09019608, 0.27058824, 0.51372549) ;
#6730 = DIRECTION ( 'NONE',  ( 0.000000000000000000, 0.000000000000000000, 1.000000000000000000 ) ) ;
#6731 = CARTESIAN_POINT ( 'NONE',  ( 10.00000000000000000, -55.20638768913724448, -51.02545421589383068 ) ) ;
#6732 = CARTESIAN_POINT ( 'NONE',  ( 13.83832728059186046, -142.6495187161941089, 5.500000000000000000 ) ) ;
#6733 = DIRECTION ( 'NONE',  ( -1.000000000000000000, 0.000000000000000000, 0.000000000000000000 ) ) ;
#6734 = VECTOR ( 'NONE', #19810, 1000.000000000000000 ) ;
#6735 = ORIENTED_EDGE ( 'NONE', *, *, #1825, .F. ) ;
#6736 = DIRECTION ( 'NONE',  ( 0.000000000000000000, 0.000000000000000000, 1.000000000000000000 ) ) ;
#6737 = EDGE_CURVE ( 'NONE', #23206, #40594, #25511, .T. ) ;
#6738 = VECTOR ( 'NONE', #46836, 1000.000000000000000 ) ;
#6739 = DIRECTION ( 'NONE',  ( -0.000000000000000000, -0.000000000000000000, 1.000000000000000000 ) ) ;
#6740 = LINE ( 'NONE', #3286, #15127 ) ;
#6741 = VECTOR ( 'NONE', #9307, 1000.000000000000000 ) ;
#6742 = DIRECTION ( 'NONE',  ( 0.000000000000000000, 0.000000000000000000, 1.000000000000000000 ) ) ;
#6743 = DIRECTION ( 'NONE',  ( 0.000000000000000000, 0.000000000000000000, 1.000000000000000000 ) ) ;
#6744 = CARTESIAN_POINT ( 'NONE',  ( 24.95699195200416654, -110.9640411295978595, 5.500000000000000000 ) ) ;
#6745 = CLOSED_SHELL ( 'NONE', ( #35945, #26592, #34256, #14741, #7793, #6701, #7128, #14982, #2824, #10559 ) ) ;
#6746 = ORIENTED_EDGE ( 'NONE', *, *, #17388, .F. ) ;
#6747 = CARTESIAN_POINT ( 'NONE',  ( 0.000000000000000000, 75.11764819372142199, 2.946379043147685728 ) ) ;
#6748 = AXIS2_PLACEMENT_3D ( 'NONE', #2509, #28476, #43413 ) ;
#6749 = EDGE_CURVE ( 'NONE', #23663, #14950, #13795, .T. ) ;
#6750 = CIRCLE ( 'NONE', #38801, 37.49900000000000944 ) ;
#6751 = DIRECTION ( 'NONE',  ( -0.000000000000000000, -0.3090169943749450088, 0.9510565162951543083 ) ) ;
#6752 = EDGE_CURVE ( 'NONE', #19028, #19153, #48026, .T. ) ;
#6753 = EDGE_CURVE ( 'NONE', #42541, #844, #44363, .T. ) ;
#6754 = ORIENTED_EDGE ( 'NONE', *, *, #48050, .T. ) ;
#6755 = ORIENTED_EDGE ( 'NONE', *, *, #19544, .T. ) ;
#6756 = CIRCLE ( 'NONE', #13025, 15.99999999999999645 ) ;
#6757 = EDGE_CURVE ( 'NONE', #31795, #27602, #34862, .T. ) ;
#6758 = EDGE_LOOP ( 'NONE', ( #14043, #10490, #47477, #40623 ) ) ;
#6759 = EDGE_CURVE ( 'NONE', #25280, #12928, #1270, .T. ) ;
#6760 = CARTESIAN_POINT ( 'NONE',  ( 10.00000000000000000, -14.67089635893658794, -73.72996012237454977 ) ) ;
#6761 = ORIENTED_EDGE ( 'NONE', *, *, #40078, .T. ) ;
#6762 = ORIENTED_EDGE ( 'NONE', *, *, #44154, .T. ) ;
#6763 = AXIS2_PLACEMENT_3D ( 'NONE', #5824, #31786, #9471 ) ;
#6764 = PLANE ( 'NONE',  #5053 ) ;
#6765 = CARTESIAN_POINT ( 'NONE',  ( 0.000000000000000000, 81.96053171279902472, -2.543863470248670211 ) ) ;
#6766 = CARTESIAN_POINT ( 'NONE',  ( 10.00000000000000000, -44.99326035066006568, -68.55367621811190304 ) ) ;
#6767 = ORIENTED_EDGE ( 'NONE', *, *, #30194, .T. ) ;
#6768 = AXIS2_PLACEMENT_3D ( 'NONE', #9087, #12289, #27211 ) ;
#6769 = CARTESIAN_POINT ( 'NONE',  ( -10.00000000000000000, 0.000000000000000000, 0.000000000000000000 ) ) ;
#6770 = ORIENTED_EDGE ( 'NONE', *, *, #36065, .F. ) ;
#6771 = VERTEX_POINT ( 'NONE', #14260 ) ;
#6772 = ORIENTED_EDGE ( 'NONE', *, *, #21922, .T. ) ;
#6773 = CARTESIAN_POINT ( 'NONE',  ( -0.1915406271734583221, -121.4877204670710427, 2.500000000000000000 ) ) ;
#6774 = FACE_OUTER_BOUND ( 'NONE', #37147, .T. ) ;
#6775 = DIRECTION ( 'NONE',  ( 0.000000000000000000, 0.9876883405951371042, 0.1564344650402346437 ) ) ;
#6776 = ORIENTED_EDGE ( 'NONE', *, *, #48236, .T. ) ;
#6777 = ORIENTED_EDGE ( 'NONE', *, *, #28846, .F. ) ;
#6778 = CIRCLE ( 'NONE', #41171, 16.00000000000000000 ) ;
#6779 = VERTEX_POINT ( 'NONE', #25745 ) ;
#6780 = LINE ( 'NONE', #47635, #30248 ) ;
#6781 = ORIENTED_EDGE ( 'NONE', *, *, #31985, .T. ) ;
#6782 = CARTESIAN_POINT ( 'NONE',  ( 0.000000000000000000, 0.000000000000000000, -40.00000000000000000 ) ) ;
#6783 = CARTESIAN_POINT ( 'NONE',  ( 5.000000000000002665, 29.01471420065564644, 76.69515212746026123 ) ) ;
#6784 = FACE_BOUND ( 'NONE', #23313, .T. ) ;
#6785 = ORIENTED_EDGE ( 'NONE', *, *, #33364, .F. ) ;
#6786 = CARTESIAN_POINT ( 'NONE',  ( 15.00000000000000000, -26.23277895567245466, 4.042438405570107918 ) ) ;
#6787 = DIRECTION ( 'NONE',  ( 0.000000000000000000, -0.8910065241883721177, 0.4539904997395382003 ) ) ;
#6788 = AXIS2_PLACEMENT_3D ( 'NONE', #34652, #15586, #26842 ) ;
#6789 = FACE_OUTER_BOUND ( 'NONE', #47645, .T. ) ;
#6790 = EDGE_CURVE ( 'NONE', #4650, #23089, #28936, .T. ) ;
#6791 = CARTESIAN_POINT ( 'NONE',  ( 0.000000000000000000, 0.000000000000000000, 0.000000000000000000 ) ) ;
#6792 = AXIS2_PLACEMENT_3D ( 'NONE', #3107, #48157, #36881 ) ;
#6793 = CARTESIAN_POINT ( 'NONE',  ( 5.999999999999999112, 21.60688246758697062, -79.10210256391344785 ) ) ;
#6794 = EDGE_CURVE ( 'NONE', #16815, #4851, #10668, .T. ) ;
#6795 = ORIENTED_EDGE ( 'NONE', *, *, #22149, .F. ) ;
#6796 = DIRECTION ( 'NONE',  ( 0.000000000000000000, -0.07845909572785234043, 0.9969173337331274087 ) ) ;
#6797 = ORIENTED_EDGE ( 'NONE', *, *, #37997, .F. ) ;
#6798 = ADVANCED_FACE ( 'NONE', ( #47071 ), #13537, .T. ) ;
#6799 = DIRECTION ( 'NONE',  ( -1.000000000000000000, -0.000000000000000000, -0.000000000000000000 ) ) ;
#6800 = DIRECTION ( 'NONE',  ( 0.000000000000000000, 0.000000000000000000, 1.000000000000000000 ) ) ;
#6801 = CARTESIAN_POINT ( 'NONE',  ( 11.99999999999999822, 31.46837873495072913, -68.27212725128242710 ) ) ;
#6802 = EDGE_CURVE ( 'NONE', #27047, #47844, #24802, .T. ) ;
#6803 = DIRECTION ( 'NONE',  ( 0.000000000000000000, 0.9876883405951383255, -0.1564344650402276216 ) ) ;
#6804 = DIRECTION ( 'NONE',  ( 0.000000000000000000, 0.000000000000000000, 1.000000000000000000 ) ) ;
#6805 = VERTEX_POINT ( 'NONE', #3724 ) ;
#6806 = FACE_OUTER_BOUND ( 'NONE', #622, .T. ) ;
#6807 = DIRECTION ( 'NONE',  ( -1.000000000000000000, -0.000000000000000000, -0.000000000000000000 ) ) ;
#6808 = AXIS2_PLACEMENT_3D ( 'NONE', #20276, #42811, #27896 ) ;
#6809 = DIRECTION ( 'NONE',  ( 0.000000000000000000, 0.3826834323650907810, -0.9238795325112864054 ) ) ;
#6810 = SURFACE_STYLE_FILL_AREA ( #40575 ) ;
#6811 = CARTESIAN_POINT ( 'NONE',  ( 0.000000000000000000, -35.53030884539077050, -12.26510123303296851 ) ) ;
#6812 = EDGE_CURVE ( 'NONE', #45107, #3188, #44599, .T. ) ;
#6813 = ADVANCED_FACE ( 'NONE', ( #14750 ), #22571, .F. ) ;
#6814 = ORIENTED_EDGE ( 'NONE', *, *, #16951, .T. ) ;
#6815 = EDGE_LOOP ( 'NONE', ( #15189, #36678 ) ) ;
#6816 = CIRCLE ( 'NONE', #47441, 77.49899999999999523 ) ;
#6817 = ORIENTED_EDGE ( 'NONE', *, *, #9013, .T. ) ;
#6818 = DIRECTION ( 'NONE',  ( 0.000000000000000000, -0.4067366430757908269, 0.9135454576426049744 ) ) ;
#6819 = LINE ( 'NONE', #3121, #14420 ) ;
#6820 = ORIENTED_EDGE ( 'NONE', *, *, #11718, .T. ) ;
#6821 = EDGE_CURVE ( 'NONE', #12203, #1459, #2074, .T. ) ;
#6822 = VECTOR ( 'NONE', #43221, 1000.000000000000114 ) ;
#6823 = CARTESIAN_POINT ( 'NONE',  ( 10.00000000000000000, 0.000000000000000000, 0.000000000000000000 ) ) ;
#6824 = ORIENTED_EDGE ( 'NONE', *, *, #15473, .T. ) ;
#6825 = ORIENTED_EDGE ( 'NONE', *, *, #40363, .F. ) ;
#6826 = VECTOR ( 'NONE', #9927, 1000.000000000000000 ) ;
#6827 = AXIS2_PLACEMENT_3D ( 'NONE', #20426, #46640, #35618 ) ;
#6828 = CARTESIAN_POINT ( 'NONE',  ( 10.00000000000000000, -15.48615015657555816, -39.04073710021360455 ) ) ;
#6829 = ORIENTED_EDGE ( 'NONE', *, *, #27531, .T. ) ;
#6830 = DIRECTION ( 'NONE',  ( 0.000000000000000000, 0.000000000000000000, 1.000000000000000000 ) ) ;
#6831 = ORIENTED_EDGE ( 'NONE', *, *, #28959, .T. ) ;
#6832 = EDGE_LOOP ( 'NONE', ( #7625, #30363, #19234, #45013 ) ) ;
#6833 = LINE ( 'NONE', #2424, #2497 ) ;
#6834 = CIRCLE ( 'NONE', #15436, 31.99999999999998224 ) ;
#6835 = CYLINDRICAL_SURFACE ( 'NONE', #43276, 16.00000000000000000 ) ;
#6836 = DIRECTION ( 'NONE',  ( 0.000000000000000000, 0.000000000000000000, 1.000000000000000000 ) ) ;
#6837 = ORIENTED_EDGE ( 'NONE', *, *, #46106, .F. ) ;
#6838 = VERTEX_POINT ( 'NONE', #38226 ) ;
#6839 = DIRECTION ( 'NONE',  ( -0.000000000000000000, -0.000000000000000000, -1.000000000000000000 ) ) ;
#6840 = PLANE ( 'NONE',  #4005 ) ;
#6841 = EDGE_CURVE ( 'NONE', #24524, #25578, #48272, .T. ) ;
#6842 = CIRCLE ( 'NONE', #45914, 31.99999999999998934 ) ;
#6843 = VERTEX_POINT ( 'NONE', #44839 ) ;
#6844 = ORIENTED_EDGE ( 'NONE', *, *, #5654, .F. ) ;
#6845 = DIRECTION ( 'NONE',  ( -1.000000000000000000, -0.000000000000000000, -0.000000000000000000 ) ) ;
#6846 = DIRECTION ( 'NONE',  ( 0.000000000000000000, -0.9238795325112906243, 0.3826834323650805114 ) ) ;
#6847 = ORIENTED_EDGE ( 'NONE', *, *, #30448, .T. ) ;
#6848 = ORIENTED_EDGE ( 'NONE', *, *, #46487, .F. ) ;
#6849 = ADVANCED_FACE ( 'NONE', ( #41417, #23052 ), #26978, .F. ) ;
#6850 = DIRECTION ( 'NONE',  ( 0.000000000000000000, -0.6494480483301738882, -0.7604059656000392575 ) ) ;
#6851 = CARTESIAN_POINT ( 'NONE',  ( -3.000000000000000000, 9.615535125379096826, -24.73947219025905042 ) ) ;
#6852 = CARTESIAN_POINT ( 'NONE',  ( 11.99999999999999822, -31.46837873494930093, -68.27212725128309501 ) ) ;
#6853 = CARTESIAN_POINT ( 'NONE',  ( 2.500000000000000000, 16.00000000000000000, -10.00000000000000178 ) ) ;
#6854 = EDGE_CURVE ( 'NONE', #24231, #27585, #7403, .T. ) ;
#6855 = CIRCLE ( 'NONE', #43578, 31.99999999999999289 ) ;
#6856 = CARTESIAN_POINT ( 'NONE',  ( 10.00000000000000000, -15.48615015657610883, 39.04073710021339139 ) ) ;
#6857 = ORIENTED_EDGE ( 'NONE', *, *, #4823, .T. ) ;
#6858 = DIRECTION ( 'NONE',  ( 0.4279312458752991266, 0.9038112904824847638, 0.000000000000000000 ) ) ;
#6859 = DIRECTION ( 'NONE',  ( 0.000000000000000000, -0.8910065241883722287, 0.4539904997395383668 ) ) ;
#6860 = CARTESIAN_POINT ( 'NONE',  ( 10.00000000000000000, 51.29473840253317718, -63.97538442413367932 ) ) ;
#6861 = DIRECTION ( 'NONE',  ( -1.000000000000000000, -0.000000000000000000, -0.000000000000000000 ) ) ;
#6862 = DIRECTION ( 'NONE',  ( 0.000000000000000000, 0.000000000000000000, 1.000000000000000000 ) ) ;
#6863 = VERTEX_POINT ( 'NONE', #11328 ) ;
#6864 = VERTEX_POINT ( 'NONE', #34293 ) ;
#6865 = EDGE_CURVE ( 'NONE', #6291, #17248, #19367, .T. ) ;
#6866 = EDGE_CURVE ( 'NONE', #2845, #39728, #30170, .T. ) ;
#6867 = ORIENTED_EDGE ( 'NONE', *, *, #861, .F. ) ;
#6868 = AXIS2_PLACEMENT_3D ( 'NONE', #1783, #5228, #17176 ) ;
#6869 = ADVANCED_FACE ( 'NONE', ( #11565 ), #7872, .T. ) ;
#6870 = DIRECTION ( 'NONE',  ( 0.000000000000000000, -0.9945218953682745111, 0.1045284632676429237 ) ) ;
#6871 = AXIS2_PLACEMENT_3D ( 'NONE', #9205, #5303, #24139 ) ;
#6872 = DIRECTION ( 'NONE',  ( -0.000000000000000000, -0.000000000000000000, 1.000000000000000000 ) ) ;
#6873 = AXIS2_PLACEMENT_3D ( 'NONE', #34154, #11645, #41508 ) ;
#6874 = ORIENTED_EDGE ( 'NONE', *, *, #17431, .F. ) ;
#6875 = EDGE_CURVE ( 'NONE', #46585, #32891, #37498, .T. ) ;
#6876 = ORIENTED_EDGE ( 'NONE', *, *, #19794, .T. ) ;
#6877 = CARTESIAN_POINT ( 'NONE',  ( 0.000000000000000000, 12.24744871391588852, 2.500000000000003553 ) ) ;
#6878 = VERTEX_POINT ( 'NONE', #41651 ) ;
#6879 = FACE_OUTER_BOUND ( 'NONE', #17165, .T. ) ;
#6880 = ORIENTED_EDGE ( 'NONE', *, *, #26930, .T. ) ;
#6881 = CIRCLE ( 'NONE', #24086, 31.99999999999998579 ) ;
#6882 = DIRECTION ( 'NONE',  ( 1.000000000000000000, -0.000000000000000000, -0.000000000000000000 ) ) ;
#6883 = CARTESIAN_POINT ( 'NONE',  ( 5.999999999999999112, 77.16300072079698680, -27.74655509720591340 ) ) ;
#6884 = VERTEX_POINT ( 'NONE', #22808 ) ;
#6885 = CARTESIAN_POINT ( 'NONE',  ( 11.99999999999999822, -2.956366410621191765, 75.11725578898467859 ) ) ;
#6886 = ORIENTED_EDGE ( 'NONE', *, *, #32944, .T. ) ;
#6887 = CARTESIAN_POINT ( 'NONE',  ( 0.000000000000000000, -120.0000000000000000, 2.500000000000000000 ) ) ;
#6888 = CARTESIAN_POINT ( 'NONE',  ( 10.05638427806949586, -98.76043467366159234, -2.500000000000000000 ) ) ;
#6889 = ORIENTED_EDGE ( 'NONE', *, *, #31782, .F. ) ;
#6890 = DIRECTION ( 'NONE',  ( 0.8541291221503261033, -0.5200609990133016058, 0.000000000000000000 ) ) ;
#6891 = CARTESIAN_POINT ( 'NONE',  ( 0.000000000000000000, 0.000000000000000000, 0.000000000000000000 ) ) ;
#6893 = ORIENTED_EDGE ( 'NONE', *, *, #756, .F. ) ;
#6892 = DIRECTION ( 'NONE',  ( 0.000000000000000000, -8.881784197001252323E-16, -1.000000000000000000 ) ) ;
#6894 = CARTESIAN_POINT ( 'NONE',  ( 10.00000000000000000, 0.000000000000000000, 0.000000000000000000 ) ) ;
#6895 = EDGE_LOOP ( 'NONE', ( #203, #25516, #11574, #39938 ) ) ;
#6896 = CYLINDRICAL_SURFACE ( 'NONE', #42826, 37.49900000000000233 ) ;
#6897 = EDGE_LOOP ( 'NONE', ( #31361, #2847, #13043, #22659 ) ) ;
#6898 = ORIENTED_EDGE ( 'NONE', *, *, #25907, .F. ) ;
#6899 = CARTESIAN_POINT ( 'NONE',  ( 10.00000000000000000, -26.79245525562738095, 32.34446384429961796 ) ) ;
#6900 = DIRECTION ( 'NONE',  ( -1.000000000000000000, 0.000000000000000000, 0.000000000000000000 ) ) ;
#6901 = ORIENTED_EDGE ( 'NONE', *, *, #14370, .F. ) ;
#6902 = ADVANCED_FACE ( 'NONE', ( #15472 ), #29665, .T. ) ;
#6903 = DIRECTION ( 'NONE',  ( 0.000000000000000000, 0.000000000000000000, 1.000000000000000000 ) ) ;
#6904 = DIRECTION ( 'NONE',  ( 0.9918136447140100120, -0.1276937514489704939, 0.000000000000000000 ) ) ;
#6905 = DIRECTION ( 'NONE',  ( 0.000000000000000000, -0.9510565162951506446, -0.3090169943749562775 ) ) ;
#6906 = EDGE_LOOP ( 'NONE', ( #31444, #42845, #4249, #15924 ) ) ;
#6907 = ADVANCED_FACE ( 'NONE', ( #37258 ), #41190, .F. ) ;
#6908 = DIRECTION ( 'NONE',  ( 1.000000000000000000, 0.000000000000000000, 0.000000000000000000 ) ) ;
#6909 = ADVANCED_FACE ( 'NONE', ( #18649 ), #26727, .T. ) ;
#6910 = CARTESIAN_POINT ( 'NONE',  ( 0.000000000000000000, -120.0000000000000000, -125.0000000000000000 ) ) ;
#6911 = DIRECTION ( 'NONE',  ( -1.000000000000000000, 0.000000000000000000, 0.000000000000000000 ) ) ;
#6912 = ORIENTED_EDGE ( 'NONE', *, *, #37923, .F. ) ;
#6913 = EDGE_CURVE ( 'NONE', #20902, #8878, #22339, .T. ) ;
#6914 = CARTESIAN_POINT ( 'NONE',  ( 0.000000000000000000, -80.55351364060599906, 15.33399622253457295 ) ) ;
#6916 = EDGE_CURVE ( 'NONE', #8858, #11527, #11450, .T. ) ;
#6915 = LINE ( 'NONE', #17434, #41098 ) ;
#6917 = CARTESIAN_POINT ( 'NONE',  ( 0.000000000000000000, 0.000000000000000000, 0.000000000000000000 ) ) ;
#6918 = DIRECTION ( 'NONE',  ( 1.000000000000000000, 1.390371824233641368E-16, 0.000000000000000000 ) ) ;
#6919 = ORIENTED_EDGE ( 'NONE', *, *, #19584, .T. ) ;
#6920 = FACE_OUTER_BOUND ( 'NONE', #7118, .T. ) ;
#6921 = DIRECTION ( 'NONE',  ( -1.000000000000000000, -0.000000000000000000, 0.000000000000000000 ) ) ;
#6922 = AXIS2_PLACEMENT_3D ( 'NONE', #5070, #5545, #35392 ) ;
#6923 = LINE ( 'NONE', #29441, #17033 ) ;
#6924 = CARTESIAN_POINT ( 'NONE',  ( 0.000000000000000000, 59.46389618802034960, -49.70050353004825894 ) ) ;
#6925 = AXIS2_PLACEMENT_3D ( 'NONE', #29189, #7159, #14999 ) ;
#6926 = ORIENTED_EDGE ( 'NONE', *, *, #13097, .T. ) ;
#6927 = LINE ( 'NONE', #3236, #37079 ) ;
#6928 = ORIENTED_EDGE ( 'NONE', *, *, #21744, .F. ) ;
#6929 = EDGE_CURVE ( 'NONE', #23939, #27284, #27872, .T. ) ;
#6930 = DIRECTION ( 'NONE',  ( 0.000000000000000000, -0.7604059656000228262, -0.6494480483301932061 ) ) ;
#6931 = DIRECTION ( 'NONE',  ( 0.000000000000000000, 0.000000000000000000, 1.000000000000000000 ) ) ;
#6932 = CARTESIAN_POINT ( 'NONE',  ( -11.70000000000000107, 0.000000000000000000, -20.69999999999999929 ) ) ;
#6933 = ORIENTED_EDGE ( 'NONE', *, *, #24605, .F. ) ;
#6934 = EDGE_CURVE ( 'NONE', #14862, #5941, #38959, .T. ) ;
#6935 = CARTESIAN_POINT ( 'NONE',  ( 1.250000000000000444, -16.78109714094927085, -1.199999999999999956 ) ) ;
#6936 = VECTOR ( 'NONE', #29078, 1000.000000000000000 ) ;
#6937 = ORIENTED_EDGE ( 'NONE', *, *, #32346, .F. ) ;
#6938 = ORIENTED_EDGE ( 'NONE', *, *, #14821, .F. ) ;
#6939 = VECTOR ( 'NONE', #24342, 1000.000000000000000 ) ;
#6940 = EDGE_CURVE ( 'NONE', #26295, #45334, #9550, .T. ) ;
#6941 = CARTESIAN_POINT ( 'NONE',  ( 0.000000000000000000, 68.26794271651307611, -31.47745569255064169 ) ) ;
#6942 = ORIENTED_EDGE ( 'NONE', *, *, #42710, .T. ) ;
#6943 = CARTESIAN_POINT ( 'NONE',  ( 0.000000000000000000, -59.75363087400035056, -56.15606465355020305 ) ) ;
#6944 = CARTESIAN_POINT ( 'NONE',  ( 6.000000000000000000, -81.50828551894220197, -8.966570791701593990 ) ) ;
#6945 = ORIENTED_EDGE ( 'NONE', *, *, #34805, .T. ) ;
#6946 = DIRECTION ( 'NONE',  ( -1.000000000000000000, 0.000000000000000000, 0.000000000000000000 ) ) ;
#6947 = ORIENTED_EDGE ( 'NONE', *, *, #31011, .T. ) ;
#6948 = LINE ( 'NONE', #32427, #38181 ) ;
#6949 = FACE_OUTER_BOUND ( 'NONE', #31585, .T. ) ;
#6950 = FACE_OUTER_BOUND ( 'NONE', #38546, .T. ) ;
#6951 = EDGE_CURVE ( 'NONE', #11599, #32258, #29426, .T. ) ;
#6952 = CARTESIAN_POINT ( 'NONE',  ( 10.00000000000000000, -33.71516098798684880, -74.74816331893465815 ) ) ;
#6953 = VERTEX_POINT ( 'NONE', #12293 ) ;
#6954 = CARTESIAN_POINT ( 'NONE',  ( 11.99999999999999822, 0.000000000000000000, 0.000000000000000000 ) ) ;
#6955 = ORIENTED_EDGE ( 'NONE', *, *, #32561, .T. ) ;
#6956 = ORIENTED_EDGE ( 'NONE', *, *, #31688, .F. ) ;
#6957 = EDGE_CURVE ( 'NONE', #32773, #32651, #25498, .T. ) ;
#6958 = DIRECTION ( 'NONE',  ( 0.000000000000000000, -0.5877852522924624790, -0.8090169943749550008 ) ) ;
#6959 = DIRECTION ( 'NONE',  ( -1.000000000000000000, -0.000000000000000000, 0.000000000000000000 ) ) ;
#6960 = DIRECTION ( 'NONE',  ( 0.000000000000000000, 0.000000000000000000, 1.000000000000000000 ) ) ;
#6961 = CYLINDRICAL_SURFACE ( 'NONE', #24367, 32.00000000000000000 ) ;
#6962 = VERTEX_POINT ( 'NONE', #19843 ) ;
#6963 = EDGE_CURVE ( 'NONE', #35099, #23124, #1507, .T. ) ;
#6964 = LINE ( 'NONE', #40503, #4971 ) ;
#6965 = CARTESIAN_POINT ( 'NONE',  ( 0.000000000000000000, 50.23322058963442061, -64.81221759200289512 ) ) ;
#6966 = EDGE_CURVE ( 'NONE', #44214, #22321, #13243, .T. ) ;
#6967 = DIRECTION ( 'NONE',  ( 0.000000000000000000, 0.000000000000000000, -1.000000000000000000 ) ) ;
#6968 = CARTESIAN_POINT ( 'NONE',  ( 0.000000000000000000, 79.10210256391398786, -21.60688246758504505 ) ) ;
#6969 = CARTESIAN_POINT ( 'NONE',  ( 10.00000000000000000, -26.02418014898359289, 70.52718814184250107 ) ) ;
#6970 = ORIENTED_EDGE ( 'NONE', *, *, #48014, .F. ) ;
#6971 = VECTOR ( 'NONE', #25644, 1000.000000000000114 ) ;
#6973 = EDGE_CURVE ( 'NONE', #488, #37099, #8316, .T. ) ;
#6972 = CYLINDRICAL_SURFACE ( 'NONE', #2900, 31.99999999999998579 ) ;
#6974 = AXIS2_PLACEMENT_3D ( 'NONE', #47206, #24930, #39868 ) ;
#6975 = CARTESIAN_POINT ( 'NONE',  ( -18.12185313557660038, -104.9634299478706794, 5.500000000000000000 ) ) ;
#6976 = CARTESIAN_POINT ( 'NONE',  ( 0.000000000000000000, 17.80606268964540106, 33.00180498840052934 ) ) ;
#6977 = VECTOR ( 'NONE', #21147, 1000.000000000000114 ) ;
#6978 = FACE_OUTER_BOUND ( 'NONE', #25053, .T. ) ;
#6979 = LINE ( 'NONE', #32215, #6822 ) ;
#6980 = CARTESIAN_POINT ( 'NONE',  ( 15.00000000000000000, 20.85821328998741109, -10.92862929874522671 ) ) ;
#6981 = ORIENTED_EDGE ( 'NONE', *, *, #37282, .F. ) ;
#6982 = DIRECTION ( 'NONE',  ( -1.000000000000000000, 0.000000000000000000, -0.000000000000000000 ) ) ;
#6983 = CARTESIAN_POINT ( 'NONE',  ( 10.00000000000000000, 0.000000000000000000, 0.000000000000000000 ) ) ;
#6984 = ORIENTED_EDGE ( 'NONE', *, *, #43713, .T. ) ;
#6985 = VERTEX_POINT ( 'NONE', #16670 ) ;
#6986 =( GEOMETRIC_REPRESENTATION_CONTEXT ( 3 ) GLOBAL_UNCERTAINTY_ASSIGNED_CONTEXT ( ( #45275 ) ) GLOBAL_UNIT_ASSIGNED_CONTEXT ( ( #16379, #12963, #1945 ) ) REPRESENTATION_CONTEXT ( 'NONE', 'WORKASPACE' ) );
#6987 = ORIENTED_EDGE ( 'NONE', *, *, #19095, .T. ) ;
#6988 = EDGE_LOOP ( 'NONE', ( #6761, #5085, #36501, #43392 ) ) ;
#6989 = DIRECTION ( 'NONE',  ( 1.000000000000000000, 0.000000000000000000, -0.000000000000000000 ) ) ;
#6990 = ORIENTED_EDGE ( 'NONE', *, *, #9385, .T. ) ;
#6991 = VERTEX_POINT ( 'NONE', #34783 ) ;
#6992 = DIRECTION ( 'NONE',  ( -1.000000000000000000, 0.000000000000000000, 0.000000000000000000 ) ) ;
#6993 = CARTESIAN_POINT ( 'NONE',  ( 10.00000000000000000, -22.64427369931148348, -30.00120703465229965 ) ) ;
#6994 = CARTESIAN_POINT ( 'NONE',  ( 0.000000000000000000, 0.000000000000000000, -44.99999999999998579 ) ) ;
#6995 = ORIENTED_EDGE ( 'NONE', *, *, #5110, .T. ) ;
#6996 = CYLINDRICAL_SURFACE ( 'NONE', #25813, 82.00000000000000000 ) ;
#6997 = ORIENTED_EDGE ( 'NONE', *, *, #330, .F. ) ;
#6998 = ORIENTED_EDGE ( 'NONE', *, *, #42342, .F. ) ;
#6999 = ORIENTED_EDGE ( 'NONE', *, *, #2208, .F. ) ;
#7000 = LINE ( 'NONE', #25833, #29550 ) ;
#7001 = CARTESIAN_POINT ( 'NONE',  ( -2.981742216678212820, 0.000000000000000000, 0.000000000000000000 ) ) ;
#7002 = FACE_OUTER_BOUND ( 'NONE', #36511, .T. ) ;
#7003 = ORIENTED_EDGE ( 'NONE', *, *, #21922, .F. ) ;
#7004 = ORIENTED_EDGE ( 'NONE', *, *, #13327, .F. ) ;
#7005 = AXIS2_PLACEMENT_3D ( 'NONE', #23561, #41689, #41451 ) ;
#7006 = DIRECTION ( 'NONE',  ( 0.000000000000000000, 0.4539904997395477482, -0.8910065241883673437 ) ) ;
#7007 = ORIENTED_EDGE ( 'NONE', *, *, #21131, .T. ) ;
#7008 = EDGE_CURVE ( 'NONE', #15030, #39579, #41914, .T. ) ;
#7009 = CARTESIAN_POINT ( 'NONE',  ( 11.99999999999999822, 51.02545421589324803, 55.20638768913779870 ) ) ;
#7010 = DIRECTION ( 'NONE',  ( 0.000000000000000000, 0.000000000000000000, -1.000000000000000000 ) ) ;
#7011 = LINE ( 'NONE', #28578, #27624 ) ;
#7012 = DIRECTION ( 'NONE',  ( -1.000000000000000000, 0.000000000000000000, 0.000000000000000000 ) ) ;
#7013 = EDGE_CURVE ( 'NONE', #29636, #12206, #33292, .T. ) ;
#7014 = CYLINDRICAL_SURFACE ( 'NONE', #41694, 77.49899999999999523 ) ;
#7015 = FACE_OUTER_BOUND ( 'NONE', #38426, .T. ) ;
#7017 = EDGE_CURVE ( 'NONE', #16188, #10009, #45823, .T. ) ;
#7016 = DIRECTION ( 'NONE',  ( 0.9827303690289279636, 0.1850432970638681840, 0.000000000000000000 ) ) ;
#7018 = CARTESIAN_POINT ( 'NONE',  ( 10.00000000000000000, 17.80606268964585226, -33.00180498840028775 ) ) ;
#7019 = ORIENTED_EDGE ( 'NONE', *, *, #28946, .F. ) ;
#7021 = EDGE_CURVE ( 'NONE', #5172, #32098, #18484, .T. ) ;
#7020 = CARTESIAN_POINT ( 'NONE',  ( 10.00000000000000000, 74.65374052328648702, 8.840884882375350529 ) ) ;
#7022 = DIRECTION ( 'NONE',  ( -1.000000000000000000, 0.000000000000000000, -0.000000000000000000 ) ) ;
#7023 = ADVANCED_FACE ( 'NONE', ( #42377 ), #8831, .T. ) ;
#7024 = VERTEX_POINT ( 'NONE', #13015 ) ;
#7025 = LINE ( 'NONE', #21952, #30614 ) ;
#7026 = CARTESIAN_POINT ( 'NONE',  ( 10.00000000000000000, 77.19088730480534366, -6.903761155836915187 ) ) ;
#7027 = CYLINDRICAL_SURFACE ( 'NONE', #20049, 16.00000000000000000 ) ;
#7028 = DIRECTION ( 'NONE',  ( 0.000000000000000000, 0.000000000000000000, 1.000000000000000000 ) ) ;
#7029 = VECTOR ( 'NONE', #28650, 1000.000000000000000 ) ;
#7030 = DIRECTION ( 'NONE',  ( -1.000000000000000000, 0.000000000000000000, 0.000000000000000000 ) ) ;
#7031 = DIRECTION ( 'NONE',  ( 0.000000000000000000, 0.000000000000000000, 1.000000000000000000 ) ) ;
#7032 = ORIENTED_EDGE ( 'NONE', *, *, #37094, .T. ) ;
#7033 = AXIS2_PLACEMENT_3D ( 'NONE', #19328, #41144, #45779 ) ;
#7034 = CARTESIAN_POINT ( 'NONE',  ( 6.000000000000000000, -78.73519480814938731, -22.90783923731713045 ) ) ;
#7035 = SURFACE_SIDE_STYLE ('',( #6810 ) ) ;
#7036 = DIRECTION ( 'NONE',  ( 0.000000000000000000, -0.7071067811865536790, 0.7071067811865413555 ) ) ;
#7037 = ORIENTED_EDGE ( 'NONE', *, *, #14144, .T. ) ;
#7038 = ORIENTED_EDGE ( 'NONE', *, *, #31030, .T. ) ;
#7039 = AXIS2_PLACEMENT_3D ( 'NONE', #46581, #13051, #27982 ) ;
#7040 = ORIENTED_EDGE ( 'NONE', *, *, #36407, .F. ) ;
#7041 = LINE ( 'NONE', #9997, #3827 ) ;
#7042 = CARTESIAN_POINT ( 'NONE',  ( 11.99999999999999822, -3.894527615417340272, -81.90746397400391743 ) ) ;
#7043 = ORIENTED_EDGE ( 'NONE', *, *, #30915, .T. ) ;
#7044 = ORIENTED_EDGE ( 'NONE', *, *, #30562, .T. ) ;
#7045 = EDGE_CURVE ( 'NONE', #17031, #45751, #39435, .T. ) ;
#7046 = CARTESIAN_POINT ( 'NONE',  ( 48.80839716909466830, -10.37454508288725208, -5.500000000000000000 ) ) ;
#7047 = ADVANCED_FACE ( 'NONE', ( #24025 ), #19592, .T. ) ;
#7048 = ORIENTED_EDGE ( 'NONE', *, *, #16774, .T. ) ;
#7049 = ORIENTED_EDGE ( 'NONE', *, *, #21877, .T. ) ;
#7050 = EDGE_CURVE ( 'NONE', #7278, #44570, #46291, .T. ) ;
#7051 = AXIS2_PLACEMENT_3D ( 'NONE', #15552, #45404, #11884 ) ;
#7052 = DIRECTION ( 'NONE',  ( 0.000000000000000000, -0.9781476007338040235, -0.2079116908177671419 ) ) ;
#7054 = VERTEX_POINT ( 'NONE', #45819 ) ;
#7053 = CIRCLE ( 'NONE', #34411, 31.99999999999998934 ) ;
#7055 = LINE ( 'NONE', #33969, #23117 ) ;
#7056 = ORIENTED_EDGE ( 'NONE', *, *, #46680, .F. ) ;
#7057 = LINE ( 'NONE', #32298, #12682 ) ;
#7058 = AXIS2_PLACEMENT_3D ( 'NONE', #35623, #31480, #17011 ) ;
#7059 = CIRCLE ( 'NONE', #1591, 31.99999999999999289 ) ;
#7060 = DIRECTION ( 'NONE',  ( 0.000000000000000000, 0.9969173337331276308, 0.07845909572784864894 ) ) ;
#7061 = ADVANCED_FACE ( 'NONE', ( #42138 ), #1269, .T. ) ;
#7062 = DIRECTION ( 'NONE',  ( 0.000000000000000000, 0.000000000000000000, 1.000000000000000000 ) ) ;
#7063 = VERTEX_POINT ( 'NONE', #32091 ) ;
#7064 = AXIS2_PLACEMENT_3D ( 'NONE', #38942, #5640, #46523 ) ;
#7065 = ADVANCED_FACE ( 'NONE', ( #32785 ), #2685, .T. ) ;
#7066 = EDGE_CURVE ( 'NONE', #23020, #10873, #39610, .T. ) ;
#7067 = ORIENTED_EDGE ( 'NONE', *, *, #9430, .F. ) ;
#7068 = AXIS2_PLACEMENT_3D ( 'NONE', #15693, #44350, #10823 ) ;
#7069 = CARTESIAN_POINT ( 'NONE',  ( 0.000000000000000000, -18.13022148937263012, 15.02647892043544608 ) ) ;
#7070 = DIRECTION ( 'NONE',  ( 0.000000000000000000, 0.000000000000000000, 1.000000000000000000 ) ) ;
#7071 = ORIENTED_EDGE ( 'NONE', *, *, #40549, .T. ) ;
#7072 = VECTOR ( 'NONE', #39419, 1000.000000000000000 ) ;
#7073 = VERTEX_POINT ( 'NONE', #13475 ) ;
#7074 = FACE_OUTER_BOUND ( 'NONE', #45705, .T. ) ;
#7075 = DIRECTION ( 'NONE',  ( -0.2079116908177431888, 1.197885328332322634E-16, -0.9781476007338091305 ) ) ;
#7076 = EDGE_LOOP ( 'NONE', ( #32430, #31340, #43338, #11702 ) ) ;
#7077 = ORIENTED_EDGE ( 'NONE', *, *, #30409, .T. ) ;
#7078 = CARTESIAN_POINT ( 'NONE',  ( 10.00000000000000000, 50.95692526931414790, -58.39081064771693974 ) ) ;
#7079 = CYLINDRICAL_SURFACE ( 'NONE', #39199, 31.99999999999998579 ) ;
#7080 = CARTESIAN_POINT ( 'NONE',  ( 11.99999999999999822, -46.21855187248673502, 62.20884554314003623 ) ) ;
#7081 = DIRECTION ( 'NONE',  ( -1.000000000000000000, 0.000000000000000000, 0.000000000000000000 ) ) ;
#7082 = CYLINDRICAL_SURFACE ( 'NONE', #13299, 31.99999999999999289 ) ;
#7083 = EDGE_CURVE ( 'NONE', #1594, #34027, #19939, .T. ) ;
#7084 = DIRECTION ( 'NONE',  ( 1.000000000000000000, 0.000000000000000000, 0.000000000000000000 ) ) ;
#7085 = CARTESIAN_POINT ( 'NONE',  ( 11.99999999999999822, -62.50329211542407393, -41.76937507738853839 ) ) ;
#7086 = CARTESIAN_POINT ( 'NONE',  ( -11.99999999999999645, 13.90444123027096879, 0.000000000000000000 ) ) ;
#7087 = ORIENTED_EDGE ( 'NONE', *, *, #41445, .T. ) ;
#7088 = FACE_OUTER_BOUND ( 'NONE', #44344, .T. ) ;
#7089 = CARTESIAN_POINT ( 'NONE',  ( 0.000000000000000000, 55.16347631943042984, 60.67117009219157353 ) ) ;
#7090 = SURFACE_STYLE_FILL_AREA ( #40626 ) ;
#7091 = DIRECTION ( 'NONE',  ( -1.000000000000000000, -0.000000000000000000, 0.000000000000000000 ) ) ;
#7092 = EDGE_LOOP ( 'NONE', ( #35154, #29854, #1146, #37376 ) ) ;
#7093 = VERTEX_POINT ( 'NONE', #6614 ) ;
#7094 = ORIENTED_EDGE ( 'NONE', *, *, #28534, .F. ) ;
#7095 = VECTOR ( 'NONE', #6433, 1000.000000000000114 ) ;
#7096 = UNCERTAINTY_MEASURE_WITH_UNIT (LENGTH_MEASURE( 1.000000000000000082E-05 ), #1273, 'distance_accuracy_value', 'NONE');
#7097 = FACE_OUTER_BOUND ( 'NONE', #39935, .T. ) ;
#7098 = CIRCLE ( 'NONE', #30548, 15.99999999999999645 ) ;
#7099 = AXIS2_PLACEMENT_3D ( 'NONE', #10248, #32533, #17113 ) ;
#7100 = DIRECTION ( 'NONE',  ( 0.000000000000000000, 0.000000000000000000, 1.000000000000000000 ) ) ;
#7101 = ORIENTED_EDGE ( 'NONE', *, *, #32614, .T. ) ;
#7102 = CIRCLE ( 'NONE', #34451, 31.99999999999999645 ) ;
#7103 = AXIS2_PLACEMENT_3D ( 'NONE', #44767, #7576, #18810 ) ;
#7104 = EDGE_LOOP ( 'NONE', ( #3521, #24258, #10065, #1452 ) ) ;
#7105 = EDGE_CURVE ( 'NONE', #5392, #35187, #17373, .T. ) ;
#7106 = VECTOR ( 'NONE', #926, 1000.000000000000000 ) ;
#7107 = CARTESIAN_POINT ( 'NONE',  ( -11.59517495878806947, -96.12423995607481686, 5.500000000000000000 ) ) ;
#7108 = ORIENTED_EDGE ( 'NONE', *, *, #7948, .F. ) ;
#7109 = DIRECTION ( 'NONE',  ( 0.000000000000000000, 0.000000000000000000, 1.000000000000000000 ) ) ;
#7110 = ORIENTED_EDGE ( 'NONE', *, *, #21215, .F. ) ;
#7111 = ADVANCED_FACE ( 'NONE', ( #21546 ), #44055, .T. ) ;
#7112 = ORIENTED_EDGE ( 'NONE', *, *, #41308, .T. ) ;
#7113 = VERTEX_POINT ( 'NONE', #32565 ) ;
#7114 = CARTESIAN_POINT ( 'NONE',  ( -10.00000000000000000, 0.000000000000000000, 0.000000000000000000 ) ) ;
#7115 = EDGE_CURVE ( 'NONE', #43867, #32554, #5884, .T. ) ;
#7116 = CARTESIAN_POINT ( 'NONE',  ( 10.00000000000000000, -81.50828551894232987, 8.966570791700396725 ) ) ;
#7117 = VERTEX_POINT ( 'NONE', #24965 ) ;
#7118 = EDGE_LOOP ( 'NONE', ( #18750, #14117, #36140, #18395 ) ) ;
#7119 = ORIENTED_EDGE ( 'NONE', *, *, #24254, .T. ) ;
#7120 = CARTESIAN_POINT ( 'NONE',  ( 11.99999999999999822, -28.89263327155796190, 71.91182617369179297 ) ) ;
#7121 = ORIENTED_EDGE ( 'NONE', *, *, #37222, .T. ) ;
#7122 = CARTESIAN_POINT ( 'NONE',  ( 0.000000000000000000, -5.202137450156129717, -37.22597642581163768 ) ) ;
#7123 = DIRECTION ( 'NONE',  ( 0.000000000000000000, 0.000000000000000000, 1.000000000000000000 ) ) ;
#7124 = VERTEX_POINT ( 'NONE', #40397 ) ;
#7125 = EDGE_CURVE ( 'NONE', #42528, #38227, #47011, .T. ) ;
#7126 = DIRECTION ( 'NONE',  ( 0.000000000000000000, 0.9510565162951503115, 0.3090169943749573878 ) ) ;
#7127 = CARTESIAN_POINT ( 'NONE',  ( 0.000000000000000000, -21.40280677340345505, -36.13751322684441192 ) ) ;
#7128 = ADVANCED_FACE ( 'NONE', ( #6138 ), #40156, .F. ) ;
#7129 = AXIS2_PLACEMENT_3D ( 'NONE', #18143, #19125, #33087 ) ;
#7131 = ORIENTED_EDGE ( 'NONE', *, *, #44262, .T. ) ;
#7130 = DIRECTION ( 'NONE',  ( -1.000000000000000000, 0.000000000000000000, 0.000000000000000000 ) ) ;
#7132 = CARTESIAN_POINT ( 'NONE',  ( 11.99999999999999822, -20.41045688087876897, 72.35160999960810102 ) ) ;
#7133 = VERTEX_POINT ( 'NONE', #14445 ) ;
#7134 = VECTOR ( 'NONE', #10138, 1000.000000000000000 ) ;
#7135 = PLANE ( 'NONE',  #17794 ) ;
#7136 = VERTEX_POINT ( 'NONE', #25677 ) ;
#7137 = VERTEX_POINT ( 'NONE', #28656 ) ;
#7138 = LINE ( 'NONE', #22322, #9567 ) ;
#7139 = CARTESIAN_POINT ( 'NONE',  ( 10.00000000000000000, 0.000000000000000000, 0.000000000000000000 ) ) ;
#7140 = CIRCLE ( 'NONE', #15733, 82.00000000000000000 ) ;
#7141 = ORIENTED_EDGE ( 'NONE', *, *, #30710, .F. ) ;
#7142 = CIRCLE ( 'NONE', #22752, 16.00000000000000355 ) ;
#7143 = LINE ( 'NONE', #14738, #2644 ) ;
#7144 = CARTESIAN_POINT ( 'NONE',  ( 10.00000000000000000, 0.000000000000000000, 0.000000000000000000 ) ) ;
#7145 = LINE ( 'NONE', #33337, #19812 ) ;
#7146 = VERTEX_POINT ( 'NONE', #17858 ) ;
#7147 = DIRECTION ( 'NONE',  ( 0.000000000000000000, 0.000000000000000000, 1.000000000000000000 ) ) ;
#7148 = AXIS2_PLACEMENT_3D ( 'NONE', #37660, #7796, #36916 ) ;
#7149 = DIRECTION ( 'NONE',  ( -1.000000000000000000, 0.000000000000000000, -0.000000000000000000 ) ) ;
#7150 = EDGE_CURVE ( 'NONE', #11148, #16517, #45749, .T. ) ;
#7151 = DIRECTION ( 'NONE',  ( 0.000000000000000000, 0.000000000000000000, 1.000000000000000000 ) ) ;
#7152 = DIRECTION ( 'NONE',  ( -1.000000000000000000, 0.000000000000000000, -0.000000000000000000 ) ) ;
#7153 = CARTESIAN_POINT ( 'NONE',  ( 12.00000000000000000, -18.13022148937263012, -15.02647892043543898 ) ) ;
#7154 = CARTESIAN_POINT ( 'NONE',  ( 5.999999999999999112, -60.67117009219175827, 55.16347631943019536 ) ) ;
#7155 = DIRECTION ( 'NONE',  ( 0.000000000000000000, 0.000000000000000000, 1.000000000000000000 ) ) ;
#7156 = CARTESIAN_POINT ( 'NONE',  ( -18.24502636017238899, -100.7225776329765665, 5.500000000000000000 ) ) ;
#7157 = CARTESIAN_POINT ( 'NONE',  ( 10.00000000000000000, 0.000000000000000000, 0.000000000000000000 ) ) ;
#7158 = CARTESIAN_POINT ( 'NONE',  ( 0.000000000000000000, -120.0000000000000000, 125.0000000000000000 ) ) ;
#7159 = DIRECTION ( 'NONE',  ( 0.000000000000000000, 0.000000000000000000, 1.000000000000000000 ) ) ;
#7160 = ORIENTED_EDGE ( 'NONE', *, *, #38812, .T. ) ;
#7161 = EDGE_LOOP ( 'NONE', ( #9463, #21699, #20437, #45412 ) ) ;
#7162 = LINE ( 'NONE', #25998, #48007 ) ;
#7163 = VERTEX_POINT ( 'NONE', #2219 ) ;
#7164 = CARTESIAN_POINT ( 'NONE',  ( 11.99999999999999822, 0.000000000000000000, 0.000000000000000000 ) ) ;
#7165 = DIRECTION ( 'NONE',  ( -0.7533909544171997208, -0.6575728627325955200, 0.000000000000000000 ) ) ;
#7166 = DIRECTION ( 'NONE',  ( 0.000000000000000000, 0.8660254037844363761, -0.5000000000000039968 ) ) ;
#7167 = VERTEX_POINT ( 'NONE', #47707 ) ;
#7168 = AXIS2_PLACEMENT_3D ( 'NONE', #25624, #13900, #1739 ) ;
#7169 = CIRCLE ( 'NONE', #26709, 82.00000000000000000 ) ;
#7170 = CIRCLE ( 'NONE', #32209, 82.00000000000000000 ) ;
#7171 = DIRECTION ( 'NONE',  ( -1.000000000000000000, -0.000000000000000000, 0.000000000000000000 ) ) ;
#7172 = ADVANCED_FACE ( 'NONE', ( #25196 ), #28877, .T. ) ;
#7173 = VERTEX_POINT ( 'NONE', #43348 ) ;
#7174 = EDGE_CURVE ( 'NONE', #17338, #15509, #26995, .T. ) ;
#7175 = CIRCLE ( 'NONE', #32959, 31.99999999999998579 ) ;
#7176 = DIRECTION ( 'NONE',  ( -1.000000000000000000, -0.000000000000000000, 0.000000000000000000 ) ) ;
#7177 = EDGE_CURVE ( 'NONE', #24526, #43853, #23099, .T. ) ;
#7178 = CARTESIAN_POINT ( 'NONE',  ( 0.000000000000000000, 0.000000000000000000, 0.000000000000000000 ) ) ;
#7179 = CARTESIAN_POINT ( 'NONE',  ( 11.99999999999999822, -8.840884882374576037, -74.65374052328658649 ) ) ;
#7180 = CIRCLE ( 'NONE', #15020, 31.99999999999999289 ) ;
#7181 = ORIENTED_EDGE ( 'NONE', *, *, #19829, .F. ) ;
#7182 = DIRECTION ( 'NONE',  ( 0.000000000000000000, 0.000000000000000000, -1.000000000000000000 ) ) ;
#7183 = EDGE_LOOP ( 'NONE', ( #24703, #4319, #33246, #34425 ) ) ;
#7184 = LINE ( 'NONE', #570, #10491 ) ;
#7185 = CARTESIAN_POINT ( 'NONE',  ( 10.00000000000000000, 0.000000000000000000, 0.000000000000000000 ) ) ;
#7186 = EDGE_CURVE ( 'NONE', #45284, #36506, #44299, .T. ) ;
#7187 = CARTESIAN_POINT ( 'NONE',  ( 11.99999999999999822, 62.20884554314085335, -46.21855187248562657 ) ) ;
#7188 = CYLINDRICAL_SURFACE ( 'NONE', #42158, 31.99999999999998579 ) ;
#7189 = ORIENTED_EDGE ( 'NONE', *, *, #25102, .T. ) ;
#7190 = CARTESIAN_POINT ( 'NONE',  ( 10.00000000000000000, 0.000000000000000000, 0.000000000000000000 ) ) ;
#7191 = ORIENTED_EDGE ( 'NONE', *, *, #16873, .F. ) ;
#7192 = ORIENTED_EDGE ( 'NONE', *, *, #27115, .T. ) ;
#7193 = EDGE_CURVE ( 'NONE', #1357, #17758, #43581, .T. ) ;
#7194 = DIRECTION ( 'NONE',  ( -1.000000000000000000, -0.000000000000000000, 0.000000000000000000 ) ) ;
#7195 = FACE_OUTER_BOUND ( 'NONE', #44814, .T. ) ;
#7196 = CARTESIAN_POINT ( 'NONE',  ( -3.000000000000000000, -19.89357724624987256, -12.59942793731086041 ) ) ;
#7197 = CYLINDRICAL_SURFACE ( 'NONE', #36762, 12.49999999999999822 ) ;
#7198 = ORIENTED_EDGE ( 'NONE', *, *, #8538, .F. ) ;
#7199 = DIRECTION ( 'NONE',  ( 0.000000000000000000, 0.000000000000000000, 1.000000000000000000 ) ) ;
#7200 = DIRECTION ( 'NONE',  ( -1.000000000000000000, 0.000000000000000000, 0.000000000000000000 ) ) ;
#7201 = DIRECTION ( 'NONE',  ( 1.000000000000000000, -0.000000000000000000, 0.000000000000000000 ) ) ;
#7202 = AXIS2_PLACEMENT_3D ( 'NONE', #47382, #40279, #3050 ) ;
#7203 = DIRECTION ( 'NONE',  ( -0.1850432970638667129, 0.9827303690289281857, 0.000000000000000000 ) ) ;
#7204 = EDGE_CURVE ( 'NONE', #19747, #29191, #37437, .T. ) ;
#7205 = DIRECTION ( 'NONE',  ( -1.000000000000000000, 0.000000000000000000, 0.000000000000000000 ) ) ;
#7206 = CARTESIAN_POINT ( 'NONE',  ( 1.250000000000000444, -16.78109714094927085, -1.199999999999999956 ) ) ;
#7207 = CARTESIAN_POINT ( 'NONE',  ( -35.50000000000000711, -120.0000000000000000, 2.500000000000000000 ) ) ;
#7208 = CARTESIAN_POINT ( 'NONE',  ( 0.000000000000000000, 0.000000000000000000, 0.000000000000000000 ) ) ;
#7209 = AXIS2_PLACEMENT_3D ( 'NONE', #46761, #5162, #42112 ) ;
#7210 = LINE ( 'NONE', #26780, #2512 ) ;
#7211 = CARTESIAN_POINT ( 'NONE',  ( 4.999999999999999112, 36.13751322684449008, -21.40280677340332716 ) ) ;
#7212 = VECTOR ( 'NONE', #20692, 1000.000000000000000 ) ;
#7213 = ORIENTED_EDGE ( 'NONE', *, *, #21667, .F. ) ;
#7214 = PLANE ( 'NONE',  #5965 ) ;
#7215 = EDGE_CURVE ( 'NONE', #33303, #7570, #424, .T. ) ;
#7216 = DIRECTION ( 'NONE',  ( 0.000000000000000000, 0.000000000000000000, 1.000000000000000000 ) ) ;
#7217 = CYLINDRICAL_SURFACE ( 'NONE', #31622, 77.49899999999999523 ) ;
#7218 = CYLINDRICAL_SURFACE ( 'NONE', #45039, 31.99999999999998579 ) ;
#7219 = LINE ( 'NONE', #22404, #15264 ) ;
#7220 = AXIS2_PLACEMENT_3D ( 'NONE', #6983, #40524, #25810 ) ;
#7221 = DIRECTION ( 'NONE',  ( -1.000000000000000000, 0.000000000000000000, 0.000000000000000000 ) ) ;
#7222 = ORIENTED_EDGE ( 'NONE', *, *, #12178, .T. ) ;
#7223 = ORIENTED_EDGE ( 'NONE', *, *, #33533, .T. ) ;
#7224 = EDGE_CURVE ( 'NONE', #33522, #44222, #40299, .T. ) ;
#7225 = ORIENTED_EDGE ( 'NONE', *, *, #36714, .T. ) ;
#7226 = ADVANCED_FACE ( 'NONE', ( #7583, #26183 ), #33514, .T. ) ;
#7227 = DIRECTION ( 'NONE',  ( 0.000000000000000000, 0.9510565162951546414, -0.3090169943749446202 ) ) ;
#7228 = ORIENTED_EDGE ( 'NONE', *, *, #46135, .T. ) ;
#7229 = EDGE_CURVE ( 'NONE', #37417, #34741, #3664, .T. ) ;
#7230 = VECTOR ( 'NONE', #12828, 1000.000000000000114 ) ;
#7231 = VECTOR ( 'NONE', #14243, 1000.000000000000000 ) ;
#7232 = CARTESIAN_POINT ( 'NONE',  ( 22.08297821871651934, -111.8242998470044540, 5.500000000000000000 ) ) ;
#7233 = EDGE_CURVE ( 'NONE', #22033, #31962, #2761, .T. ) ;
#7234 = CARTESIAN_POINT ( 'NONE',  ( 0.000000000000000000, -22.67460108101783334, 6.353146135317912169 ) ) ;
#7235 = AXIS2_PLACEMENT_3D ( 'NONE', #12936, #43026, #39109 ) ;
#7236 = PLANE ( 'NONE',  #6624 ) ;
#7237 = VERTEX_POINT ( 'NONE', #45495 ) ;
#7238 = DIRECTION ( 'NONE',  ( 8.090853898039828715E-17, -9.269810975720166919E-17, 1.000000000000000000 ) ) ;
#7239 = AXIS2_PLACEMENT_3D ( 'NONE', #34947, #2152, #9007 ) ;
#7240 = VERTEX_POINT ( 'NONE', #30102 ) ;
#7241 = AXIS2_PLACEMENT_3D ( 'NONE', #6200, #35080, #27998 ) ;
#7242 = ORIENTED_EDGE ( 'NONE', *, *, #46007, .F. ) ;
#7243 = DIRECTION ( 'NONE',  ( -1.000000000000000000, 0.000000000000000000, 0.000000000000000000 ) ) ;
#7244 = CARTESIAN_POINT ( 'NONE',  ( 5.999999999999999112, 60.67117009219134616, 55.16347631943062879 ) ) ;
#7245 = CARTESIAN_POINT ( 'NONE',  ( -6.170112525937321735, 10.87104923258428180, -44.99999999999998579 ) ) ;
#7246 = AXIS2_PLACEMENT_3D ( 'NONE', #5521, #31736, #32198 ) ;
#7247 = ORIENTED_EDGE ( 'NONE', *, *, #19926, .T. ) ;
#7248 = ORIENTED_EDGE ( 'NONE', *, *, #23677, .F. ) ;
#7249 = DIRECTION ( 'NONE',  ( -1.000000000000000000, 0.000000000000000000, 0.000000000000000000 ) ) ;
#7250 = ORIENTED_EDGE ( 'NONE', *, *, #12186, .F. ) ;
#7251 = CARTESIAN_POINT ( 'NONE',  ( 10.00000000000000000, -21.53537804866103045, 30.80686688397002371 ) ) ;
#7252 = CIRCLE ( 'NONE', #44778, 82.00000000000000000 ) ;
#7253 = CARTESIAN_POINT ( 'NONE',  ( 10.00000000000000000, 0.000000000000000000, 0.000000000000000000 ) ) ;
#7254 = CARTESIAN_POINT ( 'NONE',  ( 11.99999999999999822, -24.73286445877757345, 73.44644590900053061 ) ) ;
#7255 = DIRECTION ( 'NONE',  ( 0.000000000000000000, 0.000000000000000000, 1.000000000000000000 ) ) ;
#7256 = DIRECTION ( 'NONE',  ( -1.000000000000000000, 0.000000000000000000, 0.000000000000000000 ) ) ;
#7257 = LINE ( 'NONE', #4078, #33456 ) ;
#7258 = CYLINDRICAL_SURFACE ( 'NONE', #8566, 31.99999999999999289 ) ;
#7259 = DIRECTION ( 'NONE',  ( -1.000000000000000000, -0.000000000000000000, -0.000000000000000000 ) ) ;
#7260 = CARTESIAN_POINT ( 'NONE',  ( 0.000000000000000000, 0.000000000000000000, 0.000000000000000000 ) ) ;
#7261 = EDGE_CURVE ( 'NONE', #10144, #1961, #3905, .T. ) ;
#7262 = EDGE_LOOP ( 'NONE', ( #2811, #46865, #10780, #16393 ) ) ;
#7263 = DIRECTION ( 'NONE',  ( 0.000000000000000000, -0.5000000000000039968, 0.8660254037844363761 ) ) ;
#7264 = LINE ( 'NONE', #36875, #16763 ) ;
#7265 = CARTESIAN_POINT ( 'NONE',  ( 22.08297821871651934, -111.8242998470044540, 5.500000000000000000 ) ) ;
#7266 = CIRCLE ( 'NONE', #39312, 37.49900000000000233 ) ;
#7267 = DIRECTION ( 'NONE',  ( -1.000000000000000000, -0.000000000000000000, 0.000000000000000000 ) ) ;
#7268 = CARTESIAN_POINT ( 'NONE',  ( 10.00000000000000000, -6.555932627142676772, 37.01155633439056203 ) ) ;
#7270 = CIRCLE ( 'NONE', #14294, 11.59999999999999964 ) ;
#7269 = DIRECTION ( 'NONE',  ( 0.000000000000000000, 0.000000000000000000, -1.000000000000000000 ) ) ;
#7271 = CYLINDRICAL_SURFACE ( 'NONE', #46668, 82.00000000000000000 ) ;
#7272 = CYLINDRICAL_SURFACE ( 'NONE', #3427, 82.00000000000000000 ) ;
#7273 = AXIS2_PLACEMENT_3D ( 'NONE', #33919, #30499, #7971 ) ;
#7274 = AXIS2_PLACEMENT_3D ( 'NONE', #28441, #43385, #2486 ) ;
#7275 = CARTESIAN_POINT ( 'NONE',  ( 11.99999999999999822, 10.30890764327501863, -81.34940948281324324 ) ) ;
#7276 = AXIS2_PLACEMENT_3D ( 'NONE', #7526, #18757, #3846 ) ;
#7277 = DIRECTION ( 'NONE',  ( 0.000000000000000000, 0.9723699203976773342, -0.2334453638559024213 ) ) ;
#7278 = VERTEX_POINT ( 'NONE', #41362 ) ;
#7279 = ORIENTED_EDGE ( 'NONE', *, *, #3922, .F. ) ;
#7280 = CIRCLE ( 'NONE', #40901, 16.00000000000000000 ) ;
#7281 = ADVANCED_FACE ( 'NONE', ( #4408 ), #14689, .F. ) ;
#7282 = AXIS2_PLACEMENT_3D ( 'NONE', #20342, #16930, #8851 ) ;
#7283 = ORIENTED_EDGE ( 'NONE', *, *, #34702, .T. ) ;
#7284 = CARTESIAN_POINT ( 'NONE',  ( 0.000000000000000000, -35.95386929396248377, -10.96151621346525751 ) ) ;
#7285 = EDGE_CURVE ( 'NONE', #27571, #18838, #17596, .T. ) ;
#7286 = CARTESIAN_POINT ( 'NONE',  ( 10.00000000000000000, 27.13269053701132094, -25.88420570971372570 ) ) ;
#7287 = VERTEX_POINT ( 'NONE', #15417 ) ;
#7288 = ORIENTED_EDGE ( 'NONE', *, *, #14705, .T. ) ;
#7289 = AXIS2_PLACEMENT_3D ( 'NONE', #37688, #29859, #19081 ) ;
#7290 = EDGE_CURVE ( 'NONE', #42611, #26945, #13701, .T. ) ;
#7291 = DIRECTION ( 'NONE',  ( -1.000000000000000000, 0.000000000000000000, -0.000000000000000000 ) ) ;
#7292 = VERTEX_POINT ( 'NONE', #33281 ) ;
#7293 = EDGE_CURVE ( 'NONE', #9579, #6370, #18594, .T. ) ;
#7294 = ORIENTED_EDGE ( 'NONE', *, *, #44526, .F. ) ;
#7295 = AXIS2_PLACEMENT_3D ( 'NONE', #15893, #4632, #30832 ) ;
#7296 = LINE ( 'NONE', #186, #33691 ) ;
#7297 = ORIENTED_EDGE ( 'NONE', *, *, #30792, .F. ) ;
#7298 = CARTESIAN_POINT ( 'NONE',  ( 10.00000000000000000, -63.97538442413463855, 51.29473840253199768 ) ) ;
#7299 = ORIENTED_EDGE ( 'NONE', *, *, #17739, .T. ) ;
#7300 = ORIENTED_EDGE ( 'NONE', *, *, #7893, .T. ) ;
#7301 = PLANE ( 'NONE',  #42378 ) ;
#7302 = AXIS2_PLACEMENT_3D ( 'NONE', #11379, #48079, #34110 ) ;
#7303 = VECTOR ( 'NONE', #1664, 1000.000000000000000 ) ;
#7304 = VECTOR ( 'NONE', #7651, 1000.000000000000000 ) ;
#7305 = EDGE_CURVE ( 'NONE', #29267, #44497, #481, .T. ) ;
#7306 = DIRECTION ( 'NONE',  ( -1.000000000000000000, 0.000000000000000000, 0.000000000000000000 ) ) ;
#7307 = CARTESIAN_POINT ( 'NONE',  ( 0.000000000000000000, -23.16143007188376757, -73.95703589263997912 ) ) ;
#7308 = ORIENTED_EDGE ( 'NONE', *, *, #17729, .T. ) ;
#7309 = ORIENTED_EDGE ( 'NONE', *, *, #32462, .F. ) ;
#7310 = DIRECTION ( 'NONE',  ( -1.000000000000000000, -0.000000000000000000, -0.000000000000000000 ) ) ;
#7311 = DIRECTION ( 'NONE',  ( -1.000000000000000000, 0.000000000000000000, -0.000000000000000000 ) ) ;
#7312 = VECTOR ( 'NONE', #24686, 1000.000000000000000 ) ;
#7313 = VECTOR ( 'NONE', #20159, 1000.000000000000000 ) ;
#7314 = ORIENTED_EDGE ( 'NONE', *, *, #32284, .F. ) ;
#7315 = ORIENTED_EDGE ( 'NONE', *, *, #37685, .T. ) ;
#7316 = AXIS2_PLACEMENT_3D ( 'NONE', #24960, #46779, #36464 ) ;
#7317 = DIRECTION ( 'NONE',  ( -1.000000000000000000, -0.000000000000000000, -0.000000000000000000 ) ) ;
#7318 = CARTESIAN_POINT ( 'NONE',  ( 11.99999999999999822, 0.000000000000000000, 0.000000000000000000 ) ) ;
#7319 = ORIENTED_EDGE ( 'NONE', *, *, #8301, .F. ) ;
#7320 = CIRCLE ( 'NONE', #5804, 31.99999999999998579 ) ;
#7321 = LINE ( 'NONE', #35804, #47213 ) ;
#7322 = CARTESIAN_POINT ( 'NONE',  ( 12.13205353604972991, -140.1820037904669789, 5.500000000000000000 ) ) ;
#7323 = CYLINDRICAL_SURFACE ( 'NONE', #30591, 31.99999999999998579 ) ;
#7324 = CARTESIAN_POINT ( 'NONE',  ( 6.000000000000000000, -71.87247863392384772, -39.47590169984923136 ) ) ;
#7325 = CARTESIAN_POINT ( 'NONE',  ( 10.00000000000000000, 33.80338159004283938, 16.23288003029508886 ) ) ;
#7326 = DIRECTION ( 'NONE',  ( -1.000000000000000000, 0.000000000000000000, 0.000000000000000000 ) ) ;
#7327 = DIRECTION ( 'NONE',  ( 0.000000000000000000, 0.000000000000000000, 1.000000000000000000 ) ) ;
#7328 = EDGE_CURVE ( 'NONE', #15373, #41886, #15286, .T. ) ;
#7329 = CARTESIAN_POINT ( 'NONE',  ( -3.000000000000000000, 24.81905959214275370, -9.408202855044498492 ) ) ;
#7330 = DIRECTION ( 'NONE',  ( -1.000000000000000000, 0.000000000000000000, 0.000000000000000000 ) ) ;
#7331 = EDGE_LOOP ( 'NONE', ( #41774, #13448, #24399, #20068 ) ) ;
#7332 = ADVANCED_FACE ( 'NONE', ( #29846 ), #22989, .T. ) ;
#7333 = LINE ( 'NONE', #37197, #5739 ) ;
#7334 = DIRECTION ( 'NONE',  ( 0.000000000000000000, 0.000000000000000000, 1.000000000000000000 ) ) ;
#7335 = SURFACE_SIDE_STYLE ('',( #47963 ) ) ;
#7336 = ADVANCED_FACE ( 'NONE', ( #18347 ), #19310, .T. ) ;
#7337 = CARTESIAN_POINT ( 'NONE',  ( 10.00000000000000000, -46.53671651293991118, 59.03961581697383565 ) ) ;
#7338 = CIRCLE ( 'NONE', #32366, 32.00000000000000000 ) ;
#7339 = ORIENTED_EDGE ( 'NONE', *, *, #46366, .F. ) ;
#7340 = CIRCLE ( 'NONE', #30029, 31.99999999999998579 ) ;
#7341 = CARTESIAN_POINT ( 'NONE',  ( -12.00000000000000000, 2.119128821244579932E-15, 17.30399999999999849 ) ) ;
#7342 = AXIS2_PLACEMENT_3D ( 'NONE', #42009, #26826, #41762 ) ;
#7343 = AXIS2_PLACEMENT_3D ( 'NONE', #35386, #13131, #24627 ) ;
#7344 = VERTEX_POINT ( 'NONE', #707 ) ;
#7345 = EDGE_CURVE ( 'NONE', #48195, #9112, #34235, .T. ) ;
#7346 = CARTESIAN_POINT ( 'NONE',  ( 4.999999999999999112, -40.98264845739755202, 9.188173127307159405 ) ) ;
#7347 = VERTEX_POINT ( 'NONE', #40622 ) ;
#7348 = ADVANCED_FACE ( 'NONE', ( #20279 ), #12960, .T. ) ;
#7349 = ADVANCED_FACE ( 'NONE', ( #30830 ), #38903, .T. ) ;
#7350 = ORIENTED_EDGE ( 'NONE', *, *, #11842, .T. ) ;
#7351 = AXIS2_PLACEMENT_3D ( 'NONE', #40572, #18041, #7031 ) ;
#7352 = CIRCLE ( 'NONE', #46430, 32.00000000000000000 ) ;
#7353 = AXIS2_PLACEMENT_3D ( 'NONE', #10522, #2678, #25435 ) ;
#7354 = DIRECTION ( 'NONE',  ( -1.000000000000000000, 0.000000000000000000, 0.000000000000000000 ) ) ;
#7355 = CIRCLE ( 'NONE', #48029, 77.49899999999999523 ) ;
#7356 = ORIENTED_EDGE ( 'NONE', *, *, #24030, .F. ) ;
#7357 = CARTESIAN_POINT ( 'NONE',  ( 11.99999999999999822, -60.67117009219096957, -55.16347631943106933 ) ) ;
#7358 = ORIENTED_EDGE ( 'NONE', *, *, #39699, .T. ) ;
#7359 = ORIENTED_EDGE ( 'NONE', *, *, #888, .T. ) ;
#7360 = VERTEX_POINT ( 'NONE', #16611 ) ;
#7361 = EDGE_CURVE ( 'NONE', #12014, #23939, #19532, .T. ) ;
#7362 = ORIENTED_EDGE ( 'NONE', *, *, #18272, .T. ) ;
#7363 = CARTESIAN_POINT ( 'NONE',  ( 0.000000000000000000, -14.66109333815410487, -73.73191006444587003 ) ) ;
#7364 = AXIS2_PLACEMENT_3D ( 'NONE', #12877, #23392, #19465 ) ;
#7365 = LINE ( 'NONE', #33543, #45357 ) ;
#7366 = ORIENTED_EDGE ( 'NONE', *, *, #20532, .F. ) ;
#7367 = VERTEX_POINT ( 'NONE', #12467 ) ;
#7368 = CARTESIAN_POINT ( 'NONE',  ( 0.000000000000000000, -120.0000000000000000, -125.0000000000000000 ) ) ;
#7369 = ORIENTED_EDGE ( 'NONE', *, *, #37162, .F. ) ;
#7370 = CIRCLE ( 'NONE', #44903, 77.49900000000000944 ) ;
#7371 = CYLINDRICAL_SURFACE ( 'NONE', #47315, 37.49900000000000233 ) ;
#7372 = CARTESIAN_POINT ( 'NONE',  ( -7.001685179585692254, -14.98378029539707512, -1.199999999999999956 ) ) ;
#7373 = ORIENTED_EDGE ( 'NONE', *, *, #48177, .T. ) ;
#7374 = CARTESIAN_POINT ( 'NONE',  ( 10.00000000000000000, 22.74946021919133088, 29.81001611431016229 ) ) ;
#7375 = CARTESIAN_POINT ( 'NONE',  ( 10.00000000000000000, 70.53064760720278059, 26.01480285779964774 ) ) ;
#7376 = CARTESIAN_POINT ( 'NONE',  ( 0.000000000000000000, -8.966570791700153364, -81.50828551894237251 ) ) ;
#7377 = AXIS2_PLACEMENT_3D ( 'NONE', #271, #22796, #44828 ) ;
#7378 = DIRECTION ( 'NONE',  ( 0.000000000000000000, 0.000000000000000000, -1.000000000000000000 ) ) ;
#7379 = ORIENTED_EDGE ( 'NONE', *, *, #3035, .F. ) ;
#7380 = DIRECTION ( 'NONE',  ( 0.000000000000000000, 0.000000000000000000, 1.000000000000000000 ) ) ;
#7381 = EDGE_LOOP ( 'NONE', ( #14241, #42122, #39035, #42487 ) ) ;
#7382 = VERTEX_POINT ( 'NONE', #34721 ) ;
#7383 = CARTESIAN_POINT ( 'NONE',  ( 15.00000000000000000, 26.49999999999999645, 1.499999999999995781 ) ) ;
#7384 = VECTOR ( 'NONE', #29024, 1000.000000000000114 ) ;
#7385 = CARTESIAN_POINT ( 'NONE',  ( -6.880223345695647197, -142.5202692415819854, 5.500000000000000000 ) ) ;
#7386 = EDGE_LOOP ( 'NONE', ( #4108, #47165, #16131, #37053 ) ) ;
#7387 = VECTOR ( 'NONE', #39753, 1000.000000000000114 ) ;
#7388 = CARTESIAN_POINT ( 'NONE',  ( 0.000000000000000000, -55.19960302592029677, -51.03279382321147750 ) ) ;
#7389 = DIRECTION ( 'NONE',  ( 0.000000000000000000, -0.9510565162951544194, 0.3090169943749450088 ) ) ;
#7390 = CARTESIAN_POINT ( 'NONE',  ( 0.000000000000000000, -29.01471420065507090, -76.69515212746047439 ) ) ;
#7391 = VECTOR ( 'NONE', #20609, 1000.000000000000000 ) ;
#7392 = CARTESIAN_POINT ( 'NONE',  ( 11.99999999999999822, 60.67117009219215618, -55.16347631942976903 ) ) ;
#7394 = EDGE_CURVE ( 'NONE', #10792, #36121, #12952, .T. ) ;
#7393 = DIRECTION ( 'NONE',  ( 0.000000000000000000, 0.000000000000000000, -1.000000000000000000 ) ) ;
#7395 = CARTESIAN_POINT ( 'NONE',  ( 10.00000000000000000, 21.60688246758585862, 79.10210256391376049 ) ) ;
#7396 = ORIENTED_EDGE ( 'NONE', *, *, #48049, .T. ) ;
#7397 = EDGE_CURVE ( 'NONE', #47663, #21394, #43414, .T. ) ;
#7398 = VECTOR ( 'NONE', #378, 1000.000000000000000 ) ;
#7399 = AXIS2_PLACEMENT_3D ( 'NONE', #6141, #21058, #16915 ) ;
#7400 = CARTESIAN_POINT ( 'NONE',  ( 10.00000000000000000, -8.840884882374576037, -74.65374052328658649 ) ) ;
#7401 = FACE_OUTER_BOUND ( 'NONE', #4361, .T. ) ;
#7402 = CARTESIAN_POINT ( 'NONE',  ( 11.99999999999999822, -51.03279382321048985, -55.19960302592120627 ) ) ;
#7404 = AXIS2_PLACEMENT_3D ( 'NONE', #14864, #10713, #29782 ) ;
#7403 = LINE ( 'NONE', #37988, #44266 ) ;
#7405 = ADVANCED_FACE ( 'NONE', ( #1204 ), #34969, .F. ) ;
#7406 = DIRECTION ( 'NONE',  ( -1.000000000000000000, 0.000000000000000000, 0.000000000000000000 ) ) ;
#7407 = CARTESIAN_POINT ( 'NONE',  ( 0.000000000000000000, -2.543863470247813119, -81.96053171279903893 ) ) ;
#7408 = LINE ( 'NONE', #18883, #27989 ) ;
#7409 = DIRECTION ( 'NONE',  ( -1.000000000000000000, -0.000000000000000000, -0.000000000000000000 ) ) ;
#7410 = EDGE_CURVE ( 'NONE', #35739, #35538, #12704, .T. ) ;
#7411 = AXIS2_PLACEMENT_3D ( 'NONE', #45674, #9424, #38833 ) ;
#7412 = ORIENTED_EDGE ( 'NONE', *, *, #37565, .F. ) ;
#7413 = ORIENTED_EDGE ( 'NONE', *, *, #38182, .F. ) ;
#7414 = CARTESIAN_POINT ( 'NONE',  ( 11.99999999999999822, -63.97538442413463855, 51.29473840253199057 ) ) ;
#7415 = ORIENTED_EDGE ( 'NONE', *, *, #43885, .T. ) ;
#7416 = DIRECTION ( 'NONE',  ( -1.000000000000000000, 0.000000000000000000, -0.000000000000000000 ) ) ;
#7417 = APPLICATION_PROTOCOL_DEFINITION ( 'draft international standard', 'automotive_design', 1998, #47580 ) ;
#7418 = ORIENTED_EDGE ( 'NONE', *, *, #20960, .T. ) ;
#7419 = DIRECTION ( 'NONE',  ( -1.000000000000000000, -0.000000000000000000, -0.000000000000000000 ) ) ;
#7420 = ORIENTED_EDGE ( 'NONE', *, *, #13609, .T. ) ;
#7421 = EDGE_CURVE ( 'NONE', #28409, #6291, #16858, .T. ) ;
#7422 = EDGE_CURVE ( 'NONE', #923, #27585, #35211, .T. ) ;
#7423 = VECTOR ( 'NONE', #95, 1000.000000000000000 ) ;
#7424 = VECTOR ( 'NONE', #16001, 1000.000000000000000 ) ;
#7425 = LINE ( 'NONE', #6702, #23709 ) ;
#7426 = ORIENTED_EDGE ( 'NONE', *, *, #47869, .T. ) ;
#7427 = ORIENTED_EDGE ( 'NONE', *, *, #43526, .F. ) ;
#7428 = EDGE_CURVE ( 'NONE', #36706, #37915, #8253, .T. ) ;
#7429 = AXIS2_PLACEMENT_3D ( 'NONE', #9169, #47350, #13329 ) ;
#7430 = AXIS2_PLACEMENT_3D ( 'NONE', #19072, #41129, #22515 ) ;
#7431 = DIRECTION ( 'NONE',  ( -0.1276937514489679404, -0.9918136447140103451, 0.000000000000000000 ) ) ;
#7432 = CARTESIAN_POINT ( 'NONE',  ( 10.00000000000000000, 0.000000000000000000, 0.000000000000000000 ) ) ;
#7434 = ORIENTED_EDGE ( 'NONE', *, *, #2941, .F. ) ;
#7433 = CYLINDRICAL_SURFACE ( 'NONE', #47295, 42.00000000000000000 ) ;
#7435 = ORIENTED_EDGE ( 'NONE', *, *, #35651, .T. ) ;
#7436 = CYLINDRICAL_SURFACE ( 'NONE', #29334, 32.00000000000000000 ) ;
#7437 = VERTEX_POINT ( 'NONE', #27397 ) ;
#7438 = AXIS2_PLACEMENT_3D ( 'NONE', #44948, #40789, #635 ) ;
#7439 = CARTESIAN_POINT ( 'NONE',  ( 0.000000000000000000, 77.49459641780886443, 0.8261519478433866359 ) ) ;
#7440 = DIRECTION ( 'NONE',  ( 0.000000000000000000, 0.000000000000000000, -1.000000000000000000 ) ) ;
#7441 = LINE ( 'NONE', #15277, #21241 ) ;
#7442 = CARTESIAN_POINT ( 'NONE',  ( 35.50000000000000711, -120.0000000000000000, 2.500000000000000000 ) ) ;
#7443 = ORIENTED_EDGE ( 'NONE', *, *, #46869, .T. ) ;
#7444 = CARTESIAN_POINT ( 'NONE',  ( 10.00000000000000000, 33.00180498840046539, 17.80606268964551120 ) ) ;
#7445 = ORIENTED_EDGE ( 'NONE', *, *, #38046, .T. ) ;
#7446 = ORIENTED_EDGE ( 'NONE', *, *, #41082, .T. ) ;
#7447 = CARTESIAN_POINT ( 'NONE',  ( -2.981742216678212820, 0.000000000000000000, 0.000000000000000000 ) ) ;
#7448 = CARTESIAN_POINT ( 'NONE',  ( 0.000000000000000000, 8.840884882375075193, 74.65374052328651544 ) ) ;
#7449 = VECTOR ( 'NONE', #9803, 1000.000000000000000 ) ;
#7450 = DIRECTION ( 'NONE',  ( -1.000000000000000000, -0.000000000000000000, -0.000000000000000000 ) ) ;
#7451 = DIRECTION ( 'NONE',  ( 0.000000000000000000, -0.5877852522924801315, 0.8090169943749421222 ) ) ;
#7452 = ORIENTED_EDGE ( 'NONE', *, *, #3127, .T. ) ;
#7453 = DIRECTION ( 'NONE',  ( -1.000000000000000000, 0.000000000000000000, 0.000000000000000000 ) ) ;
#7454 = CYLINDRICAL_SURFACE ( 'NONE', #19736, 77.49899999999999523 ) ;
#7455 = CARTESIAN_POINT ( 'NONE',  ( 0.000000000000000000, 10.96151621346487914, 35.95386929396260456 ) ) ;
#7456 = CARTESIAN_POINT ( 'NONE',  ( 10.00000000000000000, 0.000000000000000000, 0.000000000000000000 ) ) ;
#7457 = CIRCLE ( 'NONE', #34799, 16.00000000000000000 ) ;
#7458 = DIRECTION ( 'NONE',  ( 1.000000000000000000, 0.000000000000000000, -0.000000000000000000 ) ) ;
#7459 = DIRECTION ( 'NONE',  ( 0.000000000000000000, 0.000000000000000000, 1.000000000000000000 ) ) ;
#7460 = CARTESIAN_POINT ( 'NONE',  ( 12.00000000000000000, -18.13022148937242761, 15.02647892043569122 ) ) ;
#7461 = CARTESIAN_POINT ( 'NONE',  ( 0.000000000000000000, -10.30890764327323872, -81.34940948281348483 ) ) ;
#7462 = CIRCLE ( 'NONE', #30916, 31.99999999999999645 ) ;
#7463 = EDGE_CURVE ( 'NONE', #46126, #29279, #29323, .T. ) ;
#7464 = DIRECTION ( 'NONE',  ( 0.000000000000000000, 0.2334453638559058908, -0.9723699203976764460 ) ) ;
#7465 = DIRECTION ( 'NONE',  ( -1.000000000000000000, 0.000000000000000000, 0.000000000000000000 ) ) ;
#7466 = ADVANCED_FACE ( 'NONE', ( #5606 ), #35454, .T. ) ;
#7467 = CARTESIAN_POINT ( 'NONE',  ( -11.59999999999999964, -0.8299999999999986278, -1.199999999999999956 ) ) ;
#7468 = VECTOR ( 'NONE', #24054, 1000.000000000000000 ) ;
#7469 = VECTOR ( 'NONE', #43388, 1000.000000000000000 ) ;
#7470 = FACE_OUTER_BOUND ( 'NONE', #44631, .T. ) ;
#7471 = LINE ( 'NONE', #18707, #16752 ) ;
#7472 = DIRECTION ( 'NONE',  ( 0.000000000000000000, -0.8910065241883721177, 0.4539904997395382003 ) ) ;
#7473 = DIRECTION ( 'NONE',  ( 1.000000000000000000, -0.000000000000000000, -0.000000000000000000 ) ) ;
#7474 = AXIS2_PLACEMENT_3D ( 'NONE', #7924, #44653, #15296 ) ;
#7475 = DIRECTION ( 'NONE',  ( -0.000000000000000000, -0.000000000000000000, -1.000000000000000000 ) ) ;
#7476 = AXIS2_PLACEMENT_3D ( 'NONE', #38697, #35729, #46516 ) ;
#7477 = ORIENTED_EDGE ( 'NONE', *, *, #41611, .F. ) ;
#7478 = EDGE_CURVE ( 'NONE', #13639, #41791, #29386, .T. ) ;
#7479 = ORIENTED_EDGE ( 'NONE', *, *, #23360, .F. ) ;
#7480 = EDGE_CURVE ( 'NONE', #9901, #22127, #26912, .T. ) ;
#7481 = ADVANCED_FACE ( 'NONE', ( #16146 ), #27160, .T. ) ;
#7482 = ORIENTED_EDGE ( 'NONE', *, *, #22050, .T. ) ;
#7483 = AXIS2_PLACEMENT_3D ( 'NONE', #16523, #23616, #28260 ) ;
#7484 = DIRECTION ( 'NONE',  ( -1.000000000000000000, 0.000000000000000000, -0.000000000000000000 ) ) ;
#7485 = CIRCLE ( 'NONE', #23911, 42.00000000000000000 ) ;
#7486 = ORIENTED_EDGE ( 'NONE', *, *, #41658, .F. ) ;
#7487 = ADVANCED_FACE ( 'NONE', ( #31081 ), #46002, .T. ) ;
#7488 = CIRCLE ( 'NONE', #29391, 77.49900000000000944 ) ;
#7489 = DIRECTION ( 'NONE',  ( -1.000000000000000000, 0.000000000000000000, -0.000000000000000000 ) ) ;
#7490 = DIRECTION ( 'NONE',  ( 0.000000000000000000, 0.9238795325112851842, 0.3826834323650938341 ) ) ;
#7492 = ORIENTED_EDGE ( 'NONE', *, *, #25150, .F. ) ;
#7491 = DIRECTION ( 'NONE',  ( 0.000000000000000000, 0.000000000000000000, 1.000000000000000000 ) ) ;
#7493 = ORIENTED_EDGE ( 'NONE', *, *, #38470, .T. ) ;
#7494 = CARTESIAN_POINT ( 'NONE',  ( 6.000000000000000000, 8.966570791701871102, -81.50828551894218776 ) ) ;
#7495 = VERTEX_POINT ( 'NONE', #14147 ) ;
#7496 = ORIENTED_EDGE ( 'NONE', *, *, #26251, .F. ) ;
#7497 = ORIENTED_EDGE ( 'NONE', *, *, #13544, .T. ) ;
#7498 = EDGE_LOOP ( 'NONE', ( #46385, #33662, #35742, #35879 ) ) ;
#7499 = LINE ( 'NONE', #19226, #17826 ) ;
#7500 = CARTESIAN_POINT ( 'NONE',  ( 11.99999999999999822, 71.87247863392413194, 39.47590169984869846 ) ) ;
#7501 = DIRECTION ( 'NONE',  ( 0.000000000000000000, 0.000000000000000000, 1.000000000000000000 ) ) ;
#7502 = CIRCLE ( 'NONE', #39560, 12.49999999999999645 ) ;
#7503 = VERTEX_POINT ( 'NONE', #2173 ) ;
#7504 = ORIENTED_EDGE ( 'NONE', *, *, #35025, .F. ) ;
#7505 = DIRECTION ( 'NONE',  ( 0.000000000000000000, -0.3090169943749548342, 0.9510565162951511997 ) ) ;
#7506 = ORIENTED_EDGE ( 'NONE', *, *, #35798, .T. ) ;
#7507 = CARTESIAN_POINT ( 'NONE',  ( 11.99999999999999822, 31.46837873494978055, 68.27212725128286763 ) ) ;
#7508 = AXIS2_PLACEMENT_3D ( 'NONE', #19415, #27762, #34340 ) ;
#7509 = CYLINDRICAL_SURFACE ( 'NONE', #33471, 42.00000000000000000 ) ;
#7510 = FACE_OUTER_BOUND ( 'NONE', #6099, .T. ) ;
#7511 = LINE ( 'NONE', #37360, #6549 ) ;
#7512 = FACE_OUTER_BOUND ( 'NONE', #18993, .T. ) ;
#7513 = DIRECTION ( 'NONE',  ( -0.000000000000000000, -0.9135454576426059736, 0.4067366430757887730 ) ) ;
#7514 = CIRCLE ( 'NONE', #9045, 31.99999999999999289 ) ;
#7515 = CARTESIAN_POINT ( 'NONE',  ( 0.000000000000000000, 40.68715046381927891, 10.41901085202092858 ) ) ;
#7516 = DIRECTION ( 'NONE',  ( 0.000000000000000000, 0.000000000000000000, 1.000000000000000000 ) ) ;
#7517 = DIRECTION ( 'NONE',  ( 1.000000000000000000, 0.000000000000000000, 0.000000000000000000 ) ) ;
#7518 = CARTESIAN_POINT ( 'NONE',  ( -6.170112525937308412, 10.87104923258428890, 52.00000000000002132 ) ) ;
#7519 = ORIENTED_EDGE ( 'NONE', *, *, #17344, .T. ) ;
#7520 = EDGE_CURVE ( 'NONE', #2120, #26793, #16092, .T. ) ;
#7521 = DIRECTION ( 'NONE',  ( -1.000000000000000000, 0.000000000000000000, -0.000000000000000000 ) ) ;
#7522 = ADVANCED_FACE ( 'NONE', ( #6095 ), #39631, .T. ) ;
#7523 = DIRECTION ( 'NONE',  ( -1.000000000000000000, 0.000000000000000000, 0.000000000000000000 ) ) ;
#7524 = AXIS2_PLACEMENT_3D ( 'NONE', #45092, #41912, #15240 ) ;
#7525 = LINE ( 'NONE', #33694, #4034 ) ;
#7526 = CARTESIAN_POINT ( 'NONE',  ( 14.59956846177685996, -138.4757300459248484, 5.500000000000000000 ) ) ;
#7527 = AXIS2_PLACEMENT_3D ( 'NONE', #4194, #3200, #45068 ) ;
#7528 = EDGE_CURVE ( 'NONE', #21034, #21021, #24437, .T. ) ;
#7529 = EDGE_CURVE ( 'NONE', #41033, #30788, #2786, .T. ) ;
#7530 = DIRECTION ( 'NONE',  ( 0.000000000000000000, 0.000000000000000000, -1.000000000000000000 ) ) ;
#7531 = DIRECTION ( 'NONE',  ( 0.000000000000000000, 0.000000000000000000, 1.000000000000000000 ) ) ;
#7532 = DIRECTION ( 'NONE',  ( 0.4279312458753000703, 0.9038112904824842087, 0.000000000000000000 ) ) ;
#7533 = ADVANCED_FACE ( 'NONE', ( #6327 ), #9986, .T. ) ;
#7534 = CARTESIAN_POINT ( 'NONE',  ( 0.000000000000000000, 0.000000000000000000, 0.000000000000000000 ) ) ;
#7535 = EDGE_CURVE ( 'NONE', #31422, #3459, #43759, .T. ) ;
#7536 = FACE_OUTER_BOUND ( 'NONE', #21679, .T. ) ;
#7537 = DIRECTION ( 'NONE',  ( 0.000000000000000000, 0.000000000000000000, 1.000000000000000000 ) ) ;
#7538 = ORIENTED_EDGE ( 'NONE', *, *, #46610, .F. ) ;
#7539 = CIRCLE ( 'NONE', #46611, 21.00000000000000000 ) ;
#7540 = EDGE_CURVE ( 'NONE', #36257, #38129, #10227, .T. ) ;
#7541 = ORIENTED_EDGE ( 'NONE', *, *, #26320, .F. ) ;
#7542 = ORIENTED_EDGE ( 'NONE', *, *, #24869, .F. ) ;
#7543 = CIRCLE ( 'NONE', #34887, 32.00000000000000000 ) ;
#7544 = DIRECTION ( 'NONE',  ( 0.5687579148473765889, -0.8225049752423776450, 0.000000000000000000 ) ) ;
#7545 = DIRECTION ( 'NONE',  ( 0.000000000000000000, 0.5224985647159440250, 0.8526401643540951758 ) ) ;
#7546 = ORIENTED_EDGE ( 'NONE', *, *, #10924, .T. ) ;
#7547 = ADVANCED_FACE ( 'NONE', ( #20773 ), #2625, .T. ) ;
#7548 = AXIS2_PLACEMENT_3D ( 'NONE', #16856, #21227, #31806 ) ;
#7549 = CARTESIAN_POINT ( 'NONE',  ( 11.99999999999999822, 5.256550761633951296, -77.32052557432835727 ) ) ;
#7550 = ORIENTED_EDGE ( 'NONE', *, *, #6048, .T. ) ;
#7551 = EDGE_CURVE ( 'NONE', #12619, #3891, #33258, .T. ) ;
#7552 = AXIS2_PLACEMENT_3D ( 'NONE', #32821, #16947, #10313 ) ;
#7553 = DIRECTION ( 'NONE',  ( -1.000000000000000000, 0.000000000000000000, 0.000000000000000000 ) ) ;
#7554 = CIRCLE ( 'NONE', #27911, 16.00000000000000000 ) ;
#7555 = EDGE_CURVE ( 'NONE', #39954, #26342, #9052, .T. ) ;
#7556 = DIRECTION ( 'NONE',  ( 1.000000000000000000, -0.000000000000000000, 0.000000000000000000 ) ) ;
#7557 = ORIENTED_EDGE ( 'NONE', *, *, #6041, .F. ) ;
#7558 = DIRECTION ( 'NONE',  ( -1.000000000000000000, 0.000000000000000000, -0.000000000000000000 ) ) ;
#7559 = ORIENTED_EDGE ( 'NONE', *, *, #18220, .F. ) ;
#7560 = CARTESIAN_POINT ( 'NONE',  ( 0.000000000000000000, 3.894527615419058009, -81.90746397400384637 ) ) ;
#7561 = DIRECTION ( 'NONE',  ( 0.000000000000000000, 1.000000000000000000, 3.469446951953615767E-15 ) ) ;
#7562 = CARTESIAN_POINT ( 'NONE',  ( 8.700667342345820288, -98.11853780484867116, -5.500000000000000000 ) ) ;
#7563 = AXIS2_PLACEMENT_3D ( 'NONE', #14127, #42851, #24008 ) ;
#7564 = ORIENTED_EDGE ( 'NONE', *, *, #4613, .T. ) ;
#7565 = ORIENTED_EDGE ( 'NONE', *, *, #12999, .T. ) ;
#7567 = EDGE_CURVE ( 'NONE', #42120, #42306, #5149, .T. ) ;
#7566 = FACE_OUTER_BOUND ( 'NONE', #16870, .T. ) ;
#7568 = DIRECTION ( 'NONE',  ( 0.000000000000000000, -0.3090169943749549453, 0.9510565162951511997 ) ) ;
#7569 = ORIENTED_EDGE ( 'NONE', *, *, #42987, .F. ) ;
#7570 = VERTEX_POINT ( 'NONE', #32516 ) ;
#7571 = EDGE_CURVE ( 'NONE', #17448, #20243, #36409, .T. ) ;
#7572 = CARTESIAN_POINT ( 'NONE',  ( 10.00000000000000000, 0.000000000000000000, 0.000000000000000000 ) ) ;
#7573 = ORIENTED_EDGE ( 'NONE', *, *, #47416, .T. ) ;
#7574 = DIRECTION ( 'NONE',  ( 0.000000000000000000, -0.9876883405951361050, -0.1564344650402419989 ) ) ;
#7575 = CARTESIAN_POINT ( 'NONE',  ( -10.00000000000000000, 0.000000000000000000, 0.000000000000000000 ) ) ;
#7576 = DIRECTION ( 'NONE',  ( -1.000000000000000000, 0.000000000000000000, 0.000000000000000000 ) ) ;
#7577 = DIRECTION ( 'NONE',  ( -1.000000000000000000, 0.000000000000000000, 0.000000000000000000 ) ) ;
#7578 = EDGE_CURVE ( 'NONE', #37298, #3370, #47658, .T. ) ;
#7579 = CARTESIAN_POINT ( 'NONE',  ( 10.00000000000000000, -10.74501242461258244, -35.92658777277521409 ) ) ;
#7580 = CARTESIAN_POINT ( 'NONE',  ( 22.51310757741980240, -113.2613067136482101, -2.500000000000000000 ) ) ;
#7581 = DIRECTION ( 'NONE',  ( 0.3311129884571281101, 0.9435911131814402886, -0.000000000000000000 ) ) ;
#7582 = FACE_OUTER_BOUND ( 'NONE', #37220, .T. ) ;
#7583 = FACE_BOUND ( 'NONE', #23989, .T. ) ;
#7584 = EDGE_CURVE ( 'NONE', #45066, #44958, #13189, .T. ) ;
#7585 = ORIENTED_EDGE ( 'NONE', *, *, #6635, .F. ) ;
#7586 = DIRECTION ( 'NONE',  ( 1.000000000000000000, -0.000000000000000000, -0.000000000000000000 ) ) ;
#7587 = FACE_OUTER_BOUND ( 'NONE', #22039, .T. ) ;
#7588 = VECTOR ( 'NONE', #20219, 1000.000000000000000 ) ;
#7589 = DIRECTION ( 'NONE',  ( 0.000000000000000000, 0.8526401643540897357, 0.5224985647159527957 ) ) ;
#7590 = ORIENTED_EDGE ( 'NONE', *, *, #29243, .F. ) ;
#7591 = CIRCLE ( 'NONE', #20908, 16.00000000000000000 ) ;
#7592 = UNCERTAINTY_MEASURE_WITH_UNIT (LENGTH_MEASURE( 1.000000000000000082E-05 ), #10355, 'distance_accuracy_value', 'NONE');
#7593 = DIRECTION ( 'NONE',  ( 1.000000000000000000, 0.000000000000000000, 0.000000000000000000 ) ) ;
#7594 = FACE_OUTER_BOUND ( 'NONE', #23487, .T. ) ;
#7595 = CARTESIAN_POINT ( 'NONE',  ( 5.000000000000000000, 41.91543099594818500, -2.663952781846291362 ) ) ;
#7596 = ORIENTED_EDGE ( 'NONE', *, *, #39522, .F. ) ;
#7597 = ORIENTED_EDGE ( 'NONE', *, *, #43605, .F. ) ;
#7598 = CIRCLE ( 'NONE', #42799, 82.00000000000000000 ) ;
#7599 = CARTESIAN_POINT ( 'NONE',  ( 15.00000000000000000, 14.60985201121703980, -18.46759930825707841 ) ) ;
#7600 = ORIENTED_EDGE ( 'NONE', *, *, #1779, .T. ) ;
#7601 = VECTOR ( 'NONE', #36880, 1000.000000000000000 ) ;
#7602 = ORIENTED_EDGE ( 'NONE', *, *, #5262, .T. ) ;
#7603 = ORIENTED_EDGE ( 'NONE', *, *, #44702, .F. ) ;
#7604 = EDGE_LOOP ( 'NONE', ( #35071, #22915, #32636, #20043 ) ) ;
#7605 = CARTESIAN_POINT ( 'NONE',  ( 4.999999999999999112, 41.81611651403861885, 3.925862922256313503 ) ) ;
#7606 = CARTESIAN_POINT ( 'NONE',  ( 0.000000000000000000, -70.52718814184240159, -26.02418014898383802 ) ) ;
#7607 = VERTEX_POINT ( 'NONE', #32043 ) ;
#7608 = AXIS2_PLACEMENT_3D ( 'NONE', #42137, #1506, #46290 ) ;
#7609 = VERTEX_POINT ( 'NONE', #46960 ) ;
#7610 = ORIENTED_EDGE ( 'NONE', *, *, #36844, .T. ) ;
#7611 = LINE ( 'NONE', #19098, #43905 ) ;
#7612 = ORIENTED_EDGE ( 'NONE', *, *, #7428, .T. ) ;
#7613 = DIRECTION ( 'NONE',  ( 0.000000000000000000, 1.000000000000000000, 3.469446951953614978E-15 ) ) ;
#7614 = CARTESIAN_POINT ( 'NONE',  ( 0.000000000000000000, -70.52718814184277107, 26.02418014898285037 ) ) ;
#7615 = ORIENTED_EDGE ( 'NONE', *, *, #4825, .F. ) ;
#7616 = ORIENTED_EDGE ( 'NONE', *, *, #23210, .T. ) ;
#7617 = CARTESIAN_POINT ( 'NONE',  ( 10.00000000000000000, 0.000000000000000000, 0.000000000000000000 ) ) ;
#7618 = DIRECTION ( 'NONE',  ( -1.000000000000000000, 0.000000000000000000, 0.000000000000000000 ) ) ;
#7619 = EDGE_LOOP ( 'NONE', ( #28890, #36613, #38299, #26084 ) ) ;
#7620 = AXIS2_PLACEMENT_3D ( 'NONE', #2693, #32570, #43816 ) ;
#7621 = CARTESIAN_POINT ( 'NONE',  ( 10.00000000000000000, 38.55633173627034438, -16.65560815589369881 ) ) ;
#7622 = LINE ( 'NONE', #10813, #10989 ) ;
#7623 = ORIENTED_EDGE ( 'NONE', *, *, #7520, .T. ) ;
#7624 = DIRECTION ( 'NONE',  ( -0.000000000000000000, -0.000000000000000000, -1.000000000000000000 ) ) ;
#7625 = ORIENTED_EDGE ( 'NONE', *, *, #9135, .T. ) ;
#7626 = VERTEX_POINT ( 'NONE', #43291 ) ;
#7627 = DIRECTION ( 'NONE',  ( -1.000000000000000000, 0.000000000000000000, 0.000000000000000000 ) ) ;
#7628 = DIRECTION ( 'NONE',  ( -1.000000000000000000, 0.000000000000000000, 0.000000000000000000 ) ) ;
#7629 = ORIENTED_EDGE ( 'NONE', *, *, #38441, .F. ) ;
#7630 = CARTESIAN_POINT ( 'NONE',  ( 10.00000000000000000, 33.00180498840072829, -17.80606268964504935 ) ) ;
#7631 = DIRECTION ( 'NONE',  ( 0.000000000000000000, -0.9876883405951359940, -0.1564344650402420822 ) ) ;
#7632 = CARTESIAN_POINT ( 'NONE',  ( -12.50000000000000000, -132.5000000000000000, 40.00000000000000000 ) ) ;
#7633 = EDGE_CURVE ( 'NONE', #30791, #43803, #23869, .T. ) ;
#7634 = DIRECTION ( 'NONE',  ( -1.000000000000000000, 0.000000000000000000, 0.000000000000000000 ) ) ;
#7635 = FACE_OUTER_BOUND ( 'NONE', #26616, .T. ) ;
#7636 = EDGE_CURVE ( 'NONE', #3648, #42120, #30992, .T. ) ;
#7637 = LINE ( 'NONE', #25507, #36428 ) ;
#7638 = CARTESIAN_POINT ( 'NONE',  ( 13.83832728059186046, -142.6495187161941089, 5.500000000000000000 ) ) ;
#7639 = CARTESIAN_POINT ( 'NONE',  ( 10.00000000000000000, 0.6853352020795618893, -37.58145647212453611 ) ) ;
#7640 = CARTESIAN_POINT ( 'NONE',  ( 5.000000000000002665, 74.18225833017937987, -34.94270380257560049 ) ) ;
#7641 = CARTESIAN_POINT ( 'NONE',  ( 0.000000000000000000, 0.000000000000000000, 0.000000000000000000 ) ) ;
#7642 = EDGE_CURVE ( 'NONE', #3459, #34359, #15316, .T. ) ;
#7643 = AXIS2_PLACEMENT_3D ( 'NONE', #5189, #20104, #45826 ) ;
#7644 = ADVANCED_FACE ( 'NONE', ( #16050 ), #24113, .T. ) ;
#7645 = FACE_OUTER_BOUND ( 'NONE', #17780, .T. ) ;
#7646 = CYLINDRICAL_SURFACE ( 'NONE', #38650, 31.99999999999999289 ) ;
#7647 = CARTESIAN_POINT ( 'NONE',  ( -43.60332556124591008, -133.0000000000000000, -2.500000000000002220 ) ) ;
#7648 = DIRECTION ( 'NONE',  ( 0.000000000000000000, 0.1564344650402242354, 0.9876883405951387696 ) ) ;
#7649 = ORIENTED_EDGE ( 'NONE', *, *, #1402, .T. ) ;
#7650 = ORIENTED_EDGE ( 'NONE', *, *, #18574, .F. ) ;
#7651 = DIRECTION ( 'NONE',  ( -1.000000000000000000, -0.000000000000000000, 0.000000000000000000 ) ) ;
#7652 = ORIENTED_EDGE ( 'NONE', *, *, #22459, .T. ) ;
#7653 = CARTESIAN_POINT ( 'NONE',  ( 11.99999999999999822, 78.73519480814954363, 22.90783923731657268 ) ) ;
#7654 = CARTESIAN_POINT ( 'NONE',  ( 5.000000000000000000, 46.11716303203188261, 67.80270845531904911 ) ) ;
#7655 = ORIENTED_EDGE ( 'NONE', *, *, #26269, .T. ) ;
#7656 = EDGE_CURVE ( 'NONE', #45038, #6991, #35608, .T. ) ;
#7657 = VECTOR ( 'NONE', #37358, 1000.000000000000000 ) ;
#7658 = CARTESIAN_POINT ( 'NONE',  ( -3.000000000000000000, -19.89357724625003598, 12.59942793731059574 ) ) ;
#7659 = ORIENTED_EDGE ( 'NONE', *, *, #9546, .F. ) ;
#7660 = EDGE_CURVE ( 'NONE', #29685, #33124, #1230, .T. ) ;
#7661 = VECTOR ( 'NONE', #14623, 1000.000000000000000 ) ;
#7662 = EDGE_CURVE ( 'NONE', #36733, #44017, #39040, .T. ) ;
#7663 = CARTESIAN_POINT ( 'NONE',  ( -11.68233973192911535, 0.000000000000000000, 0.000000000000000000 ) ) ;
#7664 = PLANE ( 'NONE',  #28895 ) ;
#7666 = ORIENTED_EDGE ( 'NONE', *, *, #16209, .T. ) ;
#7665 = DIRECTION ( 'NONE',  ( 0.000000000000000000, 0.000000000000000000, -1.000000000000000000 ) ) ;
#7667 = EDGE_CURVE ( 'NONE', #4717, #16717, #28595, .T. ) ;
#7668 = VERTEX_POINT ( 'NONE', #38313 ) ;
#7669 = AXIS2_PLACEMENT_3D ( 'NONE', #9242, #1917, #31789 ) ;
#7670 = AXIS2_PLACEMENT_3D ( 'NONE', #23143, #45659, #19448 ) ;
#7671 = ADVANCED_FACE ( 'NONE', ( #46633 ), #38562, .T. ) ;
#7672 = CARTESIAN_POINT ( 'NONE',  ( 10.00000000000000000, 0.000000000000000000, 0.000000000000000000 ) ) ;
#7673 = DIRECTION ( 'NONE',  ( 0.000000000000000000, 0.000000000000000000, 1.000000000000000000 ) ) ;
#7674 = CARTESIAN_POINT ( 'NONE',  ( 0.000000000000000000, -33.00180498840060039, 17.80606268964528027 ) ) ;
#7675 = DIRECTION ( 'NONE',  ( -1.000000000000000000, 0.000000000000000000, 0.000000000000000000 ) ) ;
#7676 = ORIENTED_EDGE ( 'NONE', *, *, #40960, .T. ) ;
#7677 = DIRECTION ( 'NONE',  ( 0.000000000000000000, 0.000000000000000000, 1.000000000000000000 ) ) ;
#7678 = VERTEX_POINT ( 'NONE', #5277 ) ;
#7679 = VERTEX_POINT ( 'NONE', #28033 ) ;
#7680 = CYLINDRICAL_SURFACE ( 'NONE', #18435, 42.00000000000000000 ) ;
#7681 = CARTESIAN_POINT ( 'NONE',  ( 10.00000000000000000, -55.38113227695743745, -54.21277698773734244 ) ) ;
#7682 = DIRECTION ( 'NONE',  ( -1.000000000000000000, 0.000000000000000000, 0.000000000000000000 ) ) ;
#7683 = DIRECTION ( 'NONE',  ( -1.000000000000000000, 0.000000000000000000, 0.000000000000000000 ) ) ;
#7684 = EDGE_LOOP ( 'NONE', ( #9004, #30482, #41099, #12907 ) ) ;
#7685 = DIRECTION ( 'NONE',  ( 0.000000000000000000, 0.000000000000000000, 1.000000000000000000 ) ) ;
#7686 = DIRECTION ( 'NONE',  ( 0.000000000000000000, -0.07845909572783053842, -0.9969173337331290741 ) ) ;
#7687 = EDGE_CURVE ( 'NONE', #24923, #20697, #455, .T. ) ;
#7688 = ADVANCED_FACE ( 'NONE', ( #16772 ), #35112, .T. ) ;
#7689 = FACE_OUTER_BOUND ( 'NONE', #33263, .T. ) ;
#7690 = DIRECTION ( 'NONE',  ( -1.000000000000000000, -0.000000000000000000, -0.000000000000000000 ) ) ;
#7691 = DIRECTION ( 'NONE',  ( -1.000000000000000000, 0.000000000000000000, 0.000000000000000000 ) ) ;
#7692 = DIRECTION ( 'NONE',  ( 0.000000000000000000, 0.000000000000000000, 1.000000000000000000 ) ) ;
#7693 = CARTESIAN_POINT ( 'NONE',  ( 0.000000000000000000, -71.21200624218768382, -40.65526001592688488 ) ) ;
#7694 = FACE_OUTER_BOUND ( 'NONE', #20717, .T. ) ;
#7695 = CARTESIAN_POINT ( 'NONE',  ( 0.000000000000000000, 36.88895765772633695, 6.736453364083687667 ) ) ;
#7696 = LINE ( 'NONE', #33634, #12782 ) ;
#7697 = DIRECTION ( 'NONE',  ( 0.000000000000000000, 0.000000000000000000, 1.000000000000000000 ) ) ;
#7698 = EDGE_CURVE ( 'NONE', #41154, #41259, #24343, .T. ) ;
#7699 = LINE ( 'NONE', #4521, #35749 ) ;
#7700 = LINE ( 'NONE', #1333, #25368 ) ;
#7701 = DIRECTION ( 'NONE',  ( -1.000000000000000000, 0.000000000000000000, 0.000000000000000000 ) ) ;
#7702 = CYLINDRICAL_SURFACE ( 'NONE', #16031, 31.99999999999999289 ) ;
#7703 = CIRCLE ( 'NONE', #7669, 31.99999999999998934 ) ;
#7704 = CIRCLE ( 'NONE', #41326, 42.00000000000000000 ) ;
#7705 = CIRCLE ( 'NONE', #33482, 31.99999999999998579 ) ;
#7706 = DIRECTION ( 'NONE',  ( -1.000000000000000000, 0.000000000000000000, 0.000000000000000000 ) ) ;
#7707 = ORIENTED_EDGE ( 'NONE', *, *, #25293, .F. ) ;
#7708 = VERTEX_POINT ( 'NONE', #8679 ) ;
#7709 = ORIENTED_EDGE ( 'NONE', *, *, #14574, .T. ) ;
#7710 = ORIENTED_EDGE ( 'NONE', *, *, #34911, .F. ) ;
#7711 = LINE ( 'NONE', #30245, #3895 ) ;
#7712 = ORIENTED_EDGE ( 'NONE', *, *, #24277, .F. ) ;
#7713 = VERTEX_POINT ( 'NONE', #20676 ) ;
#7714 = EDGE_CURVE ( 'NONE', #11606, #25587, #35612, .T. ) ;
#7715 = VECTOR ( 'NONE', #35988, 1000.000000000000000 ) ;
#7716 = EDGE_CURVE ( 'NONE', #34741, #47392, #30943, .T. ) ;
#7717 = PLANE ( 'NONE',  #45716 ) ;
#7718 = FACE_OUTER_BOUND ( 'NONE', #33454, .T. ) ;
#7720 = ORIENTED_EDGE ( 'NONE', *, *, #10172, .F. ) ;
#7719 = FACE_OUTER_BOUND ( 'NONE', #33668, .T. ) ;
#7721 = ADVANCED_FACE ( 'NONE', ( #8451 ), #31467, .T. ) ;
#7722 = ORIENTED_EDGE ( 'NONE', *, *, #14500, .T. ) ;
#7723 = DIRECTION ( 'NONE',  ( 0.000000000000000000, 0.000000000000000000, -1.000000000000000000 ) ) ;
#7724 = ORIENTED_EDGE ( 'NONE', *, *, #35656, .F. ) ;
#7725 = ORIENTED_EDGE ( 'NONE', *, *, #7551, .T. ) ;
#7726 = ADVANCED_FACE ( 'NONE', ( #19945 ), #31224, .T. ) ;
#7727 = ORIENTED_EDGE ( 'NONE', *, *, #48444, .T. ) ;
#7728 = FACE_OUTER_BOUND ( 'NONE', #27967, .T. ) ;
#7729 = DIRECTION ( 'NONE',  ( -1.000000000000000000, -0.000000000000000000, 0.000000000000000000 ) ) ;
#7730 = CARTESIAN_POINT ( 'NONE',  ( 0.000000000000000000, 0.000000000000000000, 0.000000000000000000 ) ) ;
#7731 = VERTEX_POINT ( 'NONE', #8933 ) ;
#7732 = VERTEX_POINT ( 'NONE', #2310 ) ;
#7733 = CIRCLE ( 'NONE', #3047, 82.00000000000000000 ) ;
#7734 = DIRECTION ( 'NONE',  ( 0.000000000000000000, 0.000000000000000000, 1.000000000000000000 ) ) ;
#7735 = VERTEX_POINT ( 'NONE', #36796 ) ;
#7736 = CARTESIAN_POINT ( 'NONE',  ( 11.99999999999999822, 0.000000000000000000, 0.000000000000000000 ) ) ;
#7737 = AXIS2_PLACEMENT_3D ( 'NONE', #24446, #5865, #20783 ) ;
#7738 = CARTESIAN_POINT ( 'NONE',  ( 0.000000000000000000, 10.74501242461282757, 35.92658777277515014 ) ) ;
#7739 = DIRECTION ( 'NONE',  ( -1.000000000000000000, -0.000000000000000000, 0.000000000000000000 ) ) ;
#7740 = LINE ( 'NONE', #19240, #43308 ) ;
#7741 = LINE ( 'NONE', #41521, #11057 ) ;
#7742 = DIRECTION ( 'NONE',  ( 0.000000000000000000, 0.000000000000000000, 1.000000000000000000 ) ) ;
#7743 = AXIS2_PLACEMENT_3D ( 'NONE', #29697, #33382, #38023 ) ;
#7744 = CARTESIAN_POINT ( 'NONE',  ( 5.999999999999999112, -51.29473840253269401, 63.97538442413407012 ) ) ;
#7745 = EDGE_CURVE ( 'NONE', #22843, #24574, #12977, .T. ) ;
#7746 = EDGE_CURVE ( 'NONE', #37588, #16358, #9904, .T. ) ;
#7747 = CYLINDRICAL_SURFACE ( 'NONE', #21187, 16.00000000000000000 ) ;
#7748 = CARTESIAN_POINT ( 'NONE',  ( 5.999999999999999112, 44.99326035066149387, -68.55367621811095091 ) ) ;
#7749 = ORIENTED_EDGE ( 'NONE', *, *, #33453, .T. ) ;
#7750 = DIRECTION ( 'NONE',  ( -1.000000000000000000, 0.000000000000000000, 0.000000000000000000 ) ) ;
#7751 = VERTEX_POINT ( 'NONE', #35842 ) ;
#7752 = DIRECTION ( 'NONE',  ( -1.000000000000000000, 0.000000000000000000, -0.000000000000000000 ) ) ;
#7753 = CIRCLE ( 'NONE', #41372, 31.99999999999998224 ) ;
#7754 = DIRECTION ( 'NONE',  ( -1.000000000000000000, -0.000000000000000000, -0.000000000000000000 ) ) ;
#7755 = DIRECTION ( 'NONE',  ( 1.000000000000000000, 0.000000000000000000, -0.000000000000000000 ) ) ;
#7756 = DIRECTION ( 'NONE',  ( 1.000000000000000000, 0.000000000000000000, -0.000000000000000000 ) ) ;
#7757 = DIRECTION ( 'NONE',  ( 0.6862798483830533369, 0.7273375899149812085, -0.000000000000000000 ) ) ;
#7758 = DIRECTION ( 'NONE',  ( -1.000000000000000000, 0.000000000000000000, -0.000000000000000000 ) ) ;
#7759 = ADVANCED_FACE ( 'NONE', ( #43450 ), #10635, .F. ) ;
#7760 = FACE_OUTER_BOUND ( 'NONE', #21647, .T. ) ;
#7761 = LINE ( 'NONE', #32734, #39403 ) ;
#7762 = DIRECTION ( 'NONE',  ( -0.9997280174009349762, 0.02332147558787823691, 0.000000000000000000 ) ) ;
#7763 = CARTESIAN_POINT ( 'NONE',  ( 10.00000000000000000, -16.45098606841149902, 33.79645857604508308 ) ) ;
#7764 = ORIENTED_EDGE ( 'NONE', *, *, #21484, .F. ) ;
#7765 = EDGE_LOOP ( 'NONE', ( #19746, #6874, #35666, #41608 ) ) ;
#7766 = AXIS2_PLACEMENT_3D ( 'NONE', #36520, #2985, #29170 ) ;
#7767 = ORIENTED_EDGE ( 'NONE', *, *, #15584, .F. ) ;
#7768 = AXIS2_PLACEMENT_3D ( 'NONE', #44678, #11157, #18724 ) ;
#7769 = VECTOR ( 'NONE', #37635, 1000.000000000000000 ) ;
#7770 = LINE ( 'NONE', #431, #7769 ) ;
#7771 = FACE_OUTER_BOUND ( 'NONE', #36073, .T. ) ;
#7772 = ORIENTED_EDGE ( 'NONE', *, *, #22543, .T. ) ;
#7773 = VECTOR ( 'NONE', #30435, 1000.000000000000227 ) ;
#7774 = CARTESIAN_POINT ( 'NONE',  ( -3.000000000000000000, -19.89357724624987256, -12.59942793731086041 ) ) ;
#7775 = ADVANCED_FACE ( 'NONE', ( #25058 ), #6471, .T. ) ;
#7776 = ORIENTED_EDGE ( 'NONE', *, *, #4537, .T. ) ;
#7777 = VERTEX_POINT ( 'NONE', #39775 ) ;
#7778 = ADVANCED_FACE ( 'NONE', ( #17230 ), #32649, .F. ) ;
#7779 = EDGE_CURVE ( 'NONE', #6370, #33987, #32187, .T. ) ;
#7780 = CARTESIAN_POINT ( 'NONE',  ( 6.000000000000000000, -81.90746397400391743, 3.894527615417579636 ) ) ;
#7781 = CARTESIAN_POINT ( 'NONE',  ( 0.000000000000000000, -30.80686688397025108, 21.53537804866070715 ) ) ;
#7782 = EDGE_CURVE ( 'NONE', #36901, #14848, #33519, .T. ) ;
#7783 = CARTESIAN_POINT ( 'NONE',  ( -22.67106064244953245, -113.6342314410295842, 5.500000000000000000 ) ) ;
#7784 = VERTEX_POINT ( 'NONE', #13572 ) ;
#7785 = DIRECTION ( 'NONE',  ( 0.000000000000000000, -0.1564344650402172687, -0.9876883405951399908 ) ) ;
#7786 = EDGE_CURVE ( 'NONE', #29688, #42999, #43910, .T. ) ;
#7787 = ORIENTED_EDGE ( 'NONE', *, *, #4749, .F. ) ;
#7788 = CARTESIAN_POINT ( 'NONE',  ( 0.000000000000000000, 71.27951684758068041, -30.41916302227035018 ) ) ;
#7789 = CARTESIAN_POINT ( 'NONE',  ( 0.000000000000000000, -0.6853352020793173072, 37.58145647212453611 ) ) ;
#7790 = CARTESIAN_POINT ( 'NONE',  ( -1.200000000000000030E-05, 0.9569279952884557350, -2.499999999999984457 ) ) ;
#7791 = ORIENTED_EDGE ( 'NONE', *, *, #18880, .T. ) ;
#7792 = ORIENTED_EDGE ( 'NONE', *, *, #21286, .F. ) ;
#7793 = ADVANCED_FACE ( 'NONE', ( #14292, #29224 ), #36086, .T. ) ;
#7794 = CYLINDRICAL_SURFACE ( 'NONE', #2419, 16.00000000000000000 ) ;
#7795 = AXIS2_PLACEMENT_3D ( 'NONE', #22984, #476, #26664 ) ;
#7796 = DIRECTION ( 'NONE',  ( -1.000000000000000000, 0.000000000000000000, 0.000000000000000000 ) ) ;
#7797 = ORIENTED_EDGE ( 'NONE', *, *, #814, .F. ) ;
#7798 = VECTOR ( 'NONE', #33602, 1000.000000000000000 ) ;
#7799 = ORIENTED_EDGE ( 'NONE', *, *, #40807, .F. ) ;
#7800 = EDGE_CURVE ( 'NONE', #14425, #8228, #16339, .T. ) ;
#7801 = CARTESIAN_POINT ( 'NONE',  ( 0.000000000000000000, 0.000000000000000000, 0.000000000000000000 ) ) ;
#7802 = VERTEX_POINT ( 'NONE', #25296 ) ;
#7803 = FACE_OUTER_BOUND ( 'NONE', #32080, .T. ) ;
#7804 = AXIS2_PLACEMENT_3D ( 'NONE', #22159, #18236, #614 ) ;
#7805 = CARTESIAN_POINT ( 'NONE',  ( 10.00000000000000000, 0.000000000000000000, 0.000000000000000000 ) ) ;
#7806 = DIRECTION ( 'NONE',  ( -1.000000000000000000, -0.000000000000000000, 0.000000000000000000 ) ) ;
#7807 = CARTESIAN_POINT ( 'NONE',  ( 10.00000000000000000, 16.95692799528845640, -2.500000000000000000 ) ) ;
#7808 = DIRECTION ( 'NONE',  ( 0.000000000000000000, -0.6691306063588569053, -0.7431448254773954654 ) ) ;
#7809 = CARTESIAN_POINT ( 'NONE',  ( 10.00000000000000000, 64.81221759200342092, 50.23322058963369585 ) ) ;
#7810 = CIRCLE ( 'NONE', #22762, 42.00000000000000000 ) ;
#7811 = CARTESIAN_POINT ( 'NONE',  ( 10.00000000000000000, 27.75498641678742473, 31.52238457039609898 ) ) ;
#7812 = ADVANCED_FACE ( 'NONE', ( #6949 ), #28748, .T. ) ;
#7813 = DIRECTION ( 'NONE',  ( -0.000000000000000000, -0.000000000000000000, -1.000000000000000000 ) ) ;
#7814 = AXIS2_PLACEMENT_3D ( 'NONE', #35305, #1781, #31662 ) ;
#7815 = DIRECTION ( 'NONE',  ( 0.6516173805718058487, -0.7585478161175724932, 0.000000000000000000 ) ) ;
#7816 = ORIENTED_EDGE ( 'NONE', *, *, #12827, .F. ) ;
#7817 = FACE_OUTER_BOUND ( 'NONE', #31953, .T. ) ;
#7818 = CARTESIAN_POINT ( 'NONE',  ( -3.000000000000000000, -11.95096189432345390, 23.69967320028757385 ) ) ;
#7819 = PRESENTATION_STYLE_ASSIGNMENT (( #18820 ) ) ;
#7820 = CARTESIAN_POINT ( 'NONE',  ( -10.90076147243505211, 0.000000000000000000, 0.000000000000000000 ) ) ;
#7821 = ORIENTED_EDGE ( 'NONE', *, *, #6951, .F. ) ;
#7822 = EDGE_CURVE ( 'NONE', #1706, #20800, #17474, .T. ) ;
#7823 = FACE_OUTER_BOUND ( 'NONE', #44710, .T. ) ;
#7824 = DIRECTION ( 'NONE',  ( 0.000000000000000000, 0.9238795325112878487, -0.3826834323650874503 ) ) ;
#7825 = DIRECTION ( 'NONE',  ( -1.000000000000000000, 0.000000000000000000, 0.000000000000000000 ) ) ;
#7826 = ORIENTED_EDGE ( 'NONE', *, *, #35094, .F. ) ;
#7827 = ORIENTED_EDGE ( 'NONE', *, *, #8569, .F. ) ;
#7828 = EDGE_CURVE ( 'NONE', #35093, #45508, #3263, .T. ) ;
#7829 = FACE_OUTER_BOUND ( 'NONE', #25649, .T. ) ;
#7830 = CIRCLE ( 'NONE', #35195, 15.39727592608509177 ) ;
#7831 = ORIENTED_EDGE ( 'NONE', *, *, #31084, .T. ) ;
#7832 = EDGE_LOOP ( 'NONE', ( #18258, #12318, #5210, #17099 ) ) ;
#7833 = ADVANCED_FACE ( 'NONE', ( #47357 ), #33134, .F. ) ;
#7834 = ORIENTED_EDGE ( 'NONE', *, *, #22102, .T. ) ;
#7835 = EDGE_LOOP ( 'NONE', ( #20970, #30810, #15726, #4893 ) ) ;
#7836 = ORIENTED_EDGE ( 'NONE', *, *, #24553, .F. ) ;
#7837 = EDGE_CURVE ( 'NONE', #15162, #20655, #41366, .T. ) ;
#7838 = AXIS2_PLACEMENT_3D ( 'NONE', #19865, #35777, #2238 ) ;
#7839 = CIRCLE ( 'NONE', #17201, 31.99999999999999645 ) ;
#7840 = CARTESIAN_POINT ( 'NONE',  ( 10.00000000000000000, 0.6853352020790449695, 37.58145647212454321 ) ) ;
#7841 = AXIS2_PLACEMENT_3D ( 'NONE', #48192, #40135, #40849 ) ;
#7842 = ORIENTED_EDGE ( 'NONE', *, *, #9449, .F. ) ;
#7843 = ADVANCED_FACE ( 'NONE', ( #40975 ), #40719, .T. ) ;
#7844 = ORIENTED_EDGE ( 'NONE', *, *, #5687, .T. ) ;
#7845 = DIRECTION ( 'NONE',  ( -1.000000000000000000, -0.000000000000000000, 0.000000000000000000 ) ) ;
#7846 = VERTEX_POINT ( 'NONE', #11831 ) ;
#7847 = LINE ( 'NONE', #15676, #1184 ) ;
#7848 = CARTESIAN_POINT ( 'NONE',  ( 10.00000000000000000, 22.48208911017500355, 35.47612816024531668 ) ) ;
#7849 = ORIENTED_EDGE ( 'NONE', *, *, #17449, .T. ) ;
#7850 = CARTESIAN_POINT ( 'NONE',  ( 10.00000000000000000, 0.000000000000000000, 0.000000000000000000 ) ) ;
#7851 = DIRECTION ( 'NONE',  ( -1.000000000000000000, 0.000000000000000000, -0.000000000000000000 ) ) ;
#7852 = EDGE_LOOP ( 'NONE', ( #14082, #15206, #39587, #46868 ) ) ;
#7853 = CARTESIAN_POINT ( 'NONE',  ( -19.90058851926621131, -132.5883508287165853, 2.500000000000000000 ) ) ;
#7854 = CARTESIAN_POINT ( 'NONE',  ( 0.000000000000000000, 46.21855187248630159, 62.20884554314034176 ) ) ;
#7855 = ORIENTED_EDGE ( 'NONE', *, *, #31745, .T. ) ;
#7856 = CARTESIAN_POINT ( 'NONE',  ( 10.00000000000000000, 0.000000000000000000, 0.000000000000000000 ) ) ;
#7857 = ORIENTED_EDGE ( 'NONE', *, *, #24978, .F. ) ;
#7858 = VERTEX_POINT ( 'NONE', #22600 ) ;
#7859 = DIRECTION ( 'NONE',  ( 0.000000000000000000, -0.2334453638559126354, 0.9723699203976748917 ) ) ;
#7860 = DIRECTION ( 'NONE',  ( -1.000000000000000000, -0.000000000000000000, 0.000000000000000000 ) ) ;
#7861 = DIRECTION ( 'NONE',  ( 0.000000000000000000, 1.000000000000000000, 3.491481338843133355E-15 ) ) ;
#7862 = DIRECTION ( 'NONE',  ( -1.000000000000000000, -0.000000000000000000, -0.000000000000000000 ) ) ;
#7863 = DIRECTION ( 'NONE',  ( -1.000000000000000000, -0.000000000000000000, -0.000000000000000000 ) ) ;
#7864 = FACE_OUTER_BOUND ( 'NONE', #23863, .T. ) ;
#7865 = DIRECTION ( 'NONE',  ( 0.000000000000000000, 0.000000000000000000, 1.000000000000000000 ) ) ;
#7867 = AXIS2_PLACEMENT_3D ( 'NONE', #8413, #12575, #38041 ) ;
#7866 = DIRECTION ( 'NONE',  ( -0.000000000000000000, -0.000000000000000000, -1.000000000000000000 ) ) ;
#7868 = AXIS2_PLACEMENT_3D ( 'NONE', #21455, #43501, #14356 ) ;
#7869 = FACE_OUTER_BOUND ( 'NONE', #41514, .T. ) ;
#7870 = DIRECTION ( 'NONE',  ( 0.000000000000000000, 0.9969173337331281859, -0.07845909572784182107 ) ) ;
#7871 = DIRECTION ( 'NONE',  ( -1.000000000000000000, 0.000000000000000000, 0.000000000000000000 ) ) ;
#7872 = CYLINDRICAL_SURFACE ( 'NONE', #48148, 16.00000000000000000 ) ;
#7873 = AXIS2_PLACEMENT_3D ( 'NONE', #45360, #18922, #33861 ) ;
#7874 = CIRCLE ( 'NONE', #14136, 16.00000000000000000 ) ;
#7875 = FACE_OUTER_BOUND ( 'NONE', #6758, .T. ) ;
#7876 = DIRECTION ( 'NONE',  ( -1.000000000000000000, 0.000000000000000000, 0.000000000000000000 ) ) ;
#7877 = DIRECTION ( 'NONE',  ( 1.000000000000000000, 0.000000000000000000, 0.000000000000000000 ) ) ;
#7878 = DIRECTION ( 'NONE',  ( 0.000000000000000000, 0.9510565162951503115, 0.3090169943749573878 ) ) ;
#7879 = STYLED_ITEM ( 'NONE', ( #13752 ), #19912 ) ;
#7880 = VERTEX_POINT ( 'NONE', #22112 ) ;
#7881 = CIRCLE ( 'NONE', #15667, 16.00000000000000355 ) ;
#7882 = ORIENTED_EDGE ( 'NONE', *, *, #39703, .T. ) ;
#7883 = ADVANCED_FACE ( 'NONE', ( #18448 ), #30204, .T. ) ;
#7884 = DIRECTION ( 'NONE',  ( -1.000000000000000000, 0.000000000000000000, 0.000000000000000000 ) ) ;
#7885 = AXIS2_PLACEMENT_3D ( 'NONE', #17603, #7310, #36207 ) ;
#7886 = ORIENTED_EDGE ( 'NONE', *, *, #23157, .F. ) ;
#7887 = CARTESIAN_POINT ( 'NONE',  ( 0.000000000000000000, 30.80686688397010542, 21.53537804866092387 ) ) ;
#7888 = DIRECTION ( 'NONE',  ( -1.000000000000000000, 0.000000000000000000, 0.000000000000000000 ) ) ;
#7889 = ORIENTED_EDGE ( 'NONE', *, *, #9119, .F. ) ;
#7890 = EDGE_CURVE ( 'NONE', #29100, #41379, #18911, .T. ) ;
#7891 = CARTESIAN_POINT ( 'NONE',  ( 0.000000000000000000, -12.93880638057369659, 76.41127070299266677 ) ) ;
#7892 = VERTEX_POINT ( 'NONE', #30431 ) ;
#7893 = EDGE_CURVE ( 'NONE', #31795, #15510, #26509, .T. ) ;
#7894 = AXIS2_PLACEMENT_3D ( 'NONE', #21103, #31923, #28464 ) ;
#7895 = LINE ( 'NONE', #15729, #26909 ) ;
#7896 = CIRCLE ( 'NONE', #16546, 82.00000000000000000 ) ;
#7897 = EDGE_CURVE ( 'NONE', #14976, #30318, #38220, .T. ) ;
#7898 = LINE ( 'NONE', #3747, #17953 ) ;
#7900 = ORIENTED_EDGE ( 'NONE', *, *, #43224, .T. ) ;
#7899 = DIRECTION ( 'NONE',  ( -1.000000000000000000, 0.000000000000000000, 0.000000000000000000 ) ) ;
#7901 = AXIS2_PLACEMENT_3D ( 'NONE', #2201, #36449, #28857 ) ;
#7902 = AXIS2_PLACEMENT_3D ( 'NONE', #39098, #23678, #23434 ) ;
#7903 = ORIENTED_EDGE ( 'NONE', *, *, #42623, .F. ) ;
#7904 = EDGE_CURVE ( 'NONE', #15597, #20505, #4597, .T. ) ;
#7905 = DIRECTION ( 'NONE',  ( -1.000000000000000000, -0.000000000000000000, -0.000000000000000000 ) ) ;
#7906 = FACE_OUTER_BOUND ( 'NONE', #8036, .T. ) ;
#7907 = AXIS2_PLACEMENT_3D ( 'NONE', #34520, #45811, #42129 ) ;
#7908 = DIRECTION ( 'NONE',  ( -1.000000000000000000, 0.000000000000000000, 0.000000000000000000 ) ) ;
#7909 = DIRECTION ( 'NONE',  ( -1.000000000000000000, 0.000000000000000000, 0.000000000000000000 ) ) ;
#7910 = EDGE_LOOP ( 'NONE', ( #35360, #38006, #46552, #48130 ) ) ;
#7911 = CYLINDRICAL_SURFACE ( 'NONE', #9943, 14.09999999999999964 ) ;
#7912 = EDGE_LOOP ( 'NONE', ( #31298, #30088, #42262, #1675 ) ) ;
#7913 = ORIENTED_EDGE ( 'NONE', *, *, #11871, .T. ) ;
#7914 = DIRECTION ( 'NONE',  ( -1.000000000000000000, -0.000000000000000000, 0.000000000000000000 ) ) ;
#7915 = ADVANCED_FACE ( 'NONE', ( #7906 ), #15275, .T. ) ;
#7916 = CARTESIAN_POINT ( 'NONE',  ( 5.000000000000000000, -44.99326035066101781, 68.55367621811127776 ) ) ;
#7917 = DIRECTION ( 'NONE',  ( 0.000000000000000000, 0.000000000000000000, 1.000000000000000000 ) ) ;
#7918 = DIRECTION ( 'NONE',  ( -1.000000000000000000, -0.000000000000000000, -0.000000000000000000 ) ) ;
#7919 = ORIENTED_EDGE ( 'NONE', *, *, #24648, .T. ) ;
#7920 = DIRECTION ( 'NONE',  ( 0.000000000000000000, 0.000000000000000000, 1.000000000000000000 ) ) ;
#7921 = DIRECTION ( 'NONE',  ( 0.000000000000000000, 0.000000000000000000, -1.000000000000000000 ) ) ;
#7922 = CARTESIAN_POINT ( 'NONE',  ( 11.99999999999999822, 81.50828551894227303, 8.966570791700986476 ) ) ;
#7923 = CYLINDRICAL_SURFACE ( 'NONE', #4877, 31.99999999999999289 ) ;
#7924 = CARTESIAN_POINT ( 'NONE',  ( -17.26469406256017791, -140.1601175325492648, 5.500000000000000000 ) ) ;
#7925 = DIRECTION ( 'NONE',  ( 0.000000000000000000, -0.9969173337331287410, 0.07845909572783486829 ) ) ;
#7926 = DIRECTION ( 'NONE',  ( -1.000000000000000000, -0.000000000000000000, -0.000000000000000000 ) ) ;
#7927 = CARTESIAN_POINT ( 'NONE',  ( 10.00000000000000000, -26.08949754953044220, 27.05870788708222818 ) ) ;
#7928 = CARTESIAN_POINT ( 'NONE',  ( -3.000000000000000000, -13.04903810567675038, 19.60159698893425428 ) ) ;
#7929 = FACE_OUTER_BOUND ( 'NONE', #22353, .T. ) ;
#7930 = DIRECTION ( 'NONE',  ( -0.000000000000000000, 0.000000000000000000, -1.000000000000000000 ) ) ;
#7931 = EDGE_CURVE ( 'NONE', #11606, #18781, #8500, .T. ) ;
#7932 = CARTESIAN_POINT ( 'NONE',  ( 10.00000000000000000, -44.88180994100421373, 63.18004540533011948 ) ) ;
#7933 = CARTESIAN_POINT ( 'NONE',  ( 11.99999999999999822, 20.40083707022882820, 72.35432306680490910 ) ) ;
#7934 = CARTESIAN_POINT ( 'NONE',  ( 10.00000000000000000, 25.88420570971400991, 27.13269053701105449 ) ) ;
#7935 = VERTEX_POINT ( 'NONE', #41448 ) ;
#7936 = CIRCLE ( 'NONE', #6407, 31.99999999999998579 ) ;
#7937 = EDGE_CURVE ( 'NONE', #15723, #13395, #11106, .T. ) ;
#7938 = CIRCLE ( 'NONE', #7058, 31.99999999999998579 ) ;
#7939 = CIRCLE ( 'NONE', #32958, 42.00000000000000000 ) ;
#7940 = ADVANCED_FACE ( 'NONE', ( #14782 ), #320, .T. ) ;
#7941 = DIRECTION ( 'NONE',  ( 0.000000000000000000, 0.000000000000000000, 1.000000000000000000 ) ) ;
#7942 = AXIS2_PLACEMENT_3D ( 'NONE', #39356, #43517, #2376 ) ;
#7943 = ORIENTED_EDGE ( 'NONE', *, *, #770, .T. ) ;
#7944 = CIRCLE ( 'NONE', #4819, 16.00000000000000000 ) ;
#7945 = DIRECTION ( 'NONE',  ( -1.000000000000000000, 0.000000000000000000, -0.000000000000000000 ) ) ;
#7946 = EDGE_CURVE ( 'NONE', #36155, #15680, #3052, .T. ) ;
#7947 = ORIENTED_EDGE ( 'NONE', *, *, #15605, .F. ) ;
#7948 = EDGE_CURVE ( 'NONE', #30446, #23907, #15504, .T. ) ;
#7949 = EDGE_CURVE ( 'NONE', #30385, #17705, #21806, .T. ) ;
#7950 = CYLINDRICAL_SURFACE ( 'NONE', #18349, 14.09999999999999964 ) ;
#7951 = CARTESIAN_POINT ( 'NONE',  ( 11.99999999999999822, 0.000000000000000000, 0.000000000000000000 ) ) ;
#7952 = DIRECTION ( 'NONE',  ( 0.000000000000000000, 0.000000000000000000, 1.000000000000000000 ) ) ;
#7953 = ORIENTED_EDGE ( 'NONE', *, *, #9061, .F. ) ;
#7954 = DIRECTION ( 'NONE',  ( -1.000000000000000000, -0.000000000000000000, -0.000000000000000000 ) ) ;
#7955 = ORIENTED_EDGE ( 'NONE', *, *, #31884, .F. ) ;
#7956 = ORIENTED_EDGE ( 'NONE', *, *, #6468, .F. ) ;
#7957 = LINE ( 'NONE', #15800, #8438 ) ;
#7958 = DIRECTION ( 'NONE',  ( 0.000000000000000000, 0.8660254037844432595, -0.4999999999999920064 ) ) ;
#7959 = CIRCLE ( 'NONE', #8770, 37.49900000000000233 ) ;
#7960 = CARTESIAN_POINT ( 'NONE',  ( 15.00000000000000000, -22.32062822937469093, 14.36278369418830181 ) ) ;
#7961 = ORIENTED_EDGE ( 'NONE', *, *, #5377, .F. ) ;
#7962 = ORIENTED_EDGE ( 'NONE', *, *, #7478, .T. ) ;
#7963 = CARTESIAN_POINT ( 'NONE',  ( 50.00005079999999680, 0.000000000000000000, 0.000000000000000000 ) ) ;
#7964 = VERTEX_POINT ( 'NONE', #41686 ) ;
#7965 = CIRCLE ( 'NONE', #4070, 31.99999999999999289 ) ;
#7966 = DIRECTION ( 'NONE',  ( -1.000000000000000000, -0.000000000000000000, 0.000000000000000000 ) ) ;
#7967 = CARTESIAN_POINT ( 'NONE',  ( 5.000000000000000000, -60.67117009219098378, -55.16347631943106933 ) ) ;
#7968 = DIRECTION ( 'NONE',  ( 0.000000000000000000, 0.000000000000000000, 1.000000000000000000 ) ) ;
#7969 = PLANE ( 'NONE',  #4973 ) ;
#7970 = CARTESIAN_POINT ( 'NONE',  ( 10.00000000000000000, 35.38097989696528600, -12.42422080174602605 ) ) ;
#7971 = DIRECTION ( 'NONE',  ( 0.000000000000000000, 0.000000000000000000, 1.000000000000000000 ) ) ;
#7972 = AXIS2_PLACEMENT_3D ( 'NONE', #44896, #10652, #36343 ) ;
#7973 = CARTESIAN_POINT ( 'NONE',  ( 10.00000000000000000, -30.84782396557233142, 21.32104025579104345 ) ) ;
#7974 = VERTEX_POINT ( 'NONE', #74 ) ;
#7975 = CARTESIAN_POINT ( 'NONE',  ( 15.00000000000000000, 23.49999999999999645, 1.499999999999995337 ) ) ;
#7976 = DIRECTION ( 'NONE',  ( 0.000000000000000000, -0.7431448254773856954, -0.6691306063588676745 ) ) ;
#7977 = ORIENTED_EDGE ( 'NONE', *, *, #37559, .F. ) ;
#7978 = CARTESIAN_POINT ( 'NONE',  ( 11.99999999999999822, 44.88180994100376608, 63.18004540533043922 ) ) ;
#7979 = ORIENTED_EDGE ( 'NONE', *, *, #30187, .T. ) ;
#7980 = ORIENTED_EDGE ( 'NONE', *, *, #19002, .T. ) ;
#7981 = DIRECTION ( 'NONE',  ( 0.000000000000000000, 0.000000000000000000, 1.000000000000000000 ) ) ;
#7982 = VECTOR ( 'NONE', #33256, 1000.000000000000000 ) ;
#7983 = CARTESIAN_POINT ( 'NONE',  ( 0.000000000000000000, 68.67312586195046720, -35.91791733033404199 ) ) ;
#7984 = CARTESIAN_POINT ( 'NONE',  ( 10.00000000000000000, -73.73191006444561424, -14.66109333815538918 ) ) ;
#7985 = CARTESIAN_POINT ( 'NONE',  ( 4.999999999999999112, -16.65560815589383381, -38.55633173627028754 ) ) ;
#7986 = ADVANCED_FACE ( 'NONE', ( #8154 ), #34322, .T. ) ;
#7987 = CARTESIAN_POINT ( 'NONE',  ( -3.000000000000000000, 23.59884966291538078, -12.14883922797231541 ) ) ;
#7988 = DIRECTION ( 'NONE',  ( -0.08130631524010122069, 0.9966891607226784355, 0.000000000000000000 ) ) ;
#7989 = ORIENTED_EDGE ( 'NONE', *, *, #43653, .T. ) ;
#7990 = EDGE_CURVE ( 'NONE', #34932, #35715, #31205, .T. ) ;
#7991 = CARTESIAN_POINT ( 'NONE',  ( 0.000000000000000000, 35.47612816024523852, 22.48208911017513145 ) ) ;
#7992 = LINE ( 'NONE', #34658, #37338 ) ;
#7993 = ADVANCED_FACE ( 'NONE', ( #44397 ), #25774, .T. ) ;
#7994 = AXIS2_PLACEMENT_3D ( 'NONE', #40089, #44718, #43996 ) ;
#7995 = EDGE_CURVE ( 'NONE', #17350, #15224, #38132, .T. ) ;
#7996 = CYLINDRICAL_SURFACE ( 'NONE', #22060, 12.49999999999999822 ) ;
#7997 = ORIENTED_EDGE ( 'NONE', *, *, #25941, .F. ) ;
#7998 = ORIENTED_EDGE ( 'NONE', *, *, #46549, .T. ) ;
#7999 = VERTEX_POINT ( 'NONE', #37645 ) ;
#8000 = AXIS2_PLACEMENT_3D ( 'NONE', #5887, #31597, #38436 ) ;
#8001 = VERTEX_POINT ( 'NONE', #33721 ) ;
#8002 = ORIENTED_EDGE ( 'NONE', *, *, #8221, .F. ) ;
#8003 = CARTESIAN_POINT ( 'NONE',  ( 11.99999999999999822, 76.41127070299290835, -12.93880638057234123 ) ) ;
#8004 = CARTESIAN_POINT ( 'NONE',  ( 11.99999999999999822, 31.46837873494978055, 68.27212725128286763 ) ) ;
#8005 = ORIENTED_EDGE ( 'NONE', *, *, #5466, .F. ) ;
#8006 = AXIS2_PLACEMENT_3D ( 'NONE', #590, #15520, #30451 ) ;
#8007 = ADVANCED_FACE ( 'NONE', ( #8015 ), #22953, .T. ) ;
#8008 = EDGE_CURVE ( 'NONE', #40594, #2738, #19499, .T. ) ;
#8009 = AXIS2_PLACEMENT_3D ( 'NONE', #17490, #20689, #32439 ) ;
#8010 = CARTESIAN_POINT ( 'NONE',  ( 10.00000000000000000, -54.21277698773636899, -55.38113227695839669 ) ) ;
#8011 = CIRCLE ( 'NONE', #3293, 13.71319123027096865 ) ;
#8012 = ORIENTED_EDGE ( 'NONE', *, *, #40747, .F. ) ;
#8013 = ORIENTED_EDGE ( 'NONE', *, *, #5274, .T. ) ;
#8014 = PRODUCT_RELATED_PRODUCT_CATEGORY ( 'part', '', ( #47219 ) ) ;
#8015 = FACE_OUTER_BOUND ( 'NONE', #44822, .T. ) ;
#8016 = EDGE_CURVE ( 'NONE', #24152, #15492, #36660, .T. ) ;
#8018 = ORIENTED_EDGE ( 'NONE', *, *, #40181, .T. ) ;
#8017 = LINE ( 'NONE', #446, #26634 ) ;
#8019 = CARTESIAN_POINT ( 'NONE',  ( -3.000000000000000000, -22.67460108101774807, -6.353146135318215038 ) ) ;
#8020 = ORIENTED_EDGE ( 'NONE', *, *, #20827, .T. ) ;
#8021 = CARTESIAN_POINT ( 'NONE',  ( 0.000000000000000000, 40.98264845739763018, -9.188173127306864529 ) ) ;
#8022 = ORIENTED_EDGE ( 'NONE', *, *, #27140, .T. ) ;
#8023 = ORIENTED_EDGE ( 'NONE', *, *, #16406, .F. ) ;
#8024 = DIRECTION ( 'NONE',  ( 0.000000000000000000, 0.9781476007338044676, 0.2079116908177653100 ) ) ;
#8025 = VECTOR ( 'NONE', #32081, 1000.000000000000000 ) ;
#8026 = CARTESIAN_POINT ( 'NONE',  ( 10.00000000000000000, 35.92658777277525672, -10.74501242461245809 ) ) ;
#8027 = CIRCLE ( 'NONE', #44787, 31.99999999999999289 ) ;
#8028 = CARTESIAN_POINT ( 'NONE',  ( 0.000000000000000000, 0.000000000000000000, 0.000000000000000000 ) ) ;
#8029 = ORIENTED_EDGE ( 'NONE', *, *, #45262, .T. ) ;
#8030 = ORIENTED_EDGE ( 'NONE', *, *, #3870, .T. ) ;
#8031 = CIRCLE ( 'NONE', #33048, 16.00000000000000000 ) ;
#8032 = FILL_AREA_STYLE_COLOUR ( '', #27426 ) ;
#8033 = CARTESIAN_POINT ( 'NONE',  ( 10.00000000000000000, 0.000000000000000000, 0.000000000000000000 ) ) ;
#8034 = CIRCLE ( 'NONE', #11966, 17.30399999999999849 ) ;
#8035 = ORIENTED_EDGE ( 'NONE', *, *, #48112, .F. ) ;
#8036 = EDGE_LOOP ( 'NONE', ( #5073, #5212, #47604, #26094 ) ) ;
#8037 = CYLINDRICAL_SURFACE ( 'NONE', #42389, 31.99999999999999289 ) ;
#8038 = ORIENTED_EDGE ( 'NONE', *, *, #17529, .F. ) ;
#8039 = AXIS2_PLACEMENT_3D ( 'NONE', #33493, #23211, #10986 ) ;
#8040 = CARTESIAN_POINT ( 'NONE',  ( 0.000000000000000000, 0.000000000000000000, 0.000000000000000000 ) ) ;
#8041 = DIRECTION ( 'NONE',  ( 0.000000000000000000, -0.8910065241883722287, 0.4539904997395382003 ) ) ;
#8042 = AXIS2_PLACEMENT_3D ( 'NONE', #7789, #18796, #19510 ) ;
#8043 = CYLINDRICAL_SURFACE ( 'NONE', #15382, 16.00000000000000000 ) ;
#8044 = DIRECTION ( 'NONE',  ( 0.000000000000000000, -0.1564344650402381687, 0.9876883405951365491 ) ) ;
#8045 = CARTESIAN_POINT ( 'NONE',  ( -6.719258119307966126, -15.35072898742050462, -1.199999999999999956 ) ) ;
#8046 = CARTESIAN_POINT ( 'NONE',  ( 11.99999999999999822, -62.20884554313985149, -46.21855187248698371 ) ) ;
#8047 = AXIS2_PLACEMENT_3D ( 'NONE', #6801, #43525, #2386 ) ;
#8048 = DIRECTION ( 'NONE',  ( -1.000000000000000000, 0.000000000000000000, 0.000000000000000000 ) ) ;
#8049 = AXIS2_PLACEMENT_3D ( 'NONE', #43634, #5238, #13786 ) ;
#8050 = FACE_OUTER_BOUND ( 'NONE', #42475, .T. ) ;
#8051 = DIRECTION ( 'NONE',  ( 0.000000000000000000, 0.8090169943749486725, -0.5877852522924713607 ) ) ;
#8052 = CIRCLE ( 'NONE', #33063, 82.00000000000000000 ) ;
#8053 = EDGE_CURVE ( 'NONE', #30740, #6106, #15570, .T. ) ;
#8054 = FACE_OUTER_BOUND ( 'NONE', #18067, .T. ) ;
#8055 = CYLINDRICAL_SURFACE ( 'NONE', #11355, 32.00000000000000000 ) ;
#8056 =( NAMED_UNIT ( * ) SI_UNIT ( $, .STERADIAN. ) SOLID_ANGLE_UNIT ( ) );
#8057 = DIRECTION ( 'NONE',  ( 0.9966891607226785466, 0.08130631524010119293, -0.000000000000000000 ) ) ;
#8058 = ADVANCED_FACE ( 'NONE', ( #37891 ), #15140, .F. ) ;
#8059 = ORIENTED_EDGE ( 'NONE', *, *, #11573, .T. ) ;
#8061 = EDGE_CURVE ( 'NONE', #2237, #1729, #18670, .T. ) ;
#8060 = UNCERTAINTY_MEASURE_WITH_UNIT (LENGTH_MEASURE( 1.000000000000000082E-05 ), #31007, 'distance_accuracy_value', 'NONE');
#8062 = CARTESIAN_POINT ( 'NONE',  ( 11.99999999999999822, 0.000000000000000000, 0.000000000000000000 ) ) ;
#8063 = DIRECTION ( 'NONE',  ( 0.000000000000000000, 0.000000000000000000, 1.000000000000000000 ) ) ;
#8064 = AXIS2_PLACEMENT_3D ( 'NONE', #25204, #47023, #35765 ) ;
#8065 = PLANE ( 'NONE',  #34669 ) ;
#8066 = VERTEX_POINT ( 'NONE', #15856 ) ;
#8067 = ADVANCED_FACE ( 'NONE', ( #30795 ), #4374, .T. ) ;
#8068 = AXIS2_PLACEMENT_3D ( 'NONE', #38905, #19786, #42084 ) ;
#8069 = EDGE_CURVE ( 'NONE', #24200, #22938, #27125, .T. ) ;
#8070 = DIRECTION ( 'NONE',  ( 0.000000000000000000, 0.000000000000000000, 1.000000000000000000 ) ) ;
#8071 = AXIS2_PLACEMENT_3D ( 'NONE', #36149, #13648, #24896 ) ;
#8072 = AXIS2_PLACEMENT_3D ( 'NONE', #14961, #19757, #30144 ) ;
#8073 = CIRCLE ( 'NONE', #37781, 16.00000000000000000 ) ;
#8074 = VECTOR ( 'NONE', #22906, 1000.000000000000000 ) ;
#8075 = VERTEX_POINT ( 'NONE', #30314 ) ;
#8076 = ORIENTED_EDGE ( 'NONE', *, *, #30132, .T. ) ;
#8077 = ORIENTED_EDGE ( 'NONE', *, *, #8458, .T. ) ;
#8078 = CIRCLE ( 'NONE', #25263, 77.49900000000000944 ) ;
#8079 = EDGE_CURVE ( 'NONE', #33302, #47783, #48375, .T. ) ;
#8080 = DIRECTION ( 'NONE',  ( 0.000000000000000000, 0.000000000000000000, 1.000000000000000000 ) ) ;
#8081 = CIRCLE ( 'NONE', #294, 31.99999999999999289 ) ;
#8082 = VECTOR ( 'NONE', #13125, 1000.000000000000114 ) ;
#8083 = ORIENTED_EDGE ( 'NONE', *, *, #19126, .F. ) ;
#8084 = ORIENTED_EDGE ( 'NONE', *, *, #17122, .F. ) ;
#8085 = VECTOR ( 'NONE', #15694, 1000.000000000000114 ) ;
#8086 = PLANE ( 'NONE',  #42338 ) ;
#8087 = CIRCLE ( 'NONE', #18246, 31.99999999999999289 ) ;
#8088 = ORIENTED_EDGE ( 'NONE', *, *, #4752, .T. ) ;
#8089 = LINE ( 'NONE', #46030, #9811 ) ;
#8090 = CARTESIAN_POINT ( 'NONE',  ( 26.47460221209471953, -121.8961639463267090, -2.500000000000000000 ) ) ;
#8092 = VERTEX_POINT ( 'NONE', #679 ) ;
#8091 = VECTOR ( 'NONE', #28501, 1000.000000000000000 ) ;
#8093 = FACE_OUTER_BOUND ( 'NONE', #44689, .T. ) ;
#8094 = ORIENTED_EDGE ( 'NONE', *, *, #22520, .F. ) ;
#8095 = ADVANCED_FACE ( 'NONE', ( #22708 ), #30066, .F. ) ;
#8097 = EDGE_LOOP ( 'NONE', ( #25811, #37643, #13167, #39458 ) ) ;
#8096 = LINE ( 'NONE', #46036, #27396 ) ;
#8098 = DIRECTION ( 'NONE',  ( 0.000000000000000000, 0.000000000000000000, 1.000000000000000000 ) ) ;
#8099 = VERTEX_POINT ( 'NONE', #19742 ) ;
#8100 = DIRECTION ( 'NONE',  ( 0.000000000000000000, 0.000000000000000000, 1.000000000000000000 ) ) ;
#8101 = ORIENTED_EDGE ( 'NONE', *, *, #5035, .F. ) ;
#8102 = DIRECTION ( 'NONE',  ( 0.000000000000000000, 0.000000000000000000, 1.000000000000000000 ) ) ;
#8103 = CARTESIAN_POINT ( 'NONE',  ( 11.99999999999999822, 23.16143007188426850, 73.95703589263983702 ) ) ;
#8104 = ORIENTED_EDGE ( 'NONE', *, *, #21080, .F. ) ;
#8105 = LINE ( 'NONE', #19120, #36309 ) ;
#8106 = CARTESIAN_POINT ( 'NONE',  ( 0.000000000000000000, 0.000000000000000000, 0.000000000000000000 ) ) ;
#8107 = DIRECTION ( 'NONE',  ( -1.000000000000000000, 0.000000000000000000, 0.000000000000000000 ) ) ;
#8108 = DIRECTION ( 'NONE',  ( -1.000000000000000000, -0.000000000000000000, 0.000000000000000000 ) ) ;
#8109 = DIRECTION ( 'NONE',  ( -1.000000000000000000, 0.000000000000000000, 0.000000000000000000 ) ) ;
#8110 = CYLINDRICAL_SURFACE ( 'NONE', #2843, 16.00000000000000000 ) ;
#8111 = EDGE_LOOP ( 'NONE', ( #32022, #22349, #9963, #45949 ) ) ;
#8112 = LINE ( 'NONE', #37985, #22347 ) ;
#8113 = DIRECTION ( 'NONE',  ( 0.000000000000000000, -0.9510565162951500895, -0.3090169943749583870 ) ) ;
#8114 = CARTESIAN_POINT ( 'NONE',  ( -12.50000000000000000, -132.5000000000000000, 40.00000000000000000 ) ) ;
#8115 = EDGE_CURVE ( 'NONE', #33547, #27354, #24932, .T. ) ;
#8116 = VECTOR ( 'NONE', #30218, 1000.000000000000000 ) ;
#8117 = AXIS2_PLACEMENT_3D ( 'NONE', #17788, #3334, #48372 ) ;
#8118 = CIRCLE ( 'NONE', #32378, 82.00000000000000000 ) ;
#8119 = EDGE_CURVE ( 'NONE', #4226, #10700, #24071, .T. ) ;
#8120 = CARTESIAN_POINT ( 'NONE',  ( -12.50000000000000000, -132.5000000000000000, -2.500000000000000000 ) ) ;
#8121 = CARTESIAN_POINT ( 'NONE',  ( 0.000000000000000000, 33.71516098798741012, 74.74816331893441657 ) ) ;
#8122 = LINE ( 'NONE', #23057, #20175 ) ;
#8123 = CARTESIAN_POINT ( 'NONE',  ( 0.000000000000000000, 68.67312586194995561, 35.91791733033500122 ) ) ;
#8124 = ADVANCED_FACE ( 'NONE', ( #14890 ), #26397, .T. ) ;
#8125 = VERTEX_POINT ( 'NONE', #44740 ) ;
#8126 = EDGE_CURVE ( 'NONE', #44023, #22951, #25712, .T. ) ;
#8128 = CARTESIAN_POINT ( 'NONE',  ( 10.00000000000000000, -16.23288003029521320, 33.80338159004277543 ) ) ;
#8127 = VECTOR ( 'NONE', #36648, 1000.000000000000000 ) ;
#8129 = EDGE_CURVE ( 'NONE', #16510, #13135, #9212, .T. ) ;
#8130 = ORIENTED_EDGE ( 'NONE', *, *, #37434, .T. ) ;
#8131 = ADVANCED_FACE ( 'NONE', ( #46925 ), #39597, .T. ) ;
#8132 = CIRCLE ( 'NONE', #331, 31.99999999999998224 ) ;
#8133 = LINE ( 'NONE', #11577, #6465 ) ;
#8134 = AXIS2_PLACEMENT_3D ( 'NONE', #8319, #27169, #15902 ) ;
#8135 = AXIS2_PLACEMENT_3D ( 'NONE', #27084, #38329, #24354 ) ;
#8136 = CONTEXT_DEPENDENT_SHAPE_REPRESENTATION ( #36649, #29658 ) ;
#8137 = FACE_OUTER_BOUND ( 'NONE', #46465, .T. ) ;
#8138 = CIRCLE ( 'NONE', #28432, 16.00000000000000000 ) ;
#8139 = VERTEX_POINT ( 'NONE', #43250 ) ;
#8140 = DIRECTION ( 'NONE',  ( -1.000000000000000000, -0.000000000000000000, 0.000000000000000000 ) ) ;
#8141 = ORIENTED_EDGE ( 'NONE', *, *, #31357, .T. ) ;
#8142 = EDGE_CURVE ( 'NONE', #45131, #26885, #4634, .T. ) ;
#8143 = DIRECTION ( 'NONE',  ( -1.000000000000000000, -0.000000000000000000, -0.000000000000000000 ) ) ;
#8144 = DIRECTION ( 'NONE',  ( -1.000000000000000000, 0.000000000000000000, -0.000000000000000000 ) ) ;
#8145 = VECTOR ( 'NONE', #43632, 1000.000000000000000 ) ;
#8147 = ORIENTED_EDGE ( 'NONE', *, *, #46618, .T. ) ;
#8146 = DIRECTION ( 'NONE',  ( 0.08130631524010120681, -0.9966891607226784355, 0.000000000000000000 ) ) ;
#8148 = AXIS2_PLACEMENT_3D ( 'NONE', #14522, #10845, #44372 ) ;
#8149 = VERTEX_POINT ( 'NONE', #9232 ) ;
#8150 = VECTOR ( 'NONE', #17661, 1000.000000000000000 ) ;
#8151 = EDGE_CURVE ( 'NONE', #22099, #9073, #28019, .T. ) ;
#8152 = ORIENTED_EDGE ( 'NONE', *, *, #6046, .T. ) ;
#8153 = CARTESIAN_POINT ( 'NONE',  ( 0.000000000000000000, 5.256550761632864166, 77.32052557432842832 ) ) ;
#8154 = FACE_OUTER_BOUND ( 'NONE', #15022, .T. ) ;
#8155 = DIRECTION ( 'NONE',  ( 0.000000000000000000, 0.000000000000000000, 1.000000000000000000 ) ) ;
#8156 = EDGE_CURVE ( 'NONE', #45983, #17444, #35805, .T. ) ;
#8157 = DIRECTION ( 'NONE',  ( 0.000000000000000000, 0.5877852522924744694, -0.8090169943749465631 ) ) ;
#8158 = AXIS2_PLACEMENT_3D ( 'NONE', #9227, #9954, #39091 ) ;
#8159 = AXIS2_PLACEMENT_3D ( 'NONE', #25932, #3666, #40871 ) ;
#8160 = ORIENTED_EDGE ( 'NONE', *, *, #23403, .F. ) ;
#8161 = DIRECTION ( 'NONE',  ( 1.000000000000000000, 0.000000000000000000, 0.000000000000000000 ) ) ;
#8162 = ORIENTED_EDGE ( 'NONE', *, *, #17582, .T. ) ;
#8163 = ORIENTED_EDGE ( 'NONE', *, *, #10017, .F. ) ;
#8164 = CIRCLE ( 'NONE', #34738, 31.99999999999998579 ) ;
#8165 = CARTESIAN_POINT ( 'NONE',  ( 5.000000000000002665, 15.33399622253600292, -80.55351364060572905 ) ) ;
#8166 = AXIS2_PLACEMENT_3D ( 'NONE', #2181, #39387, #34980 ) ;
#8167 = CYLINDRICAL_SURFACE ( 'NONE', #5081, 16.00000000000000000 ) ;
#8168 = FACE_OUTER_BOUND ( 'NONE', #17714, .T. ) ;
#8169 = DIRECTION ( 'NONE',  ( -1.000000000000000000, -0.000000000000000000, -0.000000000000000000 ) ) ;
#8170 = ORIENTED_EDGE ( 'NONE', *, *, #5220, .T. ) ;
#8171 = LINE ( 'NONE', #30685, #23770 ) ;
#8172 = AXIS2_PLACEMENT_3D ( 'NONE', #41056, #7517, #34170 ) ;
#8173 = DIRECTION ( 'NONE',  ( 0.000000000000000000, 0.8910065241883656784, 0.4539904997395511344 ) ) ;
#8174 = CARTESIAN_POINT ( 'NONE',  ( 0.000000000000000000, 73.72996012237460661, -14.67089635893632504 ) ) ;
#8175 = CARTESIAN_POINT ( 'NONE',  ( 0.000000000000000000, -74.65491531819124305, 8.830959090342128448 ) ) ;
#8176 = LINE ( 'NONE', #32150, #15343 ) ;
#8177 = DIRECTION ( 'NONE',  ( 0.000000000000000000, 0.000000000000000000, 1.000000000000000000 ) ) ;
#8178 = DIRECTION ( 'NONE',  ( -1.000000000000000000, -0.000000000000000000, -0.000000000000000000 ) ) ;
#8179 = LINE ( 'NONE', #15299, #48170 ) ;
#8180 = EDGE_CURVE ( 'NONE', #42173, #7626, #42532, .T. ) ;
#8181 = DIRECTION ( 'NONE',  ( -1.000000000000000000, 0.000000000000000000, 0.000000000000000000 ) ) ;
#8182 = DIRECTION ( 'NONE',  ( 0.8225049752423786442, 0.5687579148473752566, -0.000000000000000000 ) ) ;
#8183 = EDGE_CURVE ( 'NONE', #6187, #38183, #13151, .T. ) ;
#8184 = CARTESIAN_POINT ( 'NONE',  ( 10.00000000000000000, 0.000000000000000000, 0.000000000000000000 ) ) ;
#8185 = CARTESIAN_POINT ( 'NONE',  ( 10.00000000000000000, -10.96151621346461447, -35.95386929396268272 ) ) ;
#8186 = DIRECTION ( 'NONE',  ( -1.000000000000000000, -0.000000000000000000, 0.000000000000000000 ) ) ;
#8187 = DIRECTION ( 'NONE',  ( -1.000000000000000000, 0.000000000000000000, 0.000000000000000000 ) ) ;
#8188 = VERTEX_POINT ( 'NONE', #35168 ) ;
#8189 = EDGE_CURVE ( 'NONE', #25651, #35339, #31282, .T. ) ;
#8190 = VECTOR ( 'NONE', #2095, 1000.000000000000000 ) ;
#8191 = CIRCLE ( 'NONE', #12126, 32.00000000000000711 ) ;
#8192 = EDGE_CURVE ( 'NONE', #23375, #29705, #27860, .T. ) ;
#8193 = DIRECTION ( 'NONE',  ( -1.000000000000000000, 0.000000000000000000, -0.000000000000000000 ) ) ;
#8194 = EDGE_LOOP ( 'NONE', ( #8279, #5665, #19281, #18654 ) ) ;
#8195 = CIRCLE ( 'NONE', #32416, 42.00000000000000000 ) ;
#8196 = AXIS2_PLACEMENT_3D ( 'NONE', #45034, #42758, #11508 ) ;
#8197 = AXIS2_PLACEMENT_3D ( 'NONE', #27330, #37856, #16077 ) ;
#8198 = ORIENTED_EDGE ( 'NONE', *, *, #24318, .T. ) ;
#8199 = VERTEX_POINT ( 'NONE', #27597 ) ;
#8200 = ORIENTED_EDGE ( 'NONE', *, *, #41255, .F. ) ;
#8201 = CARTESIAN_POINT ( 'NONE',  ( 2.117611129180199558, -93.54218975225703048, -5.500000000000000000 ) ) ;
#8202 = ORIENTED_EDGE ( 'NONE', *, *, #41548, .T. ) ;
#8203 = AXIS2_PLACEMENT_3D ( 'NONE', #6488, #17741, #10154 ) ;
#8204 = VECTOR ( 'NONE', #25480, 1000.000000000000000 ) ;
#8205 = FACE_OUTER_BOUND ( 'NONE', #49, .T. ) ;
#8206 = DIRECTION ( 'NONE',  ( -1.000000000000000000, 0.000000000000000000, 0.000000000000000000 ) ) ;
#8207 = CARTESIAN_POINT ( 'NONE',  ( 10.00000000000000000, 16.45098606841173705, -33.79645857604496229 ) ) ;
#8208 = ORIENTED_EDGE ( 'NONE', *, *, #32162, .T. ) ;
#8209 = DIRECTION ( 'NONE',  ( 0.000000000000000000, -0.3826834323650970537, 0.9238795325112838519 ) ) ;
#8210 = AXIS2_PLACEMENT_3D ( 'NONE', #31563, #9032, #42572 ) ;
#8211 = ORIENTED_EDGE ( 'NONE', *, *, #6036, .T. ) ;
#8212 = CARTESIAN_POINT ( 'NONE',  ( 10.00000000000000000, -77.19088730480528682, 6.903761155837488062 ) ) ;
#8213 = CARTESIAN_POINT ( 'NONE',  ( 11.99999999999999822, -40.65526001592564853, -71.21200624218839437 ) ) ;
#8214 = CIRCLE ( 'NONE', #35583, 32.00000000000000000 ) ;
#8215 = ORIENTED_EDGE ( 'NONE', *, *, #39208, .F. ) ;
#8216 = EDGE_LOOP ( 'NONE', ( #13312, #19118, #36608, #13400 ) ) ;
#8217 = DIRECTION ( 'NONE',  ( 0.000000000000000000, 0.000000000000000000, -1.000000000000000000 ) ) ;
#8218 = VERTEX_POINT ( 'NONE', #6060 ) ;
#8219 = CIRCLE ( 'NONE', #35587, 32.00000000000000000 ) ;
#8220 = DIRECTION ( 'NONE',  ( -1.000000000000000000, 0.000000000000000000, 0.000000000000000000 ) ) ;
#8221 = EDGE_CURVE ( 'NONE', #23540, #23651, #5329, .T. ) ;
#8222 = DIRECTION ( 'NONE',  ( -1.000000000000000000, 0.000000000000000000, -0.000000000000000000 ) ) ;
#8223 = CYLINDRICAL_SURFACE ( 'NONE', #28378, 16.00000000000000000 ) ;
#8224 = CARTESIAN_POINT ( 'NONE',  ( 11.99999999999999822, 55.20638768913760686, 51.02545421589343988 ) ) ;
#8225 = DIRECTION ( 'NONE',  ( -0.8090169943749504489, 0.5877852522924689183, 0.000000000000000000 ) ) ;
#8226 = CARTESIAN_POINT ( 'NONE',  ( 4.999999999999999112, -9.188173127307004862, -40.98264845739759465 ) ) ;
#8227 = DIRECTION ( 'NONE',  ( 0.000000000000000000, 0.000000000000000000, 1.000000000000000000 ) ) ;
#8228 = VERTEX_POINT ( 'NONE', #20246 ) ;
#8229 = PLANE ( 'NONE',  #31392 ) ;
#8230 = DIRECTION ( 'NONE',  ( -0.8225049752423776450, -0.5687579148473765889, 0.000000000000000000 ) ) ;
#8231 = ORIENTED_EDGE ( 'NONE', *, *, #4630, .F. ) ;
#8232 = CARTESIAN_POINT ( 'NONE',  ( 11.99999999999999822, 5.256550761632864166, 77.32052557432842832 ) ) ;
#8233 = CARTESIAN_POINT ( 'NONE',  ( 10.00000000000000000, -17.67226234102849958, 33.17418723428301774 ) ) ;
#8234 = AXIS2_PLACEMENT_3D ( 'NONE', #46627, #2081, #32421 ) ;
#8235 = ORIENTED_EDGE ( 'NONE', *, *, #47916, .T. ) ;
#8236 = ORIENTED_EDGE ( 'NONE', *, *, #33873, .T. ) ;
#8237 = DIRECTION ( 'NONE',  ( -1.000000000000000000, -0.000000000000000000, 0.000000000000000000 ) ) ;
#8238 = CARTESIAN_POINT ( 'NONE',  ( 0.000000000000000000, 44.88180994100466847, -63.18004540532978552 ) ) ;
#8239 = FACE_OUTER_BOUND ( 'NONE', #47849, .T. ) ;
#8240 = FACE_OUTER_BOUND ( 'NONE', #3198, .T. ) ;
#8241 = EDGE_CURVE ( 'NONE', #6805, #43019, #37379, .T. ) ;
#8242 = CIRCLE ( 'NONE', #18406, 82.00000000000000000 ) ;
#8243 = EDGE_CURVE ( 'NONE', #46631, #16756, #43013, .T. ) ;
#8244 = CIRCLE ( 'NONE', #16847, 82.00000000000000000 ) ;
#8245 = EDGE_CURVE ( 'NONE', #43819, #35770, #15502, .T. ) ;
#8246 = DIRECTION ( 'NONE',  ( 0.000000000000000000, 0.000000000000000000, 1.000000000000000000 ) ) ;
#8247 = LINE ( 'NONE', #15366, #1355 ) ;
#8248 = ORIENTED_EDGE ( 'NONE', *, *, #19161, .T. ) ;
#8249 = VECTOR ( 'NONE', #14510, 1000.000000000000227 ) ;
#8250 = FACE_OUTER_BOUND ( 'NONE', #16828, .T. ) ;
#8251 = DIRECTION ( 'NONE',  ( -0.000000000000000000, -0.000000000000000000, -1.000000000000000000 ) ) ;
#8252 = EDGE_CURVE ( 'NONE', #10514, #29685, #20179, .T. ) ;
#8253 = CIRCLE ( 'NONE', #41839, 42.00000000000000000 ) ;
#8254 = ADVANCED_FACE ( 'NONE', ( #31528 ), #1165, .T. ) ;
#8255 = ORIENTED_EDGE ( 'NONE', *, *, #40959, .F. ) ;
#8256 = APPLICATION_PROTOCOL_DEFINITION ( 'draft international standard', 'automotive_design', 1998, #41030 ) ;
#8257 = DIRECTION ( 'NONE',  ( -1.000000000000000000, 0.000000000000000000, 0.000000000000000000 ) ) ;
#8258 = ORIENTED_EDGE ( 'NONE', *, *, #30845, .F. ) ;
#8259 = CIRCLE ( 'NONE', #41874, 82.00000000000000000 ) ;
#8260 = ORIENTED_EDGE ( 'NONE', *, *, #46212, .T. ) ;
#8261 = ORIENTED_EDGE ( 'NONE', *, *, #13856, .T. ) ;
#8262 = PLANE ( 'NONE',  #17135 ) ;
#8263 = DIRECTION ( 'NONE',  ( -1.000000000000000000, 0.000000000000000000, -0.000000000000000000 ) ) ;
#8264 = ORIENTED_EDGE ( 'NONE', *, *, #4491, .T. ) ;
#8265 = VECTOR ( 'NONE', #12493, 1000.000000000000000 ) ;
#8266 = FACE_OUTER_BOUND ( 'NONE', #15773, .T. ) ;
#8267 = EDGE_LOOP ( 'NONE', ( #14359, #39111, #31828, #38799 ) ) ;
#8268 = AXIS2_PLACEMENT_3D ( 'NONE', #40026, #36345, #17970 ) ;
#8269 = ORIENTED_EDGE ( 'NONE', *, *, #46189, .T. ) ;
#8270 = AXIS2_PLACEMENT_3D ( 'NONE', #15032, #41226, #17958 ) ;
#8271 = DIRECTION ( 'NONE',  ( 0.000000000000000000, 0.000000000000000000, 1.000000000000000000 ) ) ;
#8273 = VERTEX_POINT ( 'NONE', #45963 ) ;
#8272 = DIRECTION ( 'NONE',  ( -1.000000000000000000, -0.000000000000000000, -0.000000000000000000 ) ) ;
#8274 = CARTESIAN_POINT ( 'NONE',  ( 11.99999999999999822, -14.67089635893764665, 73.72996012237435082 ) ) ;
#8275 = EDGE_CURVE ( 'NONE', #24885, #19183, #12431, .T. ) ;
#8276 = ORIENTED_EDGE ( 'NONE', *, *, #38456, .T. ) ;
#8277 = AXIS2_PLACEMENT_3D ( 'NONE', #11625, #45158, #4292 ) ;
#8278 = CYLINDRICAL_SURFACE ( 'NONE', #27071, 37.49900000000000233 ) ;
#8279 = ORIENTED_EDGE ( 'NONE', *, *, #34927, .T. ) ;
#8280 = ORIENTED_EDGE ( 'NONE', *, *, #1764, .F. ) ;
#8281 = DIRECTION ( 'NONE',  ( 0.000000000000000000, 0.000000000000000000, 1.000000000000000000 ) ) ;
#8282 = ADVANCED_FACE ( 'NONE', ( #20003 ), #1415, .T. ) ;
#8283 = CARTESIAN_POINT ( 'NONE',  ( 0.000000000000000000, 0.000000000000000000, 0.000000000000000000 ) ) ;
#8284 = DIRECTION ( 'NONE',  ( 0.000000000000000000, -9.787530781167598712E-16, -1.000000000000000000 ) ) ;
#8285 = ADVANCED_FACE ( 'NONE', ( #47160 ), #10921, .F. ) ;
#8286 = ORIENTED_EDGE ( 'NONE', *, *, #45406, .F. ) ;
#8287 = ORIENTED_EDGE ( 'NONE', *, *, #41130, .F. ) ;
#8288 = CYLINDRICAL_SURFACE ( 'NONE', #3182, 77.49899999999999523 ) ;
#8289 = VECTOR ( 'NONE', #45817, 1000.000000000000000 ) ;
#8290 = DIRECTION ( 'NONE',  ( -1.000000000000000000, -0.000000000000000000, 0.000000000000000000 ) ) ;
#8291 = VERTEX_POINT ( 'NONE', #10692 ) ;
#8292 = DIRECTION ( 'NONE',  ( -1.000000000000000000, 0.000000000000000000, 0.000000000000000000 ) ) ;
#8293 = ORIENTED_EDGE ( 'NONE', *, *, #44474, .F. ) ;
#8294 = DIRECTION ( 'NONE',  ( -1.000000000000000000, 0.000000000000000000, 0.000000000000000000 ) ) ;
#8295 = DIRECTION ( 'NONE',  ( 0.000000000000000000, -0.3090169943749548342, 0.9510565162951510887 ) ) ;
#8296 = DIRECTION ( 'NONE',  ( 0.000000000000000000, 0.9781476007338069101, -0.2079116908177532086 ) ) ;
#8297 = LINE ( 'NONE', #34229, #36296 ) ;
#8298 = DIRECTION ( 'NONE',  ( 0.9781476007338070211, 0.000000000000000000, -0.2079116908177526257 ) ) ;
#8299 = CIRCLE ( 'NONE', #46608, 32.00000000000000000 ) ;
#8300 = CARTESIAN_POINT ( 'NONE',  ( 12.00000000000000000, -3.948201729842032215, 23.21447184625297666 ) ) ;
#8301 = EDGE_CURVE ( 'NONE', #2161, #44069, #23300, .T. ) ;
#8302 = EDGE_CURVE ( 'NONE', #34545, #42101, #10439, .T. ) ;
#8303 = FACE_OUTER_BOUND ( 'NONE', #39962, .T. ) ;
#8304 = CIRCLE ( 'NONE', #12233, 16.00000000000000000 ) ;
#8305 = LINE ( 'NONE', #11504, #41945 ) ;
#8306 = DIRECTION ( 'NONE',  ( 0.000000000000000000, 0.000000000000000000, 1.000000000000000000 ) ) ;
#8307 = AXIS2_PLACEMENT_3D ( 'NONE', #13067, #17430, #6201 ) ;
#8308 = DIRECTION ( 'NONE',  ( 0.000000000000000000, -0.9969173337331287410, 0.07845909572783489605 ) ) ;
#8309 = DIRECTION ( 'NONE',  ( 0.000000000000000000, 0.000000000000000000, 1.000000000000000000 ) ) ;
#8310 = DIRECTION ( 'NONE',  ( 0.000000000000000000, 0.000000000000000000, 1.000000000000000000 ) ) ;
#8311 = ORIENTED_EDGE ( 'NONE', *, *, #42710, .F. ) ;
#8312 = ADVANCED_FACE ( 'NONE', ( #25599 ), #3321, .T. ) ;
#8313 = ORIENTED_EDGE ( 'NONE', *, *, #11995, .F. ) ;
#8314 = DIRECTION ( 'NONE',  ( 1.000000000000000000, 0.000000000000000000, 0.000000000000000000 ) ) ;
#8315 = ORIENTED_EDGE ( 'NONE', *, *, #43498, .F. ) ;
#8316 = CIRCLE ( 'NONE', #20828, 31.99999999999998579 ) ;
#8317 = CARTESIAN_POINT ( 'NONE',  ( 0.000000000000000000, -120.0000000000000000, 2.500000000000000000 ) ) ;
#8318 = CIRCLE ( 'NONE', #31794, 82.00000000000000000 ) ;
#8319 = CARTESIAN_POINT ( 'NONE',  ( -10.00000000000000000, 0.000000000000000000, 0.000000000000000000 ) ) ;
#8320 = ORIENTED_EDGE ( 'NONE', *, *, #15276, .T. ) ;
#8321 = CIRCLE ( 'NONE', #4421, 82.00000000000000000 ) ;
#8322 = CARTESIAN_POINT ( 'NONE',  ( 0.000000000000000000, -13.04903810567647682, -19.60159698893442481 ) ) ;
#8323 = ORIENTED_EDGE ( 'NONE', *, *, #10407, .F. ) ;
#8324 = ORIENTED_EDGE ( 'NONE', *, *, #12136, .F. ) ;
#8325 = ORIENTED_EDGE ( 'NONE', *, *, #28301, .F. ) ;
#8326 = VECTOR ( 'NONE', #43198, 1000.000000000000000 ) ;
#8327 = DIRECTION ( 'NONE',  ( 0.000000000000000000, -1.000000000000000000, 0.000000000000000000 ) ) ;
#8328 = EDGE_CURVE ( 'NONE', #7146, #16268, #41302, .T. ) ;
#8329 = ORIENTED_EDGE ( 'NONE', *, *, #37364, .F. ) ;
#8330 = CARTESIAN_POINT ( 'NONE',  ( 10.00000000000000000, -46.21855187248583974, -62.20884554314070414 ) ) ;
#8331 = ORIENTED_EDGE ( 'NONE', *, *, #2303, .F. ) ;
#8332 = CARTESIAN_POINT ( 'NONE',  ( -24.50849501662245800, -109.8101191361138831, 5.500000000000000000 ) ) ;
#8333 = ORIENTED_EDGE ( 'NONE', *, *, #26841, .F. ) ;
#8334 = EDGE_CURVE ( 'NONE', #22480, #41344, #7000, .T. ) ;
#8335 = CARTESIAN_POINT ( 'NONE',  ( 10.00000000000000000, -77.16300072079640415, -27.74655509720751567 ) ) ;
#8336 = DIRECTION ( 'NONE',  ( -1.000000000000000000, 0.000000000000000000, -0.000000000000000000 ) ) ;
#8337 = EDGE_CURVE ( 'NONE', #14239, #10647, #14610, .T. ) ;
#8338 = VERTEX_POINT ( 'NONE', #40778 ) ;
#8339 = DIRECTION ( 'NONE',  ( 0.000000000000000000, 0.000000000000000000, 1.000000000000000000 ) ) ;
#8340 = EDGE_LOOP ( 'NONE', ( #44609, #12918, #28367, #36007 ) ) ;
#8341 = LINE ( 'NONE', #19571, #47694 ) ;
#8342 = DIRECTION ( 'NONE',  ( -1.000000000000000000, 0.000000000000000000, 0.000000000000000000 ) ) ;
#8343 = ORIENTED_EDGE ( 'NONE', *, *, #14574, .F. ) ;
#8344 = VECTOR ( 'NONE', #31310, 1000.000000000000000 ) ;
#8345 = CARTESIAN_POINT ( 'NONE',  ( 11.99999999999999822, 0.000000000000000000, 0.000000000000000000 ) ) ;
#8346 = ORIENTED_EDGE ( 'NONE', *, *, #22707, .T. ) ;
#8347 = ORIENTED_EDGE ( 'NONE', *, *, #34971, .T. ) ;
#8348 = DIRECTION ( 'NONE',  ( 1.000000000000000000, 0.000000000000000000, 0.000000000000000000 ) ) ;
#8349 = CARTESIAN_POINT ( 'NONE',  ( 0.000000000000000000, 0.000000000000000000, 0.000000000000000000 ) ) ;
#8350 = ORIENTED_EDGE ( 'NONE', *, *, #21488, .T. ) ;
#8351 = LINE ( 'NONE', #15692, #5006 ) ;
#8352 = DIRECTION ( 'NONE',  ( 0.000000000000000000, -0.9135454576426005335, -0.4067366430758010409 ) ) ;
#8353 = CARTESIAN_POINT ( 'NONE',  ( 8.700667342345820288, -98.11853780484867116, 5.500000000000000000 ) ) ;
#8354 = CIRCLE ( 'NONE', #28691, 0.2999999999999999334 ) ;
#8355 = DIRECTION ( 'NONE',  ( 1.000000000000000000, -0.000000000000000000, -0.000000000000000000 ) ) ;
#8356 = EDGE_CURVE ( 'NONE', #23469, #38800, #16278, .T. ) ;
#8357 = DIRECTION ( 'NONE',  ( 0.000000000000000000, 0.000000000000000000, -1.000000000000000000 ) ) ;
#8358 = EDGE_CURVE ( 'NONE', #23160, #3234, #33195, .T. ) ;
#8359 = AXIS2_PLACEMENT_3D ( 'NONE', #39376, #31080, #38902 ) ;
#8360 = DIRECTION ( 'NONE',  ( -1.000000000000000000, -0.000000000000000000, 0.000000000000000000 ) ) ;
#8361 = ORIENTED_EDGE ( 'NONE', *, *, #47210, .T. ) ;
#8362 = DIRECTION ( 'NONE',  ( 1.000000000000000000, -0.000000000000000000, 0.000000000000000000 ) ) ;
#8363 = EDGE_CURVE ( 'NONE', #17765, #2093, #43633, .T. ) ;
#8364 = LINE ( 'NONE', #18415, #42814 ) ;
#8365 = CARTESIAN_POINT ( 'NONE',  ( 11.99999999999999822, 5.256550761632864166, 77.32052557432842832 ) ) ;
#8366 = ORIENTED_EDGE ( 'NONE', *, *, #40414, .T. ) ;
#8367 = ORIENTED_EDGE ( 'NONE', *, *, #11208, .F. ) ;
#8368 = DIRECTION ( 'NONE',  ( -0.000000000000000000, -0.000000000000000000, -1.000000000000000000 ) ) ;
#8369 = DIRECTION ( 'NONE',  ( 0.000000000000000000, 0.4539904997395477482, -0.8910065241883673437 ) ) ;
#8370 = DIRECTION ( 'NONE',  ( 0.000000000000000000, 0.8090169943749486725, -0.5877852522924713607 ) ) ;
#8371 = DIRECTION ( 'NONE',  ( -1.000000000000000000, 0.000000000000000000, -0.000000000000000000 ) ) ;
#8372 = ORIENTED_EDGE ( 'NONE', *, *, #35034, .F. ) ;
#8373 = EDGE_CURVE ( 'NONE', #46408, #5128, #20956, .T. ) ;
#8374 = ORIENTED_EDGE ( 'NONE', *, *, #33058, .F. ) ;
#8375 = AXIS2_PLACEMENT_3D ( 'NONE', #6954, #40982, #44639 ) ;
#8376 = FACE_BOUND ( 'NONE', #34885, .T. ) ;
#8377 = VERTEX_POINT ( 'NONE', #2360 ) ;
#8378 = CARTESIAN_POINT ( 'NONE',  ( 0.000000000000000000, -36.72794159290197769, -65.59268652807249111 ) ) ;
#8379 = CYLINDRICAL_SURFACE ( 'NONE', #32316, 31.99999999999999289 ) ;
#8380 = ORIENTED_EDGE ( 'NONE', *, *, #32603, .T. ) ;
#8381 = CIRCLE ( 'NONE', #2890, 31.99999999999999289 ) ;
#8382 = DIRECTION ( 'NONE',  ( 0.000000000000000000, 0.000000000000000000, 1.000000000000000000 ) ) ;
#8383 = ORIENTED_EDGE ( 'NONE', *, *, #24710, .T. ) ;
#8384 = AXIS2_PLACEMENT_3D ( 'NONE', #42755, #9207, #31257 ) ;
#8385 = DIRECTION ( 'NONE',  ( 0.000000000000000000, -0.8090169943749403458, -0.5877852522924830181 ) ) ;
#8386 = ORIENTED_EDGE ( 'NONE', *, *, #197, .T. ) ;
#8387 = DIRECTION ( 'NONE',  ( 0.000000000000000000, 0.000000000000000000, 1.000000000000000000 ) ) ;
#8389 = VERTEX_POINT ( 'NONE', #17284 ) ;
#8388 = DIRECTION ( 'NONE',  ( -1.000000000000000000, -0.000000000000000000, -0.000000000000000000 ) ) ;
#8390 = ORIENTED_EDGE ( 'NONE', *, *, #44215, .F. ) ;
#8391 = ADVANCED_FACE ( 'NONE', ( #24881 ), #32239, .T. ) ;
#8392 = EDGE_CURVE ( 'NONE', #26170, #48358, #32704, .T. ) ;
#8393 = ADVANCED_FACE ( 'NONE', ( #2594 ), #17534, .T. ) ;
#8394 = CARTESIAN_POINT ( 'NONE',  ( 11.99999999999999822, 0.000000000000000000, 0.000000000000000000 ) ) ;
#8395 = CARTESIAN_POINT ( 'NONE',  ( 5.999999999999999112, 64.81221759200415988, -50.23322058963276504 ) ) ;
#8396 = LINE ( 'NONE', #4166, #15010 ) ;
#8397 = ADVANCED_FACE ( 'NONE', ( #28800 ), #43731, .T. ) ;
#8399 = DIRECTION ( 'NONE',  ( 0.000000000000000000, 0.000000000000000000, -1.000000000000000000 ) ) ;
#8398 = AXIS2_PLACEMENT_3D ( 'NONE', #2492, #12562, #2041 ) ;
#8400 = VERTEX_POINT ( 'NONE', #2848 ) ;
#8401 = FACE_OUTER_BOUND ( 'NONE', #683, .T. ) ;
#8402 = EDGE_LOOP ( 'NONE', ( #19914, #40047, #5077, #6636 ) ) ;
#8403 = ORIENTED_EDGE ( 'NONE', *, *, #30960, .T. ) ;
#8404 = EDGE_CURVE ( 'NONE', #24649, #27608, #47630, .T. ) ;
#8405 = DIRECTION ( 'NONE',  ( 0.000000000000000000, 0.000000000000000000, 1.000000000000000000 ) ) ;
#8406 = VECTOR ( 'NONE', #7988, 1000.000000000000114 ) ;
#8407 = CARTESIAN_POINT ( 'NONE',  ( 10.00000000000000000, 29.81001611431009479, 22.74946021919143391 ) ) ;
#8408 = DIRECTION ( 'NONE',  ( -1.000000000000000000, -0.000000000000000000, -0.000000000000000000 ) ) ;
#8409 = DIRECTION ( 'NONE',  ( 0.000000000000000000, 0.000000000000000000, 1.000000000000000000 ) ) ;
#8410 = EDGE_LOOP ( 'NONE', ( #44745, #23311, #16285, #19016 ) ) ;
#8411 = LINE ( 'NONE', #23573, #43307 ) ;
#8412 = LINE ( 'NONE', #30449, #17447 ) ;
#8413 = CARTESIAN_POINT ( 'NONE',  ( 10.00000000000000000, 0.000000000000000000, 0.000000000000000000 ) ) ;
#8414 = ADVANCED_FACE ( 'NONE', ( #11422 ), #15334, .F. ) ;
#8415 = DIRECTION ( 'NONE',  ( -0.000000000000000000, -0.000000000000000000, -1.000000000000000000 ) ) ;
#8416 = CARTESIAN_POINT ( 'NONE',  ( 10.00000000000000000, 55.19960302592066625, 51.03279382321107249 ) ) ;
#8417 = FACE_OUTER_BOUND ( 'NONE', #44005, .T. ) ;
#8418 = EDGE_CURVE ( 'NONE', #3180, #44307, #7957, .T. ) ;
#8419 = FACE_OUTER_BOUND ( 'NONE', #20142, .T. ) ;
#8420 = DIRECTION ( 'NONE',  ( -1.000000000000000000, 0.000000000000000000, 0.000000000000000000 ) ) ;
#8421 = CYLINDRICAL_SURFACE ( 'NONE', #37698, 42.00000000000000000 ) ;
#8422 = CARTESIAN_POINT ( 'NONE',  ( 10.00000000000000000, 66.50666863322055633, -39.78640506895536078 ) ) ;
#8423 = ORIENTED_EDGE ( 'NONE', *, *, #32008, .F. ) ;
#8424 = AXIS2_PLACEMENT_3D ( 'NONE', #29976, #41248, #44909 ) ;
#8425 = EDGE_CURVE ( 'NONE', #6273, #5369, #7499, .T. ) ;
#8426 = DIRECTION ( 'NONE',  ( -1.000000000000000000, 0.000000000000000000, -0.000000000000000000 ) ) ;
#8427 = DIRECTION ( 'NONE',  ( -1.000000000000000000, 0.000000000000000000, -0.000000000000000000 ) ) ;
#8428 = ORIENTED_EDGE ( 'NONE', *, *, #24594, .F. ) ;
#8429 = ORIENTED_EDGE ( 'NONE', *, *, #22345, .T. ) ;
#8430 = LINE ( 'NONE', #18948, #41676 ) ;
#8431 = EDGE_LOOP ( 'NONE', ( #30089, #4978, #37426, #116 ) ) ;
#8432 = ADVANCED_FACE ( 'NONE', ( #22177 ), #15555, .T. ) ;
#8433 = VECTOR ( 'NONE', #3095, 1000.000000000000000 ) ;
#8434 = EDGE_LOOP ( 'NONE', ( #17523, #46083, #6402, #47218, #19111, #43637, #34686, #29647, #22538, #1641, #7724, #10375, #5394, #36918, #17700, #40728, #26200, #1189, #8617, #34568, #9362, #25688, #28181, #2402, #43059, #32336, #8323, #35498, #42089, #12021, #11587, #5130, #7314, #39887, #46268, #25883, #9175, #21205, #17601, #28588, #20291, #17406, #1239, #2479, #38150, #32126, #37596, #41427, #42341, #3883, #42725, #19263, #3494, #19684, #18855, #47992, #24583, #39047, #40469, #40777, #19324, #47995, #32169, #37818, #4065, #4665, #17278, #3303, #5253, #38823, #47398, #32335, #4376, #26416, #47241, #32661, #15823, #13084, #4782, #37494, #45283, #18438, #15490, #40917, #42833, #40029, #19484, #26788, #30192, #44671, #47812, #23988, #19922, #13140, #18770, #29056, #1205, #7294, #24171, #19175, #23295, #22198, #43149, #25782, #46357, #47408, #35378, #25750, #8012, #14972, #7504, #24443, #35167, #34441, #5858, #44638, #16055, #36665, #23729, #29074, #40853, #34950, #31261, #5456, #34424, #1057, #16191, #2523, #43076, #2846, #7366, #35581, #39237, #43624, #14883, #37713, #17417, #14047, #41876, #2765, #21563, #22414, #46686, #15317, #24003, #19952, #1845, #1023, #29624, #32813, #7956, #16415, #3879, #26384, #4671, #23438, #19024, #46354, #5279, #17764, #44673, #40059, #20673, #40405, #27975, #46900, #46701, #13386, #23291, #12144, #34353, #36622, #41320, #7889, #12363, #36369, #26931, #12795, #31160, #5667, #33295, #33130, #1042, #6645, #19052, #6345, #3732, #35971, #3850, #28919, #4584, #26461, #5989, #26597, #4669, #3326, #10241, #2573, #43373, #40509, #36196, #16390, #1471, #25501, #32535, #3681, #43547, #42416, #44523, #27112, #9691, #5759, #40443, #1253, #45451, #34294, #45846, #12674, #15385, #24956, #20296, #23840, #3492, #34771, #24380, #43123, #28993, #38811, #8293, #40160, #23604, #17078, #12215, #46452, #28251, #32235, #36088, #6272, #35803, #36499, #31388, #12534, #5337, #21923, #14055, #5230, #16563, #32738, #34574, #20443, #29327, #44881, #48240, #24731, #12076, #46142, #47090, #12668, #42679, #20393, #15939, #42155, #2411, #23885, #5011, #44435, #45831, #37300, #47629, #40442, #43380, #21435, #23507, #19447, #45849, #9243, #9528, #33403, #22445, #25766, #11640, #40477, #20293, #45385, #34255, #42726, #2972, #13106, #523, #37690, #19275, #42353, #4616, #17653, #25182, #4126, #24322, #11561, #11925, #15806, #14836, #8927, #42100, #46016, #9034, #25118, #12592, #45062, #18782, #48345, #12204, #35723, #47149, #22484, #46369, #29545, #28970, #23637, #41311, #21513, #41692, #26124, #24750, #38004, #14767 ) ) ;
#8435 = AXIS2_PLACEMENT_3D ( 'NONE', #34787, #27459, #8834 ) ;
#8436 = VERTEX_POINT ( 'NONE', #41752 ) ;
#8437 = ORIENTED_EDGE ( 'NONE', *, *, #22763, .T. ) ;
#8438 = VECTOR ( 'NONE', #30259, 1000.000000000000227 ) ;
#8439 = EDGE_LOOP ( 'NONE', ( #21185, #10334, #34494, #17222 ) ) ;
#8440 = ADVANCED_FACE ( 'NONE', ( #48359 ), #22895, .T. ) ;
#8441 = LINE ( 'NONE', #19440, #19870 ) ;
#8442 = EDGE_CURVE ( 'NONE', #40828, #46432, #48301, .T. ) ;
#8443 = CARTESIAN_POINT ( 'NONE',  ( -1.499592026101402853, -119.9650177866181764, 2.500000000000000000 ) ) ;
#8444 = DIRECTION ( 'NONE',  ( -1.000000000000000000, 0.000000000000000000, -0.000000000000000000 ) ) ;
#8445 = ORIENTED_EDGE ( 'NONE', *, *, #14700, .T. ) ;
#8446 = DIRECTION ( 'NONE',  ( -1.000000000000000000, -0.000000000000000000, 0.000000000000000000 ) ) ;
#8447 = ORIENTED_EDGE ( 'NONE', *, *, #25689, .T. ) ;
#8448 = ORIENTED_EDGE ( 'NONE', *, *, #31071, .F. ) ;
#8449 = EDGE_CURVE ( 'NONE', #30139, #8092, #1431, .T. ) ;
#8450 = CARTESIAN_POINT ( 'NONE',  ( 11.99999999999999822, 68.27212725128275395, -31.46837873495001503 ) ) ;
#8451 = FACE_OUTER_BOUND ( 'NONE', #12170, .T. ) ;
#8452 = LINE ( 'NONE', #22896, #35264 ) ;
#8453 = AXIS2_PLACEMENT_3D ( 'NONE', #7820, #15422, #3910 ) ;
#8454 = ORIENTED_EDGE ( 'NONE', *, *, #25275, .F. ) ;
#8455 = ORIENTED_EDGE ( 'NONE', *, *, #28139, .F. ) ;
#8456 = FACE_OUTER_BOUND ( 'NONE', #29471, .T. ) ;
#8457 = ORIENTED_EDGE ( 'NONE', *, *, #18499, .F. ) ;
#8458 = EDGE_CURVE ( 'NONE', #17814, #14588, #626, .T. ) ;
#8459 = DIRECTION ( 'NONE',  ( 0.000000000000000000, -0.7604059656000369261, 0.6494480483301767748 ) ) ;
#8460 = CYLINDRICAL_SURFACE ( 'NONE', #2954, 31.99999999999998579 ) ;
#8461 = CARTESIAN_POINT ( 'NONE',  ( 0.000000000000000000, -37.58145647212455032, 0.6853352020789044152 ) ) ;
#8462 = DIRECTION ( 'NONE',  ( 0.000000000000000000, -0.8090169943749403458, -0.5877852522924830181 ) ) ;
#8463 = CARTESIAN_POINT ( 'NONE',  ( 10.00000000000000000, -46.11716303203136391, -67.80270845531937596 ) ) ;
#8464 = DIRECTION ( 'NONE',  ( -1.000000000000000000, 0.000000000000000000, 0.000000000000000000 ) ) ;
#8465 = CARTESIAN_POINT ( 'NONE',  ( 0.000000000000000000, 0.000000000000000000, 0.000000000000000000 ) ) ;
#8466 = VERTEX_POINT ( 'NONE', #11889 ) ;
#8467 = LINE ( 'NONE', #31243, #43874 ) ;
#8468 = DIRECTION ( 'NONE',  ( 0.000000000000000000, 0.000000000000000000, 1.000000000000000000 ) ) ;
#8469 = DIRECTION ( 'NONE',  ( -1.000000000000000000, -0.000000000000000000, 0.000000000000000000 ) ) ;
#8470 = DIRECTION ( 'NONE',  ( 0.000000000000000000, 0.000000000000000000, 1.000000000000000000 ) ) ;
#8471 = ORIENTED_EDGE ( 'NONE', *, *, #23193, .T. ) ;
#8472 = ORIENTED_EDGE ( 'NONE', *, *, #15593, .T. ) ;
#8473 = CARTESIAN_POINT ( 'NONE',  ( 12.00000000000000000, 5.835314593368470248, -22.81335362449854642 ) ) ;
#8474 = AXIS2_PLACEMENT_3D ( 'NONE', #8510, #5100, #34694 ) ;
#8475 = DIRECTION ( 'NONE',  ( -0.000000000000000000, -0.000000000000000000, -1.000000000000000000 ) ) ;
#8476 = FACE_OUTER_BOUND ( 'NONE', #36984, .T. ) ;
#8477 = LINE ( 'NONE', #12887, #14341 ) ;
#8478 = AXIS2_PLACEMENT_3D ( 'NONE', #40259, #3026, #21389 ) ;
#8479 = CARTESIAN_POINT ( 'NONE',  ( -19.27444613274700913, -101.8135840178490668, 2.500000000000000000 ) ) ;
#8480 = DIRECTION ( 'NONE',  ( 0.000000000000000000, 0.000000000000000000, 1.000000000000000000 ) ) ;
#8481 = ORIENTED_EDGE ( 'NONE', *, *, #47504, .F. ) ;
#8482 = FACE_OUTER_BOUND ( 'NONE', #5510, .T. ) ;
#8483 = DIRECTION ( 'NONE',  ( 0.000000000000000000, 0.000000000000000000, -1.000000000000000000 ) ) ;
#8484 = ORIENTED_EDGE ( 'NONE', *, *, #4372, .F. ) ;
#8485 = ORIENTED_EDGE ( 'NONE', *, *, #33686, .T. ) ;
#8486 = CARTESIAN_POINT ( 'NONE',  ( 0.000000000000000000, 16.23288003029543347, -33.80338159004267595 ) ) ;
#8487 = ORIENTED_EDGE ( 'NONE', *, *, #46423, .F. ) ;
#8488 = VECTOR ( 'NONE', #26494, 1000.000000000000000 ) ;
#8489 = VERTEX_POINT ( 'NONE', #8212 ) ;
#8490 = CARTESIAN_POINT ( 'NONE',  ( 10.00000000000000000, 10.74501242461282757, 35.92658777277515014 ) ) ;
#8491 = ORIENTED_EDGE ( 'NONE', *, *, #29950, .F. ) ;
#8492 = VECTOR ( 'NONE', #11027, 1000.000000000000000 ) ;
#8493 = EDGE_CURVE ( 'NONE', #33708, #1101, #31140, .T. ) ;
#8494 = CARTESIAN_POINT ( 'NONE',  ( 10.00000000000000000, 0.000000000000000000, 0.000000000000000000 ) ) ;
#8495 = CARTESIAN_POINT ( 'NONE',  ( 15.00000000000000000, -0.9646360437375368635, -23.52805723605589705 ) ) ;
#8496 = AXIS2_PLACEMENT_3D ( 'NONE', #39344, #32018, #5829 ) ;
#8497 = ORIENTED_EDGE ( 'NONE', *, *, #14400, .F. ) ;
#8498 = ORIENTED_EDGE ( 'NONE', *, *, #38131, .T. ) ;
#8499 = EDGE_CURVE ( 'NONE', #33124, #2120, #30737, .T. ) ;
#8500 = CIRCLE ( 'NONE', #3834, 37.49900000000000944 ) ;
#8501 = DIRECTION ( 'NONE',  ( 1.000000000000000000, -0.000000000000000000, -0.000000000000000000 ) ) ;
#8502 = LINE ( 'NONE', #6883, #21947 ) ;
#8503 = CARTESIAN_POINT ( 'NONE',  ( 50.00005079999999680, 0.000000000000000000, 21.00000000000000000 ) ) ;
#8504 = ORIENTED_EDGE ( 'NONE', *, *, #19387, .F. ) ;
#8505 = CYLINDRICAL_SURFACE ( 'NONE', #47399, 32.00000000000000000 ) ;
#8506 = ORIENTED_EDGE ( 'NONE', *, *, #31357, .F. ) ;
#8507 = EDGE_LOOP ( 'NONE', ( #45427, #40114, #25395, #28622 ) ) ;
#8508 = ADVANCED_FACE ( 'NONE', ( #37589 ), #14841, .T. ) ;
#8509 = DIRECTION ( 'NONE',  ( 0.000000000000000000, 0.7431448254773862505, -0.6691306063588671194 ) ) ;
#8510 = CARTESIAN_POINT ( 'NONE',  ( 10.00000000000000000, 10.96151621346487914, 35.95386929396260456 ) ) ;
#8511 = VERTEX_POINT ( 'NONE', #12149 ) ;
#8512 = EDGE_CURVE ( 'NONE', #33790, #39605, #26442, .T. ) ;
#8513 = DIRECTION ( 'NONE',  ( -1.000000000000000000, 0.000000000000000000, 0.000000000000000000 ) ) ;
#8514 = CARTESIAN_POINT ( 'NONE',  ( 10.00000000000000000, 8.830959090343430518, -74.65491531819107252 ) ) ;
#8515 = VERTEX_POINT ( 'NONE', #44939 ) ;
#8516 = ORIENTED_EDGE ( 'NONE', *, *, #6749, .F. ) ;
#8517 = AXIS2_PLACEMENT_3D ( 'NONE', #17378, #39690, #39442 ) ;
#8518 = DIRECTION ( 'NONE',  ( 1.000000000000000000, 0.000000000000000000, 0.000000000000000000 ) ) ;
#8519 = CARTESIAN_POINT ( 'NONE',  ( 10.00000000000000000, 0.000000000000000000, 0.000000000000000000 ) ) ;
#8520 = ORIENTED_EDGE ( 'NONE', *, *, #43101, .T. ) ;
#8521 = CARTESIAN_POINT ( 'NONE',  ( 10.00000000000000000, 39.78640506895700213, -66.50666863321957578 ) ) ;
#8522 = VERTEX_POINT ( 'NONE', #30009 ) ;
#8524 = ADVANCED_FACE ( 'NONE', ( #386 ), #33664, .T. ) ;
#8523 = LINE ( 'NONE', #38397, #19150 ) ;
#8525 = CARTESIAN_POINT ( 'NONE',  ( 17.82587367876289974, -104.6869915565625320, 2.500000000000000000 ) ) ;
#8526 = DIRECTION ( 'NONE',  ( 0.000000000000000000, -0.3090169943749349613, -0.9510565162951576390 ) ) ;
#8527 = DIRECTION ( 'NONE',  ( -1.000000000000000000, -0.000000000000000000, 0.000000000000000000 ) ) ;
#8528 = CARTESIAN_POINT ( 'NONE',  ( 15.00000000000000000, 0.000000000000000000, 0.000000000000000000 ) ) ;
#8529 = AXIS2_PLACEMENT_3D ( 'NONE', #44354, #25735, #17911 ) ;
#8530 = LINE ( 'NONE', #4626, #18450 ) ;
#8531 = CIRCLE ( 'NONE', #27311, 21.00000000000000000 ) ;
#8532 = DIRECTION ( 'NONE',  ( -1.000000000000000000, -0.000000000000000000, 0.000000000000000000 ) ) ;
#8533 = AXIS2_PLACEMENT_3D ( 'NONE', #3620, #48402, #11210 ) ;
#8534 = DIRECTION ( 'NONE',  ( 0.000000000000000000, 0.4539904997395414754, 0.8910065241883706744 ) ) ;
#8535 = CARTESIAN_POINT ( 'NONE',  ( 7.001685179585692254, -14.98378029539707512, -1.199999999999999956 ) ) ;
#8536 = ORIENTED_EDGE ( 'NONE', *, *, #15039, .T. ) ;
#8537 = EDGE_LOOP ( 'NONE', ( #33036, #45003, #26419, #37825 ) ) ;
#8538 = EDGE_CURVE ( 'NONE', #21261, #20465, #29757, .T. ) ;
#8539 = CIRCLE ( 'NONE', #39063, 77.49900000000000944 ) ;
#8540 = DIRECTION ( 'NONE',  ( 0.000000000000000000, 0.000000000000000000, -1.000000000000000000 ) ) ;
#8541 = ORIENTED_EDGE ( 'NONE', *, *, #11813, .F. ) ;
#8542 = EDGE_CURVE ( 'NONE', #31426, #29904, #38987, .T. ) ;
#8543 = FACE_OUTER_BOUND ( 'NONE', #3169, .T. ) ;
#8544 = CARTESIAN_POINT ( 'NONE',  ( 0.000000000000000000, 70.53064760720278059, 26.01480285779964774 ) ) ;
#8545 = ADVANCED_FACE ( 'NONE', ( #7728 ), #4061, .T. ) ;
#8546 = VERTEX_POINT ( 'NONE', #16049 ) ;
#8547 = CARTESIAN_POINT ( 'NONE',  ( 0.000000000000000000, 40.65526001592611749, 71.21200624218811015 ) ) ;
#8548 = ORIENTED_EDGE ( 'NONE', *, *, #42664, .T. ) ;
#8549 = ORIENTED_EDGE ( 'NONE', *, *, #7224, .T. ) ;
#8550 = ORIENTED_EDGE ( 'NONE', *, *, #33803, .F. ) ;
#8551 = ORIENTED_EDGE ( 'NONE', *, *, #26783, .F. ) ;
#8552 = EDGE_CURVE ( 'NONE', #28265, #25548, #40523, .T. ) ;
#8553 = EDGE_CURVE ( 'NONE', #22152, #18327, #34621, .T. ) ;
#8554 = EDGE_CURVE ( 'NONE', #17812, #22693, #34878, .T. ) ;
#8555 = CIRCLE ( 'NONE', #26561, 31.99999999999999289 ) ;
#8556 = DIRECTION ( 'NONE',  ( -1.000000000000000000, -0.000000000000000000, 0.000000000000000000 ) ) ;
#8557 = ORIENTED_EDGE ( 'NONE', *, *, #33912, .F. ) ;
#8558 = DIRECTION ( 'NONE',  ( -1.000000000000000000, 0.000000000000000000, 0.000000000000000000 ) ) ;
#8559 = ORIENTED_EDGE ( 'NONE', *, *, #9658, .T. ) ;
#8560 = DIRECTION ( 'NONE',  ( -1.000000000000000000, -0.000000000000000000, 0.000000000000000000 ) ) ;
#8561 = ORIENTED_EDGE ( 'NONE', *, *, #19661, .T. ) ;
#8562 = AXIS2_PLACEMENT_3D ( 'NONE', #32929, #3302, #9947 ) ;
#8563 = LINE ( 'NONE', #45794, #1967 ) ;
#8564 = DIRECTION ( 'NONE',  ( -1.000000000000000000, 0.000000000000000000, -0.000000000000000000 ) ) ;
#8565 = ORIENTED_EDGE ( 'NONE', *, *, #5310, .T. ) ;
#8566 = AXIS2_PLACEMENT_3D ( 'NONE', #11441, #22446, #15097 ) ;
#8567 = DIRECTION ( 'NONE',  ( 0.000000000000000000, 0.2079116908177532086, -0.9781476007338069101 ) ) ;
#8568 = ORIENTED_EDGE ( 'NONE', *, *, #21298, .F. ) ;
#8569 = EDGE_CURVE ( 'NONE', #24221, #45052, #25647, .T. ) ;
#8570 = DIRECTION ( 'NONE',  ( -1.000000000000000000, 0.000000000000000000, 0.000000000000000000 ) ) ;
#8571 = FACE_OUTER_BOUND ( 'NONE', #44955, .T. ) ;
#8572 = ORIENTED_EDGE ( 'NONE', *, *, #30080, .F. ) ;
#8573 = LINE ( 'NONE', #37483, #35021 ) ;
#8574 = ORIENTED_EDGE ( 'NONE', *, *, #35298, .F. ) ;
#8575 = CIRCLE ( 'NONE', #10964, 37.49900000000000233 ) ;
#8576 = EDGE_LOOP ( 'NONE', ( #47107, #22613, #2916, #19950 ) ) ;
#8577 = DIRECTION ( 'NONE',  ( -1.000000000000000000, 0.000000000000000000, 0.000000000000000000 ) ) ;
#8578 = DIRECTION ( 'NONE',  ( 0.000000000000000000, 0.7604059656000276002, 0.6494480483301876550 ) ) ;
#8579 = DIRECTION ( 'NONE',  ( 1.000000000000000000, 0.000000000000000000, 0.000000000000000000 ) ) ;
#8580 = FACE_OUTER_BOUND ( 'NONE', #44449, .T. ) ;
#8581 = CARTESIAN_POINT ( 'NONE',  ( 5.000000000000000000, 32.34446384430010113, -26.79245525562679831 ) ) ;
#8582 = PRODUCT_DEFINITION_SHAPE ( 'NONE', 'NONE',  #16707 ) ;
#8583 = DIRECTION ( 'NONE',  ( -1.000000000000000000, 0.000000000000000000, 0.000000000000000000 ) ) ;
#8584 = FACE_OUTER_BOUND ( 'NONE', #46441, .T. ) ;
#8585 = CARTESIAN_POINT ( 'NONE',  ( 11.99999999999999822, -2.956366410621191765, 75.11725578898467859 ) ) ;
#8586 = DIRECTION ( 'NONE',  ( -1.000000000000000000, 0.000000000000000000, 0.000000000000000000 ) ) ;
#8587 = DIRECTION ( 'NONE',  ( 0.000000000000000000, 0.8660254037844374864, -0.5000000000000019984 ) ) ;
#8588 = DIRECTION ( 'NONE',  ( 0.000000000000000000, 0.000000000000000000, -1.000000000000000000 ) ) ;
#8589 = DIRECTION ( 'NONE',  ( 0.000000000000000000, 0.000000000000000000, 1.000000000000000000 ) ) ;
#8590 = CARTESIAN_POINT ( 'NONE',  ( -10.00000000000000000, 0.000000000000000000, 0.000000000000000000 ) ) ;
#8591 = CARTESIAN_POINT ( 'NONE',  ( 11.99999999999999822, 0.000000000000000000, 0.000000000000000000 ) ) ;
#8592 = LINE ( 'NONE', #5192, #30373 ) ;
#8593 = ORIENTED_EDGE ( 'NONE', *, *, #41506, .F. ) ;
#8594 = ORIENTED_EDGE ( 'NONE', *, *, #43947, .F. ) ;
#8595 = AXIS2_PLACEMENT_3D ( 'NONE', #14191, #13951, #44295 ) ;
#8596 = ADVANCED_FACE ( 'NONE', ( #42957 ), #8678, .F. ) ;
#8597 = CARTESIAN_POINT ( 'NONE',  ( -3.961125083139900749, -143.2122702051246677, 5.500000000000000000 ) ) ;
#8598 = AXIS2_PLACEMENT_3D ( 'NONE', #37036, #65, #15017 ) ;
#8599 = ORIENTED_EDGE ( 'NONE', *, *, #39703, .F. ) ;
#8600 = DIRECTION ( 'NONE',  ( -1.000000000000000000, -0.000000000000000000, 0.000000000000000000 ) ) ;
#8602 = EDGE_CURVE ( 'NONE', #1613, #5563, #16771, .T. ) ;
#8601 = CIRCLE ( 'NONE', #42123, 42.00000000000000000 ) ;
#8603 = DIRECTION ( 'NONE',  ( -1.000000000000000000, -0.000000000000000000, 0.000000000000000000 ) ) ;
#8604 = ADVANCED_FACE ( 'NONE', ( #20419 ), #38816, .T. ) ;
#8605 = ORIENTED_EDGE ( 'NONE', *, *, #29405, .F. ) ;
#8606 = AXIS2_PLACEMENT_3D ( 'NONE', #36094, #28522, #17733 ) ;
#8607 = VECTOR ( 'NONE', #6839, 1000.000000000000000 ) ;
#8608 = DIRECTION ( 'NONE',  ( -1.000000000000000000, -0.000000000000000000, -0.000000000000000000 ) ) ;
#8609 = ORIENTED_EDGE ( 'NONE', *, *, #13421, .T. ) ;
#8610 = EDGE_CURVE ( 'NONE', #31655, #11482, #12613, .T. ) ;
#8611 = EDGE_CURVE ( 'NONE', #2989, #19224, #19395, .T. ) ;
#8612 = FACE_OUTER_BOUND ( 'NONE', #34990, .T. ) ;
#8613 = ORIENTED_EDGE ( 'NONE', *, *, #39477, .T. ) ;
#8614 = CARTESIAN_POINT ( 'NONE',  ( 10.00000000000000000, 68.27212725128275395, -31.46837873495001503 ) ) ;
#8615 = EDGE_LOOP ( 'NONE', ( #26794, #37995, #18231, #35165 ) ) ;
#8617 = ORIENTED_EDGE ( 'NONE', *, *, #8979, .F. ) ;
#8616 = LINE ( 'NONE', #792, #27001 ) ;
#8618 = VERTEX_POINT ( 'NONE', #12860 ) ;
#8619 = DIRECTION ( 'NONE',  ( -1.000000000000000000, 0.000000000000000000, 0.000000000000000000 ) ) ;
#8620 = DIRECTION ( 'NONE',  ( 0.000000000000000000, 0.2334453638558990907, 0.9723699203976781114 ) ) ;
#8621 = CARTESIAN_POINT ( 'NONE',  ( 10.00000000000000000, 38.55633173627010990, 16.65560815589424593 ) ) ;
#8622 = EDGE_CURVE ( 'NONE', #13463, #15338, #23376, .T. ) ;
#8623 = AXIS2_PLACEMENT_3D ( 'NONE', #27064, #8446, #30987 ) ;
#8624 = DIRECTION ( 'NONE',  ( 0.000000000000000000, 0.000000000000000000, -1.000000000000000000 ) ) ;
#8625 = EDGE_LOOP ( 'NONE', ( #17114, #16348, #18367, #8816 ) ) ;
#8626 = AXIS2_PLACEMENT_3D ( 'NONE', #30660, #15980, #8387 ) ;
#8627 = CARTESIAN_POINT ( 'NONE',  ( 15.00000000000000000, -1.278221433540145391, 26.51162292216073979 ) ) ;
#8628 = ORIENTED_EDGE ( 'NONE', *, *, #2405, .F. ) ;
#8629 = EDGE_LOOP ( 'NONE', ( #33098, #26635, #46131, #20117 ) ) ;
#8630 = CYLINDRICAL_SURFACE ( 'NONE', #43473, 77.49899999999999523 ) ;
#8631 = AXIS2_PLACEMENT_3D ( 'NONE', #17240, #32660, #25309 ) ;
#8632 = ORIENTED_EDGE ( 'NONE', *, *, #47009, .F. ) ;
#8633 = CIRCLE ( 'NONE', #35995, 31.99999999999998579 ) ;
#8634 = DIRECTION ( 'NONE',  ( -1.000000000000000000, -0.000000000000000000, 0.000000000000000000 ) ) ;
#8635 = CARTESIAN_POINT ( 'NONE',  ( 11.99999999999999822, 0.000000000000000000, 0.000000000000000000 ) ) ;
#8636 = CARTESIAN_POINT ( 'NONE',  ( 10.00000000000000000, 0.000000000000000000, 0.000000000000000000 ) ) ;
#8637 = VERTEX_POINT ( 'NONE', #39273 ) ;
#8638 = LINE ( 'NONE', #12103, #25285 ) ;
#8639 = PLANE ( 'NONE',  #30739 ) ;
#8640 = AXIS2_PLACEMENT_3D ( 'NONE', #11049, #22316, #25720 ) ;
#8641 = CARTESIAN_POINT ( 'NONE',  ( 10.00000000000000000, -14.66109333815513160, 73.73191006444567108 ) ) ;
#8642 = VECTOR ( 'NONE', #39731, 1000.000000000000000 ) ;
#8643 = DIRECTION ( 'NONE',  ( 0.000000000000000000, -0.5877852522924803536, 0.8090169943749422332 ) ) ;
#8644 = DIRECTION ( 'NONE',  ( -1.000000000000000000, -0.000000000000000000, 0.000000000000000000 ) ) ;
#8645 = DIRECTION ( 'NONE',  ( 0.000000000000000000, -0.9945218953682730678, 0.1045284632676569680 ) ) ;
#8646 = LINE ( 'NONE', #1804, #10732 ) ;
#8647 = DIRECTION ( 'NONE',  ( -1.000000000000000000, -0.000000000000000000, 0.000000000000000000 ) ) ;
#8648 = LINE ( 'NONE', #37800, #26858 ) ;
#8649 = ORIENTED_EDGE ( 'NONE', *, *, #1281, .F. ) ;
#8650 = ORIENTED_EDGE ( 'NONE', *, *, #38413, .T. ) ;
#8651 = FACE_OUTER_BOUND ( 'NONE', #35846, .T. ) ;
#8652 = ORIENTED_EDGE ( 'NONE', *, *, #915, .F. ) ;
#8653 = VERTEX_POINT ( 'NONE', #38312 ) ;
#8654 = PLANE ( 'NONE',  #34680 ) ;
#8655 = EDGE_CURVE ( 'NONE', #1692, #9518, #36632, .T. ) ;
#8656 = CARTESIAN_POINT ( 'NONE',  ( 10.00000000000000000, 30.00120703465205452, 22.64427369931179967 ) ) ;
#8657 = EDGE_CURVE ( 'NONE', #39152, #40727, #7705, .T. ) ;
#8658 = ORIENTED_EDGE ( 'NONE', *, *, #42899, .T. ) ;
#8659 = AXIS2_PLACEMENT_3D ( 'NONE', #7455, #37312, #3774 ) ;
#8660 = AXIS2_PLACEMENT_3D ( 'NONE', #9233, #43015, #35414 ) ;
#8661 = ADVANCED_FACE ( 'NONE', ( #45910 ), #19944, .F. ) ;
#8662 = ORIENTED_EDGE ( 'NONE', *, *, #23365, .F. ) ;
#8663 = CIRCLE ( 'NONE', #6314, 31.99999999999998934 ) ;
#8664 = VECTOR ( 'NONE', #11703, 1000.000000000000114 ) ;
#8665 = ORIENTED_EDGE ( 'NONE', *, *, #46582, .T. ) ;
#8666 = ORIENTED_EDGE ( 'NONE', *, *, #645, .F. ) ;
#8667 = EDGE_LOOP ( 'NONE', ( #18612, #30705, #2496, #38149 ) ) ;
#8668 = EDGE_CURVE ( 'NONE', #45189, #29506, #8932, .T. ) ;
#8669 = AXIS2_PLACEMENT_3D ( 'NONE', #31610, #13005, #16193 ) ;
#8670 = CARTESIAN_POINT ( 'NONE',  ( 11.99999999999999822, 0.000000000000000000, 0.000000000000000000 ) ) ;
#8671 = EDGE_CURVE ( 'NONE', #28806, #27309, #35059, .T. ) ;
#8672 = DIRECTION ( 'NONE',  ( -0.000000000000000000, -1.156482317317870936E-15, -1.000000000000000000 ) ) ;
#8673 = CARTESIAN_POINT ( 'NONE',  ( 5.999999999999999112, -60.67117009219097667, -55.16347631943106933 ) ) ;
#8674 = ORIENTED_EDGE ( 'NONE', *, *, #11932, .T. ) ;
#8675 = DIRECTION ( 'NONE',  ( 0.000000000000000000, 0.000000000000000000, -1.000000000000000000 ) ) ;
#8676 = ORIENTED_EDGE ( 'NONE', *, *, #5110, .F. ) ;
#8677 = EDGE_LOOP ( 'NONE', ( #10822, #36712, #25684, #32910 ) ) ;
#8678 = PLANE ( 'NONE',  #13200 ) ;
#8679 = CARTESIAN_POINT ( 'NONE',  ( 6.719258119307965238, -15.35072898742050107, -1.199999999999999956 ) ) ;
#8680 = DIRECTION ( 'NONE',  ( 0.000000000000000000, 0.000000000000000000, 1.000000000000000000 ) ) ;
#8681 = EDGE_CURVE ( 'NONE', #12258, #441, #34285, .T. ) ;
#8682 = ORIENTED_EDGE ( 'NONE', *, *, #38710, .T. ) ;
#8683 = ORIENTED_EDGE ( 'NONE', *, *, #1619, .T. ) ;
#8684 = EDGE_LOOP ( 'NONE', ( #14838, #17866, #3385, #2259 ) ) ;
#8685 = DIRECTION ( 'NONE',  ( -1.000000000000000000, -0.000000000000000000, 0.000000000000000000 ) ) ;
#8686 = ORIENTED_EDGE ( 'NONE', *, *, #42994, .F. ) ;
#8687 = CARTESIAN_POINT ( 'NONE',  ( 10.00000000000000000, -16.45098606841102651, -33.79645857604531045 ) ) ;
#8688 = DIRECTION ( 'NONE',  ( -1.000000000000000000, 0.000000000000000000, 0.000000000000000000 ) ) ;
#8689 = CYLINDRICAL_SURFACE ( 'NONE', #40093, 16.00000000000000000 ) ;
#8690 = DIRECTION ( 'NONE',  ( -1.000000000000000000, 0.000000000000000000, 0.000000000000000000 ) ) ;
#8691 = CARTESIAN_POINT ( 'NONE',  ( 11.59999999999999787, 1.420590287010929336E-15, -54.99999999999998579 ) ) ;
#8692 = CYLINDRICAL_SURFACE ( 'NONE', #22156, 82.00000000000000000 ) ;
#8693 = CARTESIAN_POINT ( 'NONE',  ( 20.07203437053270179, -132.2214334768125354, 2.500000000000000000 ) ) ;
#8694 = CARTESIAN_POINT ( 'NONE',  ( 0.000000000000000000, 77.49459641780886443, -0.8261519478433960728 ) ) ;
#8695 = DIRECTION ( 'NONE',  ( -1.000000000000000000, 0.000000000000000000, 0.000000000000000000 ) ) ;
#8696 = CIRCLE ( 'NONE', #34477, 42.00000000000000000 ) ;
#8697 = EDGE_CURVE ( 'NONE', #32725, #7093, #2085, .T. ) ;
#8698 = CARTESIAN_POINT ( 'NONE',  ( 10.00000000000000000, 0.000000000000000000, 0.000000000000000000 ) ) ;
#8699 = DIRECTION ( 'NONE',  ( 1.000000000000000000, 0.000000000000000000, 0.000000000000000000 ) ) ;
#8700 = ORIENTED_EDGE ( 'NONE', *, *, #16027, .F. ) ;
#8701 = VERTEX_POINT ( 'NONE', #41998 ) ;
#8702 = AXIS2_PLACEMENT_3D ( 'NONE', #31958, #46873, #42723 ) ;
#8703 =( NAMED_UNIT ( * ) SI_UNIT ( $, .STERADIAN. ) SOLID_ANGLE_UNIT ( ) );
#8704 = CIRCLE ( 'NONE', #20402, 77.49899999999999523 ) ;
#8705 = AXIS2_PLACEMENT_3D ( 'NONE', #7730, #22657, #389 ) ;
#8706 = DIRECTION ( 'NONE',  ( -1.000000000000000000, 0.000000000000000000, 0.000000000000000000 ) ) ;
#8707 = CARTESIAN_POINT ( 'NONE',  ( 11.99999999999999822, 31.47745569255140552, 68.26794271651274926 ) ) ;
#8708 = CARTESIAN_POINT ( 'NONE',  ( 0.000000000000000000, -59.03961581697432592, 46.53671651293927880 ) ) ;
#8709 = CIRCLE ( 'NONE', #46250, 37.49900000000000233 ) ;
#8710 = FILL_AREA_STYLE_COLOUR ( '', #46663 ) ;
#8711 = DIRECTION ( 'NONE',  ( -1.000000000000000000, 0.000000000000000000, -0.000000000000000000 ) ) ;
#8712 = CYLINDRICAL_SURFACE ( 'NONE', #23201, 31.99999999999998579 ) ;
#8713 = DIRECTION ( 'NONE',  ( 0.000000000000000000, 0.000000000000000000, 1.000000000000000000 ) ) ;
#8714 = ORIENTED_EDGE ( 'NONE', *, *, #34854, .T. ) ;
#8715 = VECTOR ( 'NONE', #44168, 1000.000000000000000 ) ;
#8716 = EDGE_CURVE ( 'NONE', #20085, #29267, #29575, .T. ) ;
#8717 = AXIS2_PLACEMENT_3D ( 'NONE', #44566, #21323, #25477 ) ;
#8718 = ADVANCED_FACE ( 'NONE', ( #21146 ), #14291, .T. ) ;
#8719 = ORIENTED_EDGE ( 'NONE', *, *, #281, .T. ) ;
#8720 =( NAMED_UNIT ( * ) PLANE_ANGLE_UNIT ( ) SI_UNIT ( $, .RADIAN. ) );
#8721 = DIRECTION ( 'NONE',  ( 0.000000000000000000, 0.000000000000000000, 1.000000000000000000 ) ) ;
#8722 = VERTEX_POINT ( 'NONE', #40491 ) ;
#8723 = EDGE_CURVE ( 'NONE', #13379, #46560, #15536, .T. ) ;
#8724 = ORIENTED_EDGE ( 'NONE', *, *, #9608, .T. ) ;
#8725 = VERTEX_POINT ( 'NONE', #44158 ) ;
#8726 = ADVANCED_FACE ( 'NONE', ( #2539 ), #35841, .T. ) ;
#8727 = ORIENTED_EDGE ( 'NONE', *, *, #19769, .F. ) ;
#8728 = FACE_OUTER_BOUND ( 'NONE', #11576, .T. ) ;
#8729 = ORIENTED_EDGE ( 'NONE', *, *, #15155, .F. ) ;
#8730 = AXIS2_PLACEMENT_3D ( 'NONE', #2872, #40342, #10714 ) ;
#8731 = AXIS2_PLACEMENT_3D ( 'NONE', #8872, #13050, #16711 ) ;
#8732 = CARTESIAN_POINT ( 'NONE',  ( -3.000000000000000000, 20.85821328998741109, 10.92862929874522315 ) ) ;
#8733 = CIRCLE ( 'NONE', #47043, 16.00000000000000000 ) ;
#8734 = CARTESIAN_POINT ( 'NONE',  ( 0.000000000000000000, 0.000000000000000000, 0.000000000000000000 ) ) ;
#8735 = ORIENTED_EDGE ( 'NONE', *, *, #25170, .T. ) ;
#8736 = EDGE_LOOP ( 'NONE', ( #15542, #21317, #6633, #23146 ) ) ;
#8737 = CIRCLE ( 'NONE', #19669, 77.49899999999999523 ) ;
#8738 = AXIS2_PLACEMENT_3D ( 'NONE', #16542, #39789, #20441 ) ;
#8739 = CARTESIAN_POINT ( 'NONE',  ( 4.999999999999999112, -41.91543099594819921, 2.663952781846001816 ) ) ;
#8741 = ORIENTED_EDGE ( 'NONE', *, *, #25087, .F. ) ;
#8740 = CARTESIAN_POINT ( 'NONE',  ( 6.000000000000000000, -39.47590169984795239, -71.87247863392455827 ) ) ;
#8742 = EDGE_CURVE ( 'NONE', #38437, #34100, #16314, .T. ) ;
#8743 = FACE_OUTER_BOUND ( 'NONE', #12669, .T. ) ;
#8744 = ORIENTED_EDGE ( 'NONE', *, *, #20169, .T. ) ;
#8745 = ORIENTED_EDGE ( 'NONE', *, *, #33379, .T. ) ;
#8746 = LINE ( 'NONE', #34211, #34881 ) ;
#8747 = ORIENTED_EDGE ( 'NONE', *, *, #6304, .F. ) ;
#8748 = EDGE_LOOP ( 'NONE', ( #32969, #11818, #13023, #728 ) ) ;
#8749 = CARTESIAN_POINT ( 'NONE',  ( 6.000000000000000000, 80.28980883073758434, 16.65972982744962749 ) ) ;
#8750 = FACE_OUTER_BOUND ( 'NONE', #18319, .T. ) ;
#8751 = VECTOR ( 'NONE', #21262, 1000.000000000000000 ) ;
#8752 = ORIENTED_EDGE ( 'NONE', *, *, #7897, .F. ) ;
#8753 = DIRECTION ( 'NONE',  ( -1.000000000000000000, 0.000000000000000000, 0.000000000000000000 ) ) ;
#8754 = CARTESIAN_POINT ( 'NONE',  ( -42.50000000000000000, 1.702802944658382841E-15, 13.90444123027096879 ) ) ;
#8755 = DIRECTION ( 'NONE',  ( 1.000000000000000000, 0.000000000000000000, 0.000000000000000000 ) ) ;
#8756 = ORIENTED_EDGE ( 'NONE', *, *, #43118, .T. ) ;
#8757 = ORIENTED_EDGE ( 'NONE', *, *, #8776, .T. ) ;
#8758 = CARTESIAN_POINT ( 'NONE',  ( -10.00000000000000000, 0.000000000000000000, 0.000000000000000000 ) ) ;
#8759 = EDGE_CURVE ( 'NONE', #4600, #11933, #6948, .T. ) ;
#8760 = DIRECTION ( 'NONE',  ( 1.000000000000000000, -0.000000000000000000, 0.000000000000000000 ) ) ;
#8761 = ORIENTED_EDGE ( 'NONE', *, *, #40944, .T. ) ;
#8762 = CARTESIAN_POINT ( 'NONE',  ( 15.00000000000000000, -23.29833615347104470, 3.418703333116808629 ) ) ;
#8763 = ORIENTED_EDGE ( 'NONE', *, *, #35644, .T. ) ;
#8764 = CYLINDRICAL_SURFACE ( 'NONE', #13679, 82.00000000000000000 ) ;
#8765 = LINE ( 'NONE', #23702, #23191 ) ;
#8766 = CARTESIAN_POINT ( 'NONE',  ( -20.62008904684763166, -131.2721749321093512, -2.500000000000000000 ) ) ;
#8767 = CARTESIAN_POINT ( 'NONE',  ( 14.59956846177685996, -138.4757300459248484, 5.500000000000000000 ) ) ;
#8768 = DIRECTION ( 'NONE',  ( 0.000000000000000000, 0.000000000000000000, 1.000000000000000000 ) ) ;
#8770 = AXIS2_PLACEMENT_3D ( 'NONE', #28536, #2332, #28997 ) ;
#8769 = CARTESIAN_POINT ( 'NONE',  ( 10.00000000000000000, 30.80686688397010542, 21.53537804866092387 ) ) ;
#8771 = DIRECTION ( 'NONE',  ( 1.000000000000000000, 0.000000000000000000, 0.000000000000000000 ) ) ;
#8772 = CARTESIAN_POINT ( 'NONE',  ( -10.00000000000000000, 0.000000000000000000, 0.000000000000000000 ) ) ;
#8773 = EDGE_CURVE ( 'NONE', #32853, #24228, #36561, .T. ) ;
#8774 = CIRCLE ( 'NONE', #36129, 16.00000000000000355 ) ;
#8775 = CARTESIAN_POINT ( 'NONE',  ( 5.000000000000000000, -55.16347631943085617, 60.67117009219118273 ) ) ;
#8776 = EDGE_CURVE ( 'NONE', #46691, #36404, #6715, .T. ) ;
#8777 = CIRCLE ( 'NONE', #44733, 31.99999999999999289 ) ;
#8778 = ORIENTED_EDGE ( 'NONE', *, *, #19428, .T. ) ;
#8779 = CARTESIAN_POINT ( 'NONE',  ( 5.000000000000002665, 16.65972982745046238, -80.28980883073738539 ) ) ;
#8780 = EDGE_CURVE ( 'NONE', #35445, #36858, #10136, .T. ) ;
#8781 = ORIENTED_EDGE ( 'NONE', *, *, #23769, .T. ) ;
#8782 = VECTOR ( 'NONE', #10169, 1000.000000000000000 ) ;
#8783 = EDGE_CURVE ( 'NONE', #17824, #18426, #27245, .T. ) ;
#8784 = DIRECTION ( 'NONE',  ( 0.000000000000000000, 0.000000000000000000, 1.000000000000000000 ) ) ;
#8785 = DIRECTION ( 'NONE',  ( -1.000000000000000000, 0.000000000000000000, -0.000000000000000000 ) ) ;
#8786 = ORIENTED_EDGE ( 'NONE', *, *, #11684, .F. ) ;
#8787 = CARTESIAN_POINT ( 'NONE',  ( 0.000000000000000000, -23.29833615347104825, -3.418703333116803744 ) ) ;
#8788 = VECTOR ( 'NONE', #12748, 1000.000000000000000 ) ;
#8789 = EDGE_LOOP ( 'NONE', ( #16135, #43135, #14463, #5895 ) ) ;
#8790 = VERTEX_POINT ( 'NONE', #47356 ) ;
#8791 = ORIENTED_EDGE ( 'NONE', *, *, #18676, .F. ) ;
#8792 = VERTEX_POINT ( 'NONE', #43909 ) ;
#8793 = CIRCLE ( 'NONE', #38547, 16.00000000000000000 ) ;
#8794 = AXIS2_PLACEMENT_3D ( 'NONE', #32156, #43643, #10109 ) ;
#8795 = VECTOR ( 'NONE', #42481, 1000.000000000000000 ) ;
#8796 = DIRECTION ( 'NONE',  ( 0.000000000000000000, -0.4539904997395350916, -0.8910065241883738940 ) ) ;
#8797 = ORIENTED_EDGE ( 'NONE', *, *, #47722, .F. ) ;
#8798 = ORIENTED_EDGE ( 'NONE', *, *, #13609, .F. ) ;
#8799 = DIRECTION ( 'NONE',  ( -1.000000000000000000, -0.000000000000000000, -0.000000000000000000 ) ) ;
#8800 = ORIENTED_EDGE ( 'NONE', *, *, #45976, .F. ) ;
#8801 = CARTESIAN_POINT ( 'NONE',  ( 0.000000000000000000, -10.74501242461258244, -35.92658777277521409 ) ) ;
#8802 = AXIS2_PLACEMENT_3D ( 'NONE', #8028, #15621, #11485 ) ;
#8803 = AXIS2_PLACEMENT_3D ( 'NONE', #8283, #19043, #33976 ) ;
#8804 = CARTESIAN_POINT ( 'NONE',  ( 11.99999999999999822, 0.000000000000000000, 0.000000000000000000 ) ) ;
#8805 = DIRECTION ( 'NONE',  ( 0.000000000000000000, 0.000000000000000000, 1.000000000000000000 ) ) ;
#8806 = VECTOR ( 'NONE', #43994, 1000.000000000000114 ) ;
#8807 = ORIENTED_EDGE ( 'NONE', *, *, #7261, .T. ) ;
#8808 = CARTESIAN_POINT ( 'NONE',  ( -7.469491406282116941, 4.756046723998916370, -55.00000000000000000 ) ) ;
#8809 = ORIENTED_EDGE ( 'NONE', *, *, #21298, .T. ) ;
#8810 = CYLINDRICAL_SURFACE ( 'NONE', #40696, 37.49900000000000233 ) ;
#8811 = FACE_OUTER_BOUND ( 'NONE', #11633, .T. ) ;
#8812 = VERTEX_POINT ( 'NONE', #25057 ) ;
#8813 = AXIS2_PLACEMENT_3D ( 'NONE', #22130, #18462, #7686 ) ;
#8814 = CARTESIAN_POINT ( 'NONE',  ( 5.000000000000000000, -27.75498641678720446, -31.52238457039628727 ) ) ;
#8815 = ORIENTED_EDGE ( 'NONE', *, *, #44001, .T. ) ;
#8816 = ORIENTED_EDGE ( 'NONE', *, *, #27008, .T. ) ;
#8817 = DIRECTION ( 'NONE',  ( -1.000000000000000000, -0.000000000000000000, 0.000000000000000000 ) ) ;
#8818 = CARTESIAN_POINT ( 'NONE',  ( -3.000000000000000000, -10.45096189432344147, 21.10159698893426494 ) ) ;
#8819 = AXIS2_PLACEMENT_3D ( 'NONE', #19921, #31937, #13080 ) ;
#8820 = EDGE_CURVE ( 'NONE', #25146, #44798, #39774, .T. ) ;
#8821 = CARTESIAN_POINT ( 'NONE',  ( 11.99999999999999822, -36.72794159290288718, 65.59268652807197952 ) ) ;
#8822 = LINE ( 'NONE', #41900, #18037 ) ;
#8823 = FACE_OUTER_BOUND ( 'NONE', #1033, .T. ) ;
#8824 = EDGE_CURVE ( 'NONE', #18965, #16392, #13166, .T. ) ;
#8825 = DIRECTION ( 'NONE',  ( 0.000000000000000000, 0.000000000000000000, 1.000000000000000000 ) ) ;
#8826 = DIRECTION ( 'NONE',  ( 0.000000000000000000, 0.000000000000000000, 1.000000000000000000 ) ) ;
#8827 = CARTESIAN_POINT ( 'NONE',  ( 10.00000000000000000, 73.72996012237440766, 14.67089635893739619 ) ) ;
#8828 = ORIENTED_EDGE ( 'NONE', *, *, #5434, .T. ) ;
#8829 = CYLINDRICAL_SURFACE ( 'NONE', #30981, 82.00000000000000000 ) ;
#8830 = CARTESIAN_POINT ( 'NONE',  ( -0.7195005275814509993, -118.6838241033926948, -2.500000000000000000 ) ) ;
#8831 = CYLINDRICAL_SURFACE ( 'NONE', #31016, 16.00000000000000000 ) ;
#8832 = CARTESIAN_POINT ( 'NONE',  ( 0.000000000000000000, 0.000000000000000000, 42.00000000000001421 ) ) ;
#8833 = FACE_OUTER_BOUND ( 'NONE', #34894, .T. ) ;
#8835 = AXIS2_PLACEMENT_3D ( 'NONE', #19078, #3174, #18105 ) ;
#8834 = DIRECTION ( 'NONE',  ( 0.000000000000000000, -0.3826834323650969427, 0.9238795325112838519 ) ) ;
#8836 = ADVANCED_FACE ( 'NONE', ( #32648 ), #28974, .F. ) ;
#8837 = CARTESIAN_POINT ( 'NONE',  ( 0.000000000000000000, -2.956366410621191765, 75.11725578898467859 ) ) ;
#8838 = ADVANCED_FACE ( 'NONE', ( #18187 ), #25295, .F. ) ;
#8839 = ORIENTED_EDGE ( 'NONE', *, *, #12073, .F. ) ;
#8840 = ADVANCED_FACE ( 'NONE', ( #21641 ), #13571, .T. ) ;
#8841 = CIRCLE ( 'NONE', #27615, 31.99999999999999289 ) ;
#8842 = EDGE_LOOP ( 'NONE', ( #5259, #18747, #10996, #32828 ) ) ;
#8843 = CARTESIAN_POINT ( 'NONE',  ( 15.00000000000000000, -18.13022148937263012, -15.02647892043543898 ) ) ;
#8844 = ORIENTED_EDGE ( 'NONE', *, *, #32751, .T. ) ;
#8845 = CARTESIAN_POINT ( 'NONE',  ( 15.00000000000000000, 22.07842321921480888, -8.187992925817425771 ) ) ;
#8846 = CIRCLE ( 'NONE', #23698, 31.99999999999998579 ) ;
#8847 = CIRCLE ( 'NONE', #21356, 37.49900000000001654 ) ;
#8848 = SHAPE_DEFINITION_REPRESENTATION ( #32384, #1226 ) ;
#8849 = VECTOR ( 'NONE', #4555, 1000.000000000000114 ) ;
#8850 = ADVANCED_FACE ( 'NONE', ( #9647 ), #6007, .T. ) ;
#8851 = DIRECTION ( 'NONE',  ( 1.000000000000000000, 0.000000000000000000, 0.000000000000000000 ) ) ;
#8852 = AXIS2_PLACEMENT_3D ( 'NONE', #12406, #9929, #42983 ) ;
#8853 = ORIENTED_EDGE ( 'NONE', *, *, #42836, .F. ) ;
#8854 = AXIS2_PLACEMENT_3D ( 'NONE', #17708, #16753, #6223 ) ;
#8855 = CIRCLE ( 'NONE', #29195, 42.00000000000000000 ) ;
#8856 = AXIS2_PLACEMENT_3D ( 'NONE', #2771, #17704, #21849 ) ;
#8857 = DIRECTION ( 'NONE',  ( -1.000000000000000000, -0.000000000000000000, -0.000000000000000000 ) ) ;
#8858 = VERTEX_POINT ( 'NONE', #25773 ) ;
#8859 = CARTESIAN_POINT ( 'NONE',  ( 11.99999999999999822, -72.35432306680498016, 20.40083707022857951 ) ) ;
#8860 = AXIS2_PLACEMENT_3D ( 'NONE', #42091, #3915, #18830 ) ;
#8861 = CARTESIAN_POINT ( 'NONE',  ( 0.000000000000000000, -73.95703589263990807, 23.16143007188399139 ) ) ;
#8862 = LINE ( 'NONE', #1533, #3968 ) ;
#8863 = ORIENTED_EDGE ( 'NONE', *, *, #36353, .T. ) ;
#8865 = ORIENTED_EDGE ( 'NONE', *, *, #25043, .F. ) ;
#8864 = CARTESIAN_POINT ( 'NONE',  ( -23.30023580412278505, -123.4057321492263384, 5.500000000000000000 ) ) ;
#8866 = ORIENTED_EDGE ( 'NONE', *, *, #23542, .F. ) ;
#8867 = EDGE_LOOP ( 'NONE', ( #13546, #6420, #7772, #260 ) ) ;
#8868 = DIRECTION ( 'NONE',  ( -0.7950889364178796992, 0.6064928550163510845, 0.000000000000000000 ) ) ;
#8869 = DIRECTION ( 'NONE',  ( 1.000000000000000000, -0.000000000000000000, -0.000000000000000000 ) ) ;
#8870 = DIRECTION ( 'NONE',  ( -1.000000000000000000, 0.000000000000000000, 0.000000000000000000 ) ) ;
#8871 = EDGE_CURVE ( 'NONE', #22698, #3669, #6145, .T. ) ;
#8872 = CARTESIAN_POINT ( 'NONE',  ( 15.00000000000000000, 8.688484142253932063, -21.88630264137371029 ) ) ;
#8873 = AXIS2_PLACEMENT_3D ( 'NONE', #15649, #15420, #19534 ) ;
#8874 = CARTESIAN_POINT ( 'NONE',  ( 0.000000000000000000, 20.40083707022882820, 72.35432306680490910 ) ) ;
#8875 = ADVANCED_FACE ( 'NONE', ( #15274 ), #23085, .T. ) ;
#8876 = ORIENTED_EDGE ( 'NONE', *, *, #35276, .F. ) ;
#8877 = DIRECTION ( 'NONE',  ( 0.000000000000000000, 0.000000000000000000, -1.000000000000000000 ) ) ;
#8878 = VERTEX_POINT ( 'NONE', #8153 ) ;
#8879 = VERTEX_POINT ( 'NONE', #26520 ) ;
#8880 = VECTOR ( 'NONE', #38774, 1000.000000000000000 ) ;
#8881 = CARTESIAN_POINT ( 'NONE',  ( 11.99999999999999822, 36.72794159290241822, 65.59268652807223532 ) ) ;
#8882 = AXIS2_PLACEMENT_3D ( 'NONE', #40332, #14125, #18020 ) ;
#8883 = VECTOR ( 'NONE', #41544, 1000.000000000000114 ) ;
#8884 = ADVANCED_FACE ( 'NONE', ( #3757 ), #33607, .T. ) ;
#8885 = DIRECTION ( 'NONE',  ( 0.000000000000000000, 1.000000000000000000, 3.469446951953614189E-15 ) ) ;
#8886 = FACE_OUTER_BOUND ( 'NONE', #6456, .T. ) ;
#8887 = DIRECTION ( 'NONE',  ( -1.000000000000000000, -0.000000000000000000, 0.000000000000000000 ) ) ;
#8888 = VERTEX_POINT ( 'NONE', #33381 ) ;
#8889 = FACE_OUTER_BOUND ( 'NONE', #19207, .T. ) ;
#8890 = ADVANCED_FACE ( 'NONE', ( #19396 ), #30203, .T. ) ;
#8891 = CYLINDRICAL_SURFACE ( 'NONE', #29143, 31.99999999999998579 ) ;
#8892 = FACE_OUTER_BOUND ( 'NONE', #25756, .T. ) ;
#8893 = DIRECTION ( 'NONE',  ( 0.000000000000000000, 0.000000000000000000, 1.000000000000000000 ) ) ;
#8894 = LINE ( 'NONE', #27032, #34050 ) ;
#8895 = AXIS2_PLACEMENT_3D ( 'NONE', #39459, #5933, #24986 ) ;
#8896 = DIRECTION ( 'NONE',  ( 0.000000000000000000, 0.000000000000000000, 1.000000000000000000 ) ) ;
#8897 = CARTESIAN_POINT ( 'NONE',  ( 0.000000000000000000, 5.256550761632864166, 77.32052557432842832 ) ) ;
#8898 = CARTESIAN_POINT ( 'NONE',  ( 15.00000000000000000, 14.60985201121703980, -18.46759930825707841 ) ) ;
#8899 = CIRCLE ( 'NONE', #13579, 82.00000000000000000 ) ;
#8900 = AXIS2_PLACEMENT_3D ( 'NONE', #13256, #9103, #2014 ) ;
#8901 = FACE_OUTER_BOUND ( 'NONE', #34835, .T. ) ;
#8902 = DIRECTION ( 'NONE',  ( -0.5687579148473752566, 0.8225049752423786442, 0.000000000000000000 ) ) ;
#8903 = CIRCLE ( 'NONE', #4996, 82.00000000000000000 ) ;
#8904 = ADVANCED_FACE ( 'NONE', ( #15023 ), #26756, .T. ) ;
#8905 = ORIENTED_EDGE ( 'NONE', *, *, #4342, .F. ) ;
#8906 = EDGE_CURVE ( 'NONE', #10059, #38187, #37857, .T. ) ;
#8907 = CARTESIAN_POINT ( 'NONE',  ( 26.09152095774781799, -124.8716048804687375, 5.500000000000000000 ) ) ;
#8908 = VERTEX_POINT ( 'NONE', #18678 ) ;
#8909 = DIRECTION ( 'NONE',  ( -1.000000000000000000, 0.000000000000000000, -0.000000000000000000 ) ) ;
#8910 = CYLINDRICAL_SURFACE ( 'NONE', #33835, 16.00000000000000000 ) ;
#8911 = ORIENTED_EDGE ( 'NONE', *, *, #9427, .T. ) ;
#8912 = VECTOR ( 'NONE', #42698, 1000.000000000000114 ) ;
#8913 = EDGE_CURVE ( 'NONE', #39232, #24980, #5056, .T. ) ;
#8914 = CIRCLE ( 'NONE', #47969, 31.99999999999998224 ) ;
#8915 = AXIS2_PLACEMENT_3D ( 'NONE', #37427, #30335, #48431 ) ;
#8916 = AXIS2_PLACEMENT_3D ( 'NONE', #31499, #6267, #24142 ) ;
#8917 = ORIENTED_EDGE ( 'NONE', *, *, #44607, .T. ) ;
#8918 = ORIENTED_EDGE ( 'NONE', *, *, #4588, .F. ) ;
#8919 = ORIENTED_EDGE ( 'NONE', *, *, #23422, .F. ) ;
#8920 = AXIS2_PLACEMENT_3D ( 'NONE', #30043, #44000, #14872 ) ;
#8921 = CIRCLE ( 'NONE', #1092, 31.99999999999998579 ) ;
#8922 = CARTESIAN_POINT ( 'NONE',  ( 15.00000000000000000, -1.278221433540507546, -26.51162292216071492 ) ) ;
#8923 = CARTESIAN_POINT ( 'NONE',  ( -26.29030328629083968, -123.6496510949466341, 5.500000000000000000 ) ) ;
#8924 = CIRCLE ( 'NONE', #12098, 11.59999999999999787 ) ;
#8926 = EDGE_LOOP ( 'NONE', ( #19517, #2084, #42197, #43588 ) ) ;
#8925 = CARTESIAN_POINT ( 'NONE',  ( 0.000000000000000000, 35.47612816024556537, -22.48208911017461631 ) ) ;
#8927 = ORIENTED_EDGE ( 'NONE', *, *, #22610, .F. ) ;
#8928 = FACE_OUTER_BOUND ( 'NONE', #20534, .T. ) ;
#8929 = VERTEX_POINT ( 'NONE', #26024 ) ;
#8930 = VERTEX_POINT ( 'NONE', #22111 ) ;
#8931 = CIRCLE ( 'NONE', #10508, 42.00000000000000000 ) ;
#8932 = LINE ( 'NONE', #42721, #4573 ) ;
#8933 = CARTESIAN_POINT ( 'NONE',  ( 10.00000000000000000, -44.99326035066101781, 68.55367621811129197 ) ) ;
#8934 = CARTESIAN_POINT ( 'NONE',  ( 10.00000000000000000, -74.65374052328644439, -8.840884882375878107 ) ) ;
#8935 = ORIENTED_EDGE ( 'NONE', *, *, #24733, .T. ) ;
#8936 = ADVANCED_FACE ( 'NONE', ( #73 ), #29942, .T. ) ;
#8937 = ORIENTED_EDGE ( 'NONE', *, *, #11995, .T. ) ;
#8938 = VERTEX_POINT ( 'NONE', #44875 ) ;
#8939 = DIRECTION ( 'NONE',  ( -1.000000000000000000, 0.000000000000000000, 0.000000000000000000 ) ) ;
#8940 = ORIENTED_EDGE ( 'NONE', *, *, #22166, .F. ) ;
#8941 = DIRECTION ( 'NONE',  ( 0.000000000000000000, 0.000000000000000000, 1.000000000000000000 ) ) ;
#8942 = ADVANCED_FACE ( 'NONE', ( #41215 ), #11591, .T. ) ;
#8943 = CARTESIAN_POINT ( 'NONE',  ( 5.000000000000000000, 38.55633173627010279, 16.65560815589424593 ) ) ;
#8944 = DIRECTION ( 'NONE',  ( 0.000000000000000000, 0.000000000000000000, 1.000000000000000000 ) ) ;
#8945 = FACE_OUTER_BOUND ( 'NONE', #4044, .T. ) ;
#8946 = CARTESIAN_POINT ( 'NONE',  ( -3.000000000000000000, -11.95096189432345390, 23.69967320028757385 ) ) ;
#8947 = AXIS2_PLACEMENT_3D ( 'NONE', #7639, #25742, #22569 ) ;
#8948 = LINE ( 'NONE', #39054, #47903 ) ;
#8949 = EDGE_CURVE ( 'NONE', #4532, #41636, #44396, .T. ) ;
#8950 = DIRECTION ( 'NONE',  ( -1.000000000000000000, -0.000000000000000000, -0.000000000000000000 ) ) ;
#8951 = ORIENTED_EDGE ( 'NONE', *, *, #27096, .T. ) ;
#8952 = DIRECTION ( 'NONE',  ( 0.000000000000000000, 1.000000000000000000, 3.491481338843133750E-15 ) ) ;
#8953 = CARTESIAN_POINT ( 'NONE',  ( 0.000000000000000000, 20.41045688087824317, 72.35160999960824313 ) ) ;
#8954 = VECTOR ( 'NONE', #10520, 1000.000000000000000 ) ;
#8955 = LINE ( 'NONE', #1864, #1178 ) ;
#8956 = ORIENTED_EDGE ( 'NONE', *, *, #44310, .T. ) ;
#8957 = ORIENTED_EDGE ( 'NONE', *, *, #7193, .F. ) ;
#8958 = DIRECTION ( 'NONE',  ( 0.000000000000000000, 0.3826834323650907810, -0.9238795325112864054 ) ) ;
#8959 = AXIS2_PLACEMENT_3D ( 'NONE', #29834, #44764, #43064 ) ;
#8960 = DIRECTION ( 'NONE',  ( -1.000000000000000000, -0.000000000000000000, -0.000000000000000000 ) ) ;
#8961 = CARTESIAN_POINT ( 'NONE',  ( 0.000000000000000000, -21.53537804866058991, -30.80686688397033635 ) ) ;
#8962 = EDGE_CURVE ( 'NONE', #31729, #35538, #7184, .T. ) ;
#8963 = EDGE_CURVE ( 'NONE', #44017, #25896, #37044, .T. ) ;
#8964 = DIRECTION ( 'NONE',  ( 0.000000000000000000, -0.9510565162951565288, 0.3090169943749382364 ) ) ;
#8965 = DIRECTION ( 'NONE',  ( -0.000000000000000000, -0.000000000000000000, -1.000000000000000000 ) ) ;
#8966 = CIRCLE ( 'NONE', #1137, 42.00000000000000000 ) ;
#8967 = VECTOR ( 'NONE', #34786, 1000.000000000000000 ) ;
#8968 = CYLINDRICAL_SURFACE ( 'NONE', #24780, 16.00000000000000355 ) ;
#8969 = DIRECTION ( 'NONE',  ( 1.000000000000000000, 0.000000000000000000, 0.000000000000000000 ) ) ;
#8970 = EDGE_CURVE ( 'NONE', #2830, #1792, #45567, .T. ) ;
#8971 = ORIENTED_EDGE ( 'NONE', *, *, #43604, .F. ) ;
#8972 = AXIS2_PLACEMENT_3D ( 'NONE', #44240, #18996, #22678 ) ;
#8973 = VECTOR ( 'NONE', #6900, 1000.000000000000000 ) ;
#8974 = ORIENTED_EDGE ( 'NONE', *, *, #9761, .F. ) ;
#8975 = PRESENTATION_STYLE_ASSIGNMENT (( #20462 ) ) ;
#8976 = DIRECTION ( 'NONE',  ( -1.000000000000000000, 0.000000000000000000, -0.000000000000000000 ) ) ;
#8977 = CIRCLE ( 'NONE', #37908, 16.00000000000000000 ) ;
#8978 = ORIENTED_EDGE ( 'NONE', *, *, #40977, .F. ) ;
#8979 = EDGE_CURVE ( 'NONE', #11742, #708, #22239, .T. ) ;
#8980 = VERTEX_POINT ( 'NONE', #7439 ) ;
#8981 = VERTEX_POINT ( 'NONE', #38989 ) ;
#8982 = CARTESIAN_POINT ( 'NONE',  ( 15.00000000000000000, 20.85821328998756385, 10.92862929874494249 ) ) ;
#8983 = ORIENTED_EDGE ( 'NONE', *, *, #14084, .F. ) ;
#8984 = ORIENTED_EDGE ( 'NONE', *, *, #10679, .F. ) ;
#8985 = AXIS2_PLACEMENT_3D ( 'NONE', #3777, #18699, #26051 ) ;
#8986 = DIRECTION ( 'NONE',  ( 0.000000000000000000, 0.3826834323650841752, 0.9238795325112891810 ) ) ;
#8987 = VECTOR ( 'NONE', #14303, 1000.000000000000000 ) ;
#8989 = ORIENTED_EDGE ( 'NONE', *, *, #43655, .T. ) ;
#8988 = DIRECTION ( 'NONE',  ( -1.000000000000000000, 0.000000000000000000, 0.000000000000000000 ) ) ;
#8990 = ORIENTED_EDGE ( 'NONE', *, *, #8334, .T. ) ;
#8991 = ORIENTED_EDGE ( 'NONE', *, *, #29966, .F. ) ;
#8992 = DIRECTION ( 'NONE',  ( 0.000000000000000000, 0.000000000000000000, 1.000000000000000000 ) ) ;
#8994 = ORIENTED_EDGE ( 'NONE', *, *, #42066, .F. ) ;
#8993 = LINE ( 'NONE', #8740, #39147 ) ;
#8995 = DIRECTION ( 'NONE',  ( -1.000000000000000000, 0.000000000000000000, 0.000000000000000000 ) ) ;
#8996 = VECTOR ( 'NONE', #6710, 1000.000000000000227 ) ;
#8997 = VECTOR ( 'NONE', #6982, 1000.000000000000000 ) ;
#8998 = ORIENTED_EDGE ( 'NONE', *, *, #8079, .T. ) ;
#8999 = DIRECTION ( 'NONE',  ( 0.000000000000000000, -0.9876883405951393247, 0.1564344650402204329 ) ) ;
#9000 = ORIENTED_EDGE ( 'NONE', *, *, #41955, .T. ) ;
#9001 = VERTEX_POINT ( 'NONE', #16709 ) ;
#9002 = FACE_OUTER_BOUND ( 'NONE', #35009, .T. ) ;
#9003 = FACE_OUTER_BOUND ( 'NONE', #7835, .T. ) ;
#9004 = ORIENTED_EDGE ( 'NONE', *, *, #31031, .T. ) ;
#9005 = EDGE_CURVE ( 'NONE', #44556, #22290, #34731, .T. ) ;
#9006 = CIRCLE ( 'NONE', #36361, 31.99999999999998934 ) ;
#9007 = DIRECTION ( 'NONE',  ( 0.000000000000000000, 0.000000000000000000, 1.000000000000000000 ) ) ;
#9008 = CARTESIAN_POINT ( 'NONE',  ( 10.00000000000000000, -33.17418723428294669, -17.67226234102862747 ) ) ;
#9009 = FACE_OUTER_BOUND ( 'NONE', #32352, .T. ) ;
#9010 = EDGE_CURVE ( 'NONE', #9234, #4565, #46578, .T. ) ;
#9012 = ORIENTED_EDGE ( 'NONE', *, *, #47960, .F. ) ;
#9011 = VECTOR ( 'NONE', #38323, 1000.000000000000000 ) ;
#9013 = EDGE_CURVE ( 'NONE', #10088, #27708, #12845, .T. ) ;
#9014 = AXIS2_PLACEMENT_3D ( 'NONE', #2911, #40597, #25420 ) ;
#9015 = ORIENTED_EDGE ( 'NONE', *, *, #40835, .F. ) ;
#9016 = CARTESIAN_POINT ( 'NONE',  ( 10.00000000000000000, -16.45098606841102651, -33.79645857604531045 ) ) ;
#9017 = EDGE_CURVE ( 'NONE', #27718, #17850, #47258, .T. ) ;
#9018 = CARTESIAN_POINT ( 'NONE',  ( 5.999999999999999112, 50.23322058963442771, -64.81221759200288091 ) ) ;
#9019 = ORIENTED_EDGE ( 'NONE', *, *, #16869, .T. ) ;
#9020 = ADVANCED_FACE ( 'NONE', ( #23809 ), #31659, .T. ) ;
#9021 = FACE_OUTER_BOUND ( 'NONE', #28927, .T. ) ;
#9022 = ORIENTED_EDGE ( 'NONE', *, *, #20098, .T. ) ;
#9023 = DIRECTION ( 'NONE',  ( -1.000000000000000000, 0.000000000000000000, 0.000000000000000000 ) ) ;
#9024 = FACE_OUTER_BOUND ( 'NONE', #38196, .T. ) ;
#9025 = CYLINDRICAL_SURFACE ( 'NONE', #12851, 82.00000000000000000 ) ;
#9026 = VECTOR ( 'NONE', #22011, 1000.000000000000000 ) ;
#9027 = DIRECTION ( 'NONE',  ( -1.000000000000000000, 0.000000000000000000, 0.000000000000000000 ) ) ;
#9028 = SURFACE_STYLE_FILL_AREA ( #9744 ) ;
#9029 = DIRECTION ( 'NONE',  ( -1.000000000000000000, 0.000000000000000000, 0.000000000000000000 ) ) ;
#9030 = CIRCLE ( 'NONE', #18375, 31.99999999999999289 ) ;
#9031 = LINE ( 'NONE', #46729, #33296 ) ;
#9032 = DIRECTION ( 'NONE',  ( -1.000000000000000000, 0.000000000000000000, 0.000000000000000000 ) ) ;
#9033 = EDGE_CURVE ( 'NONE', #38628, #44271, #1540, .T. ) ;
#9034 = ORIENTED_EDGE ( 'NONE', *, *, #23213, .F. ) ;
#9035 = FACE_BOUND ( 'NONE', #41197, .T. ) ;
#9036 = ORIENTED_EDGE ( 'NONE', *, *, #6152, .F. ) ;
#9037 = EDGE_CURVE ( 'NONE', #43974, #27838, #15987, .T. ) ;
#9038 = VECTOR ( 'NONE', #19158, 1000.000000000000000 ) ;
#9039 = CIRCLE ( 'NONE', #36391, 31.99999999999999289 ) ;
#9040 = DIRECTION ( 'NONE',  ( 0.000000000000000000, 0.000000000000000000, 1.000000000000000000 ) ) ;
#9041 = ORIENTED_EDGE ( 'NONE', *, *, #41962, .F. ) ;
#9042 = AXIS2_PLACEMENT_3D ( 'NONE', #25080, #17494, #2103 ) ;
#9043 = CARTESIAN_POINT ( 'NONE',  ( 10.00000000000000000, 27.05870788708231700, 26.08949754953034272 ) ) ;
#9044 = DIRECTION ( 'NONE',  ( -0.9435911131814402886, 0.3311129884571281101, 0.000000000000000000 ) ) ;
#9045 = AXIS2_PLACEMENT_3D ( 'NONE', #14559, #85, #25550 ) ;
#9046 = VERTEX_POINT ( 'NONE', #13048 ) ;
#9047 = CIRCLE ( 'NONE', #9014, 77.49899999999999523 ) ;
#9048 = EDGE_CURVE ( 'NONE', #38765, #33441, #3356, .T. ) ;
#9049 = DIRECTION ( 'NONE',  ( 0.000000000000000000, 0.4539904997395477482, -0.8910065241883674547 ) ) ;
#9050 = ORIENTED_EDGE ( 'NONE', *, *, #42011, .T. ) ;
#9051 = ORIENTED_EDGE ( 'NONE', *, *, #28276, .T. ) ;
#9052 = CIRCLE ( 'NONE', #42676, 31.99999999999999289 ) ;
#9053 = ORIENTED_EDGE ( 'NONE', *, *, #23519, .T. ) ;
#9054 = AXIS2_PLACEMENT_3D ( 'NONE', #19196, #37321, #15530 ) ;
#9055 = EDGE_CURVE ( 'NONE', #42613, #7751, #35302, .T. ) ;
#9056 = CIRCLE ( 'NONE', #34842, 16.00000000000000000 ) ;
#9057 = CARTESIAN_POINT ( 'NONE',  ( 0.000000000000000000, -46.54456581323762521, -59.03342792756313884 ) ) ;
#9058 = ORIENTED_EDGE ( 'NONE', *, *, #34614, .F. ) ;
#9059 = DIRECTION ( 'NONE',  ( 0.000000000000000000, -0.8910065241883721177, 0.4539904997395382003 ) ) ;
#9060 = ORIENTED_EDGE ( 'NONE', *, *, #9603, .T. ) ;
#9061 = EDGE_CURVE ( 'NONE', #29866, #18807, #30726, .T. ) ;
#9062 = CARTESIAN_POINT ( 'NONE',  ( -7.572224309238338336, -145.4393675041377492, -2.500000000000000444 ) ) ;
#9063 = CARTESIAN_POINT ( 'NONE',  ( 10.00000000000000000, 0.000000000000000000, 0.000000000000000000 ) ) ;
#9064 = EDGE_CURVE ( 'NONE', #37275, #42611, #18201, .T. ) ;
#9065 = DIRECTION ( 'NONE',  ( 0.000000000000000000, -6.982962677686267499E-15, 1.000000000000000000 ) ) ;
#9066 = AXIS2_PLACEMENT_3D ( 'NONE', #43214, #34902, #46410 ) ;
#9067 = ORIENTED_EDGE ( 'NONE', *, *, #20906, .T. ) ;
#9068 = ADVANCED_FACE ( 'NONE', ( #27978 ), #9122, .T. ) ;
#9069 = CARTESIAN_POINT ( 'NONE',  ( 0.000000000000000000, 0.000000000000000000, 0.000000000000000000 ) ) ;
#9070 = VERTEX_POINT ( 'NONE', #24285 ) ;
#9071 = CARTESIAN_POINT ( 'NONE',  ( 10.00000000000000000, -37.58145647212455032, 0.6853352020789044152 ) ) ;
#9072 = DIRECTION ( 'NONE',  ( 0.000000000000000000, 0.000000000000000000, 1.000000000000000000 ) ) ;
#9073 = VERTEX_POINT ( 'NONE', #23322 ) ;
#9074 = CARTESIAN_POINT ( 'NONE',  ( -10.00000000000000000, 0.000000000000000000, 0.000000000000000000 ) ) ;
#9075 = ORIENTED_EDGE ( 'NONE', *, *, #32162, .F. ) ;
#9076 = VERTEX_POINT ( 'NONE', #5691 ) ;
#9077 = EDGE_CURVE ( 'NONE', #46520, #22527, #27701, .T. ) ;
#9078 = CARTESIAN_POINT ( 'NONE',  ( 0.000000000000000000, 23.16143007188530234, -73.95703589263949596 ) ) ;
#9079 = CARTESIAN_POINT ( 'NONE',  ( 0.000000000000000000, 0.000000000000000000, 0.000000000000000000 ) ) ;
#9080 = CARTESIAN_POINT ( 'NONE',  ( 10.00000000000000000, 0.8828120875905820508, -37.48860685352290290 ) ) ;
#9081 = AXIS2_PLACEMENT_3D ( 'NONE', #5467, #39006, #20385 ) ;
#9082 = FACE_OUTER_BOUND ( 'NONE', #42956, .T. ) ;
#9083 = CARTESIAN_POINT ( 'NONE',  ( 0.000000000000000000, -39.04073710021356192, 15.48615015657568073 ) ) ;
#9084 = VECTOR ( 'NONE', #12037, 1000.000000000000114 ) ;
#9085 = CARTESIAN_POINT ( 'NONE',  ( 0.000000000000000000, 34.44570377933693806, -69.42325613327405165 ) ) ;
#9086 = CYLINDRICAL_SURFACE ( 'NONE', #37607, 37.49900000000000233 ) ;
#9087 = CARTESIAN_POINT ( 'NONE',  ( 0.000000000000000000, -37.22597642581153821, -5.202137450156795850 ) ) ;
#9088 = CARTESIAN_POINT ( 'NONE',  ( -10.00000000000000000, 0.000000000000000000, 0.000000000000000000 ) ) ;
#9089 = DIRECTION ( 'NONE',  ( 0.000000000000000000, 0.000000000000000000, 1.000000000000000000 ) ) ;
#9090 = CARTESIAN_POINT ( 'NONE',  ( 0.000000000000000000, 0.000000000000000000, 0.000000000000000000 ) ) ;
#9091 = SHAPE_REPRESENTATION ( 'small gear_ISO - Spur gear 2M 40T 20PA 10FW ---S40A75H50L20.0N', ( #11636 ), #10100 ) ;
#9092 = AXIS2_PLACEMENT_3D ( 'NONE', #28719, #33093, #36295 ) ;
#9093 = ORIENTED_EDGE ( 'NONE', *, *, #5652, .F. ) ;
#9094 = CARTESIAN_POINT ( 'NONE',  ( 0.000000000000000000, 0.000000000000000000, 0.000000000000000000 ) ) ;
#9095 = CARTESIAN_POINT ( 'NONE',  ( 26.09152095774781444, -124.8716048804687375, 2.500000000000000000 ) ) ;
#9096 = DIRECTION ( 'NONE',  ( 1.000000000000000000, -0.000000000000000000, -0.000000000000000000 ) ) ;
#9097 = CIRCLE ( 'NONE', #34865, 16.00000000000000000 ) ;
#9098 = FACE_OUTER_BOUND ( 'NONE', #13812, .T. ) ;
#9099 = ORIENTED_EDGE ( 'NONE', *, *, #19542, .T. ) ;
#9100 = VECTOR ( 'NONE', #7813, 1000.000000000000000 ) ;
#9101 = DIRECTION ( 'NONE',  ( 0.000000000000000000, 0.000000000000000000, 1.000000000000000000 ) ) ;
#9102 = FACE_OUTER_BOUND ( 'NONE', #10221, .T. ) ;
#9103 = DIRECTION ( 'NONE',  ( 1.000000000000000000, 0.000000000000000000, 0.000000000000000000 ) ) ;
#9104 = ORIENTED_EDGE ( 'NONE', *, *, #29018, .F. ) ;
#9105 = CIRCLE ( 'NONE', #13800, 31.99999999999999645 ) ;
#9106 = FACE_OUTER_BOUND ( 'NONE', #4051, .T. ) ;
#9107 = DIRECTION ( 'NONE',  ( 1.000000000000000000, 0.000000000000000000, 0.000000000000000000 ) ) ;
#9108 = AXIS2_PLACEMENT_3D ( 'NONE', #28400, #47250, #6136 ) ;
#9109 = ORIENTED_EDGE ( 'NONE', *, *, #21977, .T. ) ;
#9110 =( NAMED_UNIT ( * ) SI_UNIT ( $, .STERADIAN. ) SOLID_ANGLE_UNIT ( ) );
#9111 = DIRECTION ( 'NONE',  ( 0.000000000000000000, 0.000000000000000000, -1.000000000000000000 ) ) ;
#9112 = VERTEX_POINT ( 'NONE', #1304 ) ;
#9113 = VECTOR ( 'NONE', #20270, 1000.000000000000000 ) ;
#9114 = CARTESIAN_POINT ( 'NONE',  ( 15.00000000000000000, 23.49999999999999645, 1.499999999999995337 ) ) ;
#9115 = ORIENTED_EDGE ( 'NONE', *, *, #6246, .F. ) ;
#9116 = EDGE_CURVE ( 'NONE', #38558, #40145, #15739, .T. ) ;
#9117 = CARTESIAN_POINT ( 'NONE',  ( 10.00000000000000000, 69.42325613327489009, -34.44570377933524696 ) ) ;
#9118 = VERTEX_POINT ( 'NONE', #27247 ) ;
#9119 = EDGE_CURVE ( 'NONE', #48250, #3237, #5834, .T. ) ;
#9120 = VECTOR ( 'NONE', #4095, 1000.000000000000000 ) ;
#9121 = FACE_BOUND ( 'NONE', #40734, .T. ) ;
#9122 = CYLINDRICAL_SURFACE ( 'NONE', #48013, 77.49899999999999523 ) ;
#9123 = LINE ( 'NONE', #8395, #34065 ) ;
#9124 = CYLINDRICAL_SURFACE ( 'NONE', #38444, 77.49899999999999523 ) ;
#9125 = EDGE_CURVE ( 'NONE', #21677, #17728, #27011, .T. ) ;
#9126 = AXIS2_PLACEMENT_3D ( 'NONE', #12465, #23968, #5361 ) ;
#9127 = LINE ( 'NONE', #47292, #24236 ) ;
#9128 = VERTEX_POINT ( 'NONE', #19878 ) ;
#9129 = DIRECTION ( 'NONE',  ( 0.000000000000000000, -0.9781476007338065770, -0.2079116908177544853 ) ) ;
#9130 = VERTEX_POINT ( 'NONE', #31168 ) ;
#9131 = ORIENTED_EDGE ( 'NONE', *, *, #29081, .F. ) ;
#9132 = ADVANCED_FACE ( 'NONE', ( #34821 ), #16236, .T. ) ;
#9133 = DIRECTION ( 'NONE',  ( -1.000000000000000000, -0.000000000000000000, 0.000000000000000000 ) ) ;
#9134 = DIRECTION ( 'NONE',  ( 0.000000000000000000, 0.7071067811865437980, 0.7071067811865513475 ) ) ;
#9135 = EDGE_CURVE ( 'NONE', #25765, #39311, #43140, .T. ) ;
#9136 = LINE ( 'NONE', #16959, #23458 ) ;
#9137 = LINE ( 'NONE', #19646, #3973 ) ;
#9138 = ORIENTED_EDGE ( 'NONE', *, *, #13886, .F. ) ;
#9139 = CARTESIAN_POINT ( 'NONE',  ( 0.000000000000000000, -17.28742895386137590, 75.54627589209937355 ) ) ;
#9140 = LINE ( 'NONE', #31920, #26817 ) ;
#9141 = CARTESIAN_POINT ( 'NONE',  ( 10.00000000000000000, 39.78640506895604290, 66.50666863322015843 ) ) ;
#9142 = CARTESIAN_POINT ( 'NONE',  ( 0.000000000000000000, -62.50884508063395373, -41.76106447765554464 ) ) ;
#9143 = DIRECTION ( 'NONE',  ( -1.000000000000000000, 0.000000000000000000, -0.000000000000000000 ) ) ;
#9144 = AXIS2_PLACEMENT_3D ( 'NONE', #7963, #8939, #41515 ) ;
#9145 = CARTESIAN_POINT ( 'NONE',  ( 0.000000000000000000, 41.76937507738875155, -62.50329211542393892 ) ) ;
#9146 = DIRECTION ( 'NONE',  ( -1.000000000000000000, 0.000000000000000000, -0.000000000000000000 ) ) ;
#9148 = CARTESIAN_POINT ( 'NONE',  ( 10.00000000000000000, -25.88420570971419821, 27.13269053701087330 ) ) ;
#9147 = APPLICATION_CONTEXT ( 'automotive_design' ) ;
#9149 = CIRCLE ( 'NONE', #23998, 31.99999999999998579 ) ;
#9150 = LINE ( 'NONE', #20158, #7230 ) ;
#9151 = CARTESIAN_POINT ( 'NONE',  ( 10.00000000000000000, 0.000000000000000000, 0.000000000000000000 ) ) ;
#9152 = ORIENTED_EDGE ( 'NONE', *, *, #47155, .F. ) ;
#9153 = DIRECTION ( 'NONE',  ( 0.000000000000000000, -0.9510565162951503115, 0.3090169943749573878 ) ) ;
#9154 = VECTOR ( 'NONE', #40684, 1000.000000000000114 ) ;
#9155 = ORIENTED_EDGE ( 'NONE', *, *, #27304, .F. ) ;
#9156 = CYLINDRICAL_SURFACE ( 'NONE', #19074, 16.00000000000000000 ) ;
#9157 = LINE ( 'NONE', #20170, #47912 ) ;
#9158 = ORIENTED_EDGE ( 'NONE', *, *, #27356, .F. ) ;
#9159 = AXIS2_PLACEMENT_3D ( 'NONE', #8185, #26784, #25806 ) ;
#9160 = EDGE_CURVE ( 'NONE', #24887, #48217, #4252, .T. ) ;
#9161 = ORIENTED_EDGE ( 'NONE', *, *, #18170, .T. ) ;
#9162 = ADVANCED_FACE ( 'NONE', ( #47290 ), #21085, .F. ) ;
#9163 = CARTESIAN_POINT ( 'NONE',  ( 5.000000000000000000, -33.71516098798685590, -74.74816331893465815 ) ) ;
#9164 = ORIENTED_EDGE ( 'NONE', *, *, #42891, .T. ) ;
#9165 = ORIENTED_EDGE ( 'NONE', *, *, #19290, .F. ) ;
#9166 = EDGE_CURVE ( 'NONE', #15496, #44922, #2966, .T. ) ;
#9167 = CARTESIAN_POINT ( 'NONE',  ( -14.87942725330654348, -141.9795960975983178, 5.500000000000000000 ) ) ;
#9168 = DIRECTION ( 'NONE',  ( 0.000000000000000000, 0.000000000000000000, -1.000000000000000000 ) ) ;
#9170 = ORIENTED_EDGE ( 'NONE', *, *, #14104, .T. ) ;
#9169 = CARTESIAN_POINT ( 'NONE',  ( 10.00000000000000000, 0.000000000000000000, 0.000000000000000000 ) ) ;
#9171 = ORIENTED_EDGE ( 'NONE', *, *, #11785, .F. ) ;
#9172 = CIRCLE ( 'NONE', #28720, 77.49900000000000944 ) ;
#9173 = FACE_OUTER_BOUND ( 'NONE', #21336, .T. ) ;
#9174 = EDGE_CURVE ( 'NONE', #18614, #21261, #47743, .T. ) ;
#9175 = ORIENTED_EDGE ( 'NONE', *, *, #15756, .F. ) ;
#9176 = EDGE_CURVE ( 'NONE', #24549, #10969, #17895, .T. ) ;
#9177 = EDGE_CURVE ( 'NONE', #38028, #9618, #36261, .T. ) ;
#9178 = DIRECTION ( 'NONE',  ( 0.000000000000000000, -0.5224985647159379187, -0.8526401643540989506 ) ) ;
#9179 = DIRECTION ( 'NONE',  ( -1.000000000000000000, 0.000000000000000000, -0.000000000000000000 ) ) ;
#9180 = PLANE ( 'NONE',  #3206 ) ;
#9181 = ORIENTED_EDGE ( 'NONE', *, *, #37677, .T. ) ;
#9182 = ORIENTED_EDGE ( 'NONE', *, *, #15584, .T. ) ;
#9183 = AXIS2_PLACEMENT_3D ( 'NONE', #1003, #31619, #23521 ) ;
#9184 = ORIENTED_EDGE ( 'NONE', *, *, #48290, .F. ) ;
#9185 = CARTESIAN_POINT ( 'NONE',  ( 11.99999999999999822, 59.03961581697399907, 46.53671651293969802 ) ) ;
#9186 = VERTEX_POINT ( 'NONE', #9585 ) ;
#9187 = LINE ( 'NONE', #24120, #11362 ) ;
#9188 = CARTESIAN_POINT ( 'NONE',  ( 10.00000000000000000, -73.95703589263990807, 23.16143007188399139 ) ) ;
#9189 = DIRECTION ( 'NONE',  ( -1.000000000000000000, -0.000000000000000000, 0.000000000000000000 ) ) ;
#9190 = DIRECTION ( 'NONE',  ( 0.000000000000000000, -0.07845909572785234043, 0.9969173337331274087 ) ) ;
#9191 = CARTESIAN_POINT ( 'NONE',  ( 12.00000000000000000, -19.89357724624986545, 12.59942793731086219 ) ) ;
#9192 = LINE ( 'NONE', #15813, #19772 ) ;
#9193 = CARTESIAN_POINT ( 'NONE',  ( -0.9515373497862389396, -96.47140937769621871, -5.500000000000000000 ) ) ;
#9194 = ORIENTED_EDGE ( 'NONE', *, *, #3886, .F. ) ;
#9196 = EDGE_CURVE ( 'NONE', #27800, #30662, #35553, .T. ) ;
#9195 = CARTESIAN_POINT ( 'NONE',  ( 10.00000000000000000, -33.79645857604525361, 16.45098606841114730 ) ) ;
#9197 = CIRCLE ( 'NONE', #14686, 16.00000000000000355 ) ;
#9198 = CARTESIAN_POINT ( 'NONE',  ( 10.00000000000000000, 68.26794271651262136, 31.47745569255165066 ) ) ;
#9199 = PLANE ( 'NONE',  #25408 ) ;
#9200 = ORIENTED_EDGE ( 'NONE', *, *, #31456, .T. ) ;
#9201 = CARTESIAN_POINT ( 'NONE',  ( 10.00000000000000000, 75.11764819372149304, -2.946379043146603482 ) ) ;
#9202 = DIRECTION ( 'NONE',  ( 1.000000000000000000, -0.000000000000000000, -0.000000000000000000 ) ) ;
#9203 = CARTESIAN_POINT ( 'NONE',  ( 11.99999999999999822, 30.41916302227216562, -71.27951684757994144 ) ) ;
#9204 = CYLINDRICAL_SURFACE ( 'NONE', #6030, 21.00000000000000000 ) ;
#9205 = CARTESIAN_POINT ( 'NONE',  ( 10.00000000000000000, 8.830959090342393125, 74.65491531819122883 ) ) ;
#9206 = VECTOR ( 'NONE', #25006, 1000.000000000000000 ) ;
#9207 = DIRECTION ( 'NONE',  ( -1.000000000000000000, -0.000000000000000000, -0.000000000000000000 ) ) ;
#9208 = PLANE ( 'NONE',  #8916 ) ;
#9209 = VERTEX_POINT ( 'NONE', #6656 ) ;
#9210 = CARTESIAN_POINT ( 'NONE',  ( -10.00000000000000000, 0.000000000000000000, 0.000000000000000000 ) ) ;
#9211 = AXIS2_PLACEMENT_3D ( 'NONE', #35030, #16673, #42382 ) ;
#9212 = CIRCLE ( 'NONE', #36559, 31.99999999999999289 ) ;
#9213 = ORIENTED_EDGE ( 'NONE', *, *, #5330, .T. ) ;
#9214 = PRODUCT_CONTEXT ( 'NONE', #41030, 'mechanical' ) ;
#9215 = CARTESIAN_POINT ( 'NONE',  ( 10.00000000000000000, 51.02545421589402252, -55.20638768913705263 ) ) ;
#9216 = VERTEX_POINT ( 'NONE', #47518 ) ;
#9217 = EDGE_CURVE ( 'NONE', #46297, #44946, #12085, .T. ) ;
#9218 = ORIENTED_EDGE ( 'NONE', *, *, #39972, .F. ) ;
#9219 = EDGE_CURVE ( 'NONE', #30611, #11880, #5948, .T. ) ;
#9220 = VERTEX_POINT ( 'NONE', #25230 ) ;
#9221 = LINE ( 'NONE', #28072, #35121 ) ;
#9222 = COLOUR_RGB ( '', 0.66274510, 0.83137255, 0.94901961) ;
#9223 = VERTEX_POINT ( 'NONE', #36017 ) ;
#9224 = ADVANCED_FACE ( 'NONE', ( #20866 ), #44091, .F. ) ;
#9225 = ORIENTED_EDGE ( 'NONE', *, *, #29788, .T. ) ;
#9226 = CARTESIAN_POINT ( 'NONE',  ( 11.99999999999999822, 69.42325613327440692, 34.44570377933622041 ) ) ;
#9227 = CARTESIAN_POINT ( 'NONE',  ( 10.00000000000000000, -74.65491531819111515, -8.830959090343204920 ) ) ;
#9228 = EDGE_LOOP ( 'NONE', ( #6525, #35582, #8683, #44917 ) ) ;
#9229 = ORIENTED_EDGE ( 'NONE', *, *, #43837, .T. ) ;
#9230 = EDGE_CURVE ( 'NONE', #39825, #10102, #28199, .T. ) ;
#9231 = ADVANCED_FACE ( 'NONE', ( #16946 ), #17409, .T. ) ;
#9232 = CARTESIAN_POINT ( 'NONE',  ( 0.000000000000000000, -20.55727247249726020, -16.78983467731313084 ) ) ;
#9234 = VERTEX_POINT ( 'NONE', #2728 ) ;
#9233 = CARTESIAN_POINT ( 'NONE',  ( -3.000000000000000000, -22.32062822937469804, -14.36278369418829826 ) ) ;
#9235 = VECTOR ( 'NONE', #33211, 1000.000000000000000 ) ;
#9236 = DIRECTION ( 'NONE',  ( 0.000000000000000000, 0.000000000000000000, 1.000000000000000000 ) ) ;
#9237 = ORIENTED_EDGE ( 'NONE', *, *, #29796, .F. ) ;
#9238 = DIRECTION ( 'NONE',  ( 0.000000000000000000, 0.000000000000000000, 1.000000000000000000 ) ) ;
#9239 = ORIENTED_EDGE ( 'NONE', *, *, #11271, .T. ) ;
#9240 = ORIENTED_EDGE ( 'NONE', *, *, #12240, .F. ) ;
#9241 = DIRECTION ( 'NONE',  ( -1.000000000000000000, -0.000000000000000000, -0.000000000000000000 ) ) ;
#9242 = CARTESIAN_POINT ( 'NONE',  ( 0.000000000000000000, -75.11725578898466438, -2.956366410621452001 ) ) ;
#9243 = ORIENTED_EDGE ( 'NONE', *, *, #47891, .F. ) ;
#9244 = AXIS2_PLACEMENT_3D ( 'NONE', #24176, #30808, #34945 ) ;
#9245 = DIRECTION ( 'NONE',  ( 1.000000000000000000, 0.000000000000000000, -0.000000000000000000 ) ) ;
#9246 = FACE_OUTER_BOUND ( 'NONE', #33683, .T. ) ;
#9247 = FACE_OUTER_BOUND ( 'NONE', #31198, .T. ) ;
#9248 = VECTOR ( 'NONE', #5561, 1000.000000000000000 ) ;
#9249 = EDGE_LOOP ( 'NONE', ( #33005, #37416, #17371, #10781 ) ) ;
#9250 = ORIENTED_EDGE ( 'NONE', *, *, #38063, .F. ) ;
#9251 = CYLINDRICAL_SURFACE ( 'NONE', #32889, 82.00000000000000000 ) ;
#9252 = EDGE_CURVE ( 'NONE', #29586, #18510, #9721, .T. ) ;
#9253 = DIRECTION ( 'NONE',  ( -1.000000000000000000, 0.000000000000000000, -0.000000000000000000 ) ) ;
#9254 = ORIENTED_EDGE ( 'NONE', *, *, #39396, .T. ) ;
#9255 = CARTESIAN_POINT ( 'NONE',  ( 10.00000000000000000, -56.15606465354917987, -59.75363087400133111 ) ) ;
#9256 = EDGE_LOOP ( 'NONE', ( #24706, #3432, #31118, #34132 ) ) ;
#9257 = CARTESIAN_POINT ( 'NONE',  ( 11.99999999999999822, -70.52718814184277107, 26.02418014898285037 ) ) ;
#9258 = DIRECTION ( 'NONE',  ( 1.000000000000000000, 0.000000000000000000, 0.000000000000000000 ) ) ;
#9259 = DIRECTION ( 'NONE',  ( -0.7950889364178796992, 0.6064928550163511956, 0.000000000000000000 ) ) ;
#9260 = DIRECTION ( 'NONE',  ( -1.000000000000000000, 0.000000000000000000, -0.000000000000000000 ) ) ;
#9261 = DIRECTION ( 'NONE',  ( -1.000000000000000000, -0.000000000000000000, -0.000000000000000000 ) ) ;
#9262 = VECTOR ( 'NONE', #15961, 1000.000000000000000 ) ;
#9263 = CARTESIAN_POINT ( 'NONE',  ( 0.000000000000000000, -0.8299999999999999600, -1.199999999999999956 ) ) ;
#9264 = ORIENTED_EDGE ( 'NONE', *, *, #37138, .F. ) ;
#9265 = DIRECTION ( 'NONE',  ( -1.000000000000000000, 0.000000000000000000, -0.000000000000000000 ) ) ;
#9266 = DIRECTION ( 'NONE',  ( 0.000000000000000000, -1.000000000000000000, 1.156482317317870936E-15 ) ) ;
#9267 = DIRECTION ( 'NONE',  ( 0.000000000000000000, 0.5224985647159500202, -0.8526401643540915121 ) ) ;
#9268 = CARTESIAN_POINT ( 'NONE',  ( 10.00000000000000000, 0.000000000000000000, 0.000000000000000000 ) ) ;
#9269 = SURFACE_STYLE_FILL_AREA ( #39382 ) ;
#9270 = ORIENTED_EDGE ( 'NONE', *, *, #24636, .T. ) ;
#9272 = ADVANCED_FACE ( 'NONE', ( #13767 ), #43615, .F. ) ;
#9271 = AXIS2_PLACEMENT_3D ( 'NONE', #14157, #10482, #21736 ) ;
#9273 = VECTOR ( 'NONE', #2160, 1000.000000000000000 ) ;
#9274 = CARTESIAN_POINT ( 'NONE',  ( 11.99999999999999822, -27.74655509720618696, -77.16300072079690153 ) ) ;
#9275 = DIRECTION ( 'NONE',  ( 0.000000000000000000, 0.000000000000000000, 1.000000000000000000 ) ) ;
#9276 = EDGE_CURVE ( 'NONE', #11173, #28070, #45600, .T. ) ;
#9277 = AXIS2_PLACEMENT_3D ( 'NONE', #20190, #35111, #13099 ) ;
#9278 = ORIENTED_EDGE ( 'NONE', *, *, #382, .T. ) ;
#9279 = EDGE_CURVE ( 'NONE', #7784, #31833, #40128, .T. ) ;
#9280 = EDGE_CURVE ( 'NONE', #41101, #18029, #10418, .T. ) ;
#9281 = CARTESIAN_POINT ( 'NONE',  ( 11.99999999999999822, 74.65491531819118620, -8.830959090342659579 ) ) ;
#9282 = ORIENTED_EDGE ( 'NONE', *, *, #2, .F. ) ;
#9283 = ORIENTED_EDGE ( 'NONE', *, *, #25343, .F. ) ;
#9284 = ORIENTED_EDGE ( 'NONE', *, *, #7990, .F. ) ;
#9285 = ORIENTED_EDGE ( 'NONE', *, *, #16635, .F. ) ;
#9286 = EDGE_CURVE ( 'NONE', #26342, #4178, #47996, .T. ) ;
#9287 = PRESENTATION_LAYER_ASSIGNMENT (  '', '', ( #17872 ) ) ;
#9288 = CARTESIAN_POINT ( 'NONE',  ( 0.000000000000000000, 29.01471420065563933, 76.69515212746026123 ) ) ;
#9289 = VERTEX_POINT ( 'NONE', #26223 ) ;
#9290 = DIRECTION ( 'NONE',  ( -1.000000000000000000, 0.000000000000000000, -0.000000000000000000 ) ) ;
#9291 = EDGE_CURVE ( 'NONE', #37286, #675, #26037, .T. ) ;
#9292 = EDGE_LOOP ( 'NONE', ( #29729, #36986, #18583, #14951 ) ) ;
#9293 = CARTESIAN_POINT ( 'NONE',  ( 10.00000000000000000, 12.26510123303308752, -35.53030884539072787 ) ) ;
#9294 = FACE_OUTER_BOUND ( 'NONE', #30332, .T. ) ;
#9295 = CARTESIAN_POINT ( 'NONE',  ( 10.00000000000000000, 0.000000000000000000, 0.000000000000000000 ) ) ;
#9296 = ORIENTED_EDGE ( 'NONE', *, *, #7890, .F. ) ;
#9297 = CARTESIAN_POINT ( 'NONE',  ( 10.00000000000000000, 0.000000000000000000, 0.000000000000000000 ) ) ;
#9298 = ORIENTED_EDGE ( 'NONE', *, *, #46610, .T. ) ;
#9299 = DIRECTION ( 'NONE',  ( 1.000000000000000000, -0.000000000000000000, 0.000000000000000000 ) ) ;
#9300 = EDGE_CURVE ( 'NONE', #2423, #45055, #15214, .T. ) ;
#9301 = CARTESIAN_POINT ( 'NONE',  ( 10.00000000000000000, 0.000000000000000000, 0.000000000000000000 ) ) ;
#9302 = DIRECTION ( 'NONE',  ( -0.000000000000000000, -0.000000000000000000, -1.000000000000000000 ) ) ;
#9303 = ORIENTED_EDGE ( 'NONE', *, *, #22346, .T. ) ;
#9304 = AXIS2_PLACEMENT_3D ( 'NONE', #38365, #19496, #437 ) ;
#9305 = VERTEX_POINT ( 'NONE', #26462 ) ;
#9306 = DIRECTION ( 'NONE',  ( -0.000000000000000000, -0.9945218953682741780, 0.1045284632676447834 ) ) ;
#9307 = DIRECTION ( 'NONE',  ( -1.000000000000000000, 0.000000000000000000, 0.000000000000000000 ) ) ;
#9308 = VERTEX_POINT ( 'NONE', #22546 ) ;
#9309 = AXIS2_PLACEMENT_3D ( 'NONE', #7284, #22228, #37153 ) ;
#9310 = DIRECTION ( 'NONE',  ( -1.000000000000000000, -0.000000000000000000, 0.000000000000000000 ) ) ;
#9311 = CARTESIAN_POINT ( 'NONE',  ( 0.000000000000000000, -49.70050353004931054, 59.46389618801946142 ) ) ;
#9312 = DIRECTION ( 'NONE',  ( -1.000000000000000000, -0.000000000000000000, -0.000000000000000000 ) ) ;
#9313 = AXIS2_PLACEMENT_3D ( 'NONE', #45720, #183, #8271 ) ;
#9314 = LINE ( 'NONE', #39430, #44550 ) ;
#9315 = DIRECTION ( 'NONE',  ( 0.000000000000000000, 0.000000000000000000, 1.000000000000000000 ) ) ;
#9316 = CARTESIAN_POINT ( 'NONE',  ( 4.999999999999999112, -41.81611651403859042, -3.925862922256606602 ) ) ;
#9317 = EDGE_CURVE ( 'NONE', #11779, #45199, #29182, .T. ) ;
#9318 = DIRECTION ( 'NONE',  ( -1.000000000000000000, -0.000000000000000000, 0.000000000000000000 ) ) ;
#9319 = DIRECTION ( 'NONE',  ( 0.1736481776669309418, 0.9848077530122080203, -0.000000000000000000 ) ) ;
#9320 = CARTESIAN_POINT ( 'NONE',  ( 11.99999999999999822, -51.03279382321125723, 55.19960302592048862 ) ) ;
#9321 = VERTEX_POINT ( 'NONE', #37476 ) ;
#9322 = DIRECTION ( 'NONE',  ( 0.000000000000000000, -0.6494480483301739993, -0.7604059656000391465 ) ) ;
#9323 = DIRECTION ( 'NONE',  ( -1.000000000000000000, 0.000000000000000000, -0.000000000000000000 ) ) ;
#9324 = DIRECTION ( 'NONE',  ( -1.000000000000000000, 0.000000000000000000, 0.000000000000000000 ) ) ;
#9325 = DIRECTION ( 'NONE',  ( 1.000000000000000000, 0.000000000000000000, 0.000000000000000000 ) ) ;
#9326 = DIRECTION ( 'NONE',  ( 0.000000000000000000, -0.1564344650402170189, -0.9876883405951399908 ) ) ;
#9327 = EDGE_LOOP ( 'NONE', ( #36957, #154, #3708, #12635 ) ) ;
#9328 =( GEOMETRIC_REPRESENTATION_CONTEXT ( 3 ) GLOBAL_UNCERTAINTY_ASSIGNED_CONTEXT ( ( #36944 ) ) GLOBAL_UNIT_ASSIGNED_CONTEXT ( ( #46490, #31323, #35213 ) ) REPRESENTATION_CONTEXT ( 'NONE', 'WORKASPACE' ) );
#9329 = ORIENTED_EDGE ( 'NONE', *, *, #27901, .T. ) ;
#9330 = CARTESIAN_POINT ( 'NONE',  ( -10.00000000000000000, 0.000000000000000000, 0.000000000000000000 ) ) ;
#9331 = EDGE_CURVE ( 'NONE', #38290, #46458, #9638, .T. ) ;
#9332 = CARTESIAN_POINT ( 'NONE',  ( 0.000000000000000000, -16.23288003029521320, 33.80338159004277543 ) ) ;
#9333 = CONTEXT_DEPENDENT_SHAPE_REPRESENTATION ( #18198, #3471 ) ;
#9334 = EDGE_CURVE ( 'NONE', #19886, #43803, #1050, .T. ) ;
#9335 = CYLINDRICAL_SURFACE ( 'NONE', #26055, 31.99999999999998579 ) ;
#9336 = ORIENTED_EDGE ( 'NONE', *, *, #15758, .F. ) ;
#9337 = EDGE_CURVE ( 'NONE', #29279, #34549, #21810, .T. ) ;
#9338 = VECTOR ( 'NONE', #25504, 1000.000000000000000 ) ;
#9339 = EDGE_CURVE ( 'NONE', #40104, #8546, #3199, .T. ) ;
#9340 = DIRECTION ( 'NONE',  ( 1.000000000000000000, -0.000000000000000000, -0.000000000000000000 ) ) ;
#9341 = VERTEX_POINT ( 'NONE', #18127 ) ;
#9342 = CARTESIAN_POINT ( 'NONE',  ( 15.00000000000000000, -13.04903810567675393, -19.60159698893424718 ) ) ;
#9343 = ORIENTED_EDGE ( 'NONE', *, *, #7421, .F. ) ;
#9344 =( LENGTH_UNIT ( ) NAMED_UNIT ( * ) SI_UNIT ( .MILLI., .METRE. ) );
#9345 = CARTESIAN_POINT ( 'NONE',  ( 0.000000000000000000, 44.99326035066149387, -68.55367621811095091 ) ) ;
#9346 = VECTOR ( 'NONE', #23683, 1000.000000000000000 ) ;
#9347 = CARTESIAN_POINT ( 'NONE',  ( 0.000000000000000000, 0.000000000000000000, 0.000000000000000000 ) ) ;
#9348 = ORIENTED_EDGE ( 'NONE', *, *, #10374, .F. ) ;
#9350 = EDGE_LOOP ( 'NONE', ( #30926, #21246, #23950, #41986 ) ) ;
#9349 = DIRECTION ( 'NONE',  ( 1.000000000000000000, 0.000000000000000000, 0.000000000000000000 ) ) ;
#9351 = EDGE_LOOP ( 'NONE', ( #31272, #27537, #9240, #46200 ) ) ;
#9352 = VERTEX_POINT ( 'NONE', #3945 ) ;
#9353 = CARTESIAN_POINT ( 'NONE',  ( 0.000000000000000000, 0.000000000000000000, 0.000000000000000000 ) ) ;
#9354 = CARTESIAN_POINT ( 'NONE',  ( -3.000000000000000000, 16.83928648764923253, 16.46020748918050458 ) ) ;
#9355 = DIRECTION ( 'NONE',  ( 0.000000000000000000, 0.000000000000000000, 1.000000000000000000 ) ) ;
#9356 = CARTESIAN_POINT ( 'NONE',  ( 0.000000000000000000, 58.39081064771823293, -50.95692526931266286 ) ) ;
#9357 = DIRECTION ( 'NONE',  ( -1.000000000000000000, -0.000000000000000000, -0.000000000000000000 ) ) ;
#9358 = ORIENTED_EDGE ( 'NONE', *, *, #22674, .T. ) ;
#9359 = DIRECTION ( 'NONE',  ( -1.000000000000000000, -0.000000000000000000, 0.000000000000000000 ) ) ;
#9360 = ORIENTED_EDGE ( 'NONE', *, *, #35594, .T. ) ;
#9361 = DIRECTION ( 'NONE',  ( 0.000000000000000000, -0.1564344650402170189, -0.9876883405951399908 ) ) ;
#9362 = ORIENTED_EDGE ( 'NONE', *, *, #38916, .F. ) ;
#9363 = DIRECTION ( 'NONE',  ( -1.000000000000000000, 0.000000000000000000, 0.000000000000000000 ) ) ;
#9364 = DIRECTION ( 'NONE',  ( -1.000000000000000000, 0.000000000000000000, 0.000000000000000000 ) ) ;
#9365 = PLANE ( 'NONE',  #9442 ) ;
#9366 = ORIENTED_EDGE ( 'NONE', *, *, #17209, .F. ) ;
#9367 = CARTESIAN_POINT ( 'NONE',  ( 0.000000000000000000, 39.47590169984944453, -71.87247863392373404 ) ) ;
#9368 = CARTESIAN_POINT ( 'NONE',  ( 11.99999999999999822, 46.53671651294032330, -59.03961581697353012 ) ) ;
#9369 = CARTESIAN_POINT ( 'NONE',  ( 0.000000000000000000, 0.000000000000000000, 0.000000000000000000 ) ) ;
#9370 = DIRECTION ( 'NONE',  ( 0.000000000000000000, 0.000000000000000000, 1.000000000000000000 ) ) ;
#9372 = VECTOR ( 'NONE', #44771, 1000.000000000000000 ) ;
#9371 = DIRECTION ( 'NONE',  ( 0.000000000000000000, 0.5877852522924743583, -0.8090169943749466741 ) ) ;
#9373 = CIRCLE ( 'NONE', #44551, 31.99999999999999289 ) ;
#9374 = DIRECTION ( 'NONE',  ( 0.000000000000000000, -6.938893903907228378E-15, 1.000000000000000000 ) ) ;
#9375 = CARTESIAN_POINT ( 'NONE',  ( 11.99999999999999822, -2.543863470248965086, 81.96053171279902472 ) ) ;
#9376 = CYLINDRICAL_SURFACE ( 'NONE', #31040, 32.00000000000000000 ) ;
#9377 = AXIS2_PLACEMENT_3D ( 'NONE', #41868, #30124, #38422 ) ;
#9378 = DIRECTION ( 'NONE',  ( 0.000000000000000000, 0.000000000000000000, 1.000000000000000000 ) ) ;
#9379 = CYLINDRICAL_SURFACE ( 'NONE', #33895, 77.49899999999999523 ) ;
#9380 = CIRCLE ( 'NONE', #36725, 31.99999999999999645 ) ;
#9381 = ORIENTED_EDGE ( 'NONE', *, *, #34237, .F. ) ;
#9382 = DIRECTION ( 'NONE',  ( -1.000000000000000000, 0.000000000000000000, 0.000000000000000000 ) ) ;
#9383 = VECTOR ( 'NONE', #41398, 1000.000000000000000 ) ;
#9384 = VERTEX_POINT ( 'NONE', #33785 ) ;
#9385 = EDGE_CURVE ( 'NONE', #39461, #25221, #38385, .T. ) ;
#9386 = CARTESIAN_POINT ( 'NONE',  ( 10.00000000000000000, -71.27951684758005513, -30.41916302227188851 ) ) ;
#9387 = EDGE_CURVE ( 'NONE', #9910, #1345, #36199, .T. ) ;
#9388 = DIRECTION ( 'NONE',  ( 0.000000000000000000, 0.000000000000000000, 1.000000000000000000 ) ) ;
#9389 = ORIENTED_EDGE ( 'NONE', *, *, #42255, .T. ) ;
#9390 = EDGE_CURVE ( 'NONE', #19610, #8099, #2582, .T. ) ;
#9391 = CARTESIAN_POINT ( 'NONE',  ( -10.00000000000000000, 0.000000000000000000, 0.000000000000000000 ) ) ;
#9393 = ADVANCED_FACE ( 'NONE', ( #36735 ), #33068, .T. ) ;
#9392 = ORIENTED_EDGE ( 'NONE', *, *, #41507, .F. ) ;
#9394 = VERTEX_POINT ( 'NONE', #18625 ) ;
#9395 = VECTOR ( 'NONE', #15796, 1000.000000000000000 ) ;
#9396 = CARTESIAN_POINT ( 'NONE',  ( 15.00000000000000000, -13.04903810567646971, 19.60159698893442481 ) ) ;
#9397 = CARTESIAN_POINT ( 'NONE',  ( -10.00000000000000000, 0.000000000000000000, 0.000000000000000000 ) ) ;
#9399 = ORIENTED_EDGE ( 'NONE', *, *, #22398, .F. ) ;
#9398 = DIRECTION ( 'NONE',  ( -1.000000000000000000, -0.000000000000000000, -0.000000000000000000 ) ) ;
#9400 = AXIS2_PLACEMENT_3D ( 'NONE', #25554, #17962, #40501 ) ;
#9401 = CIRCLE ( 'NONE', #36763, 31.99999999999999645 ) ;
#9402 = EDGE_CURVE ( 'NONE', #38262, #43286, #11200, .T. ) ;
#9403 = EDGE_LOOP ( 'NONE', ( #21580, #2788, #20525, #9200 ) ) ;
#9404 = CARTESIAN_POINT ( 'NONE',  ( 10.00000000000000000, 0.000000000000000000, 0.000000000000000000 ) ) ;
#9405 = ORIENTED_EDGE ( 'NONE', *, *, #2913, .F. ) ;
#9406 = ORIENTED_EDGE ( 'NONE', *, *, #24489, .T. ) ;
#9407 = AXIS2_PLACEMENT_3D ( 'NONE', #24612, #32664, #39787 ) ;
#9408 = CARTESIAN_POINT ( 'NONE',  ( 5.000000000000000000, 36.13751322684419165, 21.40280677340384585 ) ) ;
#9409 = CARTESIAN_POINT ( 'NONE',  ( 10.00000000000000000, 0.000000000000000000, 0.000000000000000000 ) ) ;
#9410 = AXIS2_PLACEMENT_3D ( 'NONE', #1790, #42422, #1055 ) ;
#9411 = CARTESIAN_POINT ( 'NONE',  ( 0.000000000000000000, 0.000000000000000000, 0.000000000000000000 ) ) ;
#9412 = VERTEX_POINT ( 'NONE', #18386 ) ;
#9413 = ORIENTED_EDGE ( 'NONE', *, *, #14816, .T. ) ;
#9414 = CIRCLE ( 'NONE', #4745, 77.49900000000000944 ) ;
#9415 = CYLINDRICAL_SURFACE ( 'NONE', #41966, 31.99999999999998579 ) ;
#9416 = EDGE_LOOP ( 'NONE', ( #27642, #27614, #22883, #44329 ) ) ;
#9417 = FACE_BOUND ( 'NONE', #32242, .T. ) ;
#9418 = CARTESIAN_POINT ( 'NONE',  ( 0.000000000000000000, 71.91182617369187824, 28.89263327155772387 ) ) ;
#9419 = CARTESIAN_POINT ( 'NONE',  ( 0.000000000000000000, -11.30684508768393570, 76.66974797899831628 ) ) ;
#9420 = CARTESIAN_POINT ( 'NONE',  ( 4.999999999999999112, -9.188173127307592836, 40.98264845739746676 ) ) ;
#9421 = DIRECTION ( 'NONE',  ( 0.000000000000000000, 0.7431448254773954654, 0.6691306063588569053 ) ) ;
#9422 = CYLINDRICAL_SURFACE ( 'NONE', #31492, 77.49899999999999523 ) ;
#9423 =( NAMED_UNIT ( * ) PLANE_ANGLE_UNIT ( ) SI_UNIT ( $, .RADIAN. ) );
#9424 = DIRECTION ( 'NONE',  ( 1.000000000000000000, 0.000000000000000000, 0.000000000000000000 ) ) ;
#9425 = CARTESIAN_POINT ( 'NONE',  ( 5.000000000000000000, 31.52238457039637609, -27.75498641678709788 ) ) ;
#9426 = FACE_OUTER_BOUND ( 'NONE', #10704, .T. ) ;
#9427 = EDGE_CURVE ( 'NONE', #44447, #4582, #48248, .T. ) ;
#9428 = ORIENTED_EDGE ( 'NONE', *, *, #19533, .F. ) ;
#9429 = DIRECTION ( 'NONE',  ( -1.000000000000000000, -0.000000000000000000, 0.000000000000000000 ) ) ;
#9430 = EDGE_CURVE ( 'NONE', #12321, #7133, #44571, .T. ) ;
#9431 = FACE_OUTER_BOUND ( 'NONE', #19223, .T. ) ;
#9432 = DIRECTION ( 'NONE',  ( -0.9730327541852491491, 0.2306669878475648139, 0.000000000000000000 ) ) ;
#9433 = EDGE_CURVE ( 'NONE', #5603, #42611, #13, .T. ) ;
#9434 = DIRECTION ( 'NONE',  ( -1.000000000000000000, 0.000000000000000000, -0.000000000000000000 ) ) ;
#9435 = DIRECTION ( 'NONE',  ( 0.000000000000000000, -0.1045284632676558301, -0.9945218953682731788 ) ) ;
#9436 = AXIS2_PLACEMENT_3D ( 'NONE', #589, #34112, #29483 ) ;
#9437 = DIRECTION ( 'NONE',  ( -1.000000000000000000, -0.000000000000000000, 0.000000000000000000 ) ) ;
#9438 = DIRECTION ( 'NONE',  ( -1.000000000000000000, 0.000000000000000000, 0.000000000000000000 ) ) ;
#9439 = AXIS2_PLACEMENT_3D ( 'NONE', #32010, #17285, #9465 ) ;
#9440 = ORIENTED_EDGE ( 'NONE', *, *, #317, .T. ) ;
#9441 = DIRECTION ( 'NONE',  ( 0.000000000000000000, 0.000000000000000000, -1.000000000000000000 ) ) ;
#9442 = AXIS2_PLACEMENT_3D ( 'NONE', #34834, #39000, #12812 ) ;
#9443 = CIRCLE ( 'NONE', #36032, 12.49999999999999822 ) ;
#9444 = EDGE_LOOP ( 'NONE', ( #34766, #16410, #35822, #4305 ) ) ;
#9445 = EDGE_CURVE ( 'NONE', #36193, #30385, #23687, .T. ) ;
#9446 = DIRECTION ( 'NONE',  ( 0.000000000000000000, 0.000000000000000000, 1.000000000000000000 ) ) ;
#9447 = VECTOR ( 'NONE', #39709, 1000.000000000000000 ) ;
#9448 = EDGE_CURVE ( 'NONE', #19576, #9873, #12004, .T. ) ;
#9449 = EDGE_CURVE ( 'NONE', #17019, #39073, #46936, .T. ) ;
#9450 = VERTEX_POINT ( 'NONE', #5104 ) ;
#9451 = ORIENTED_EDGE ( 'NONE', *, *, #12425, .F. ) ;
#9452 = AXIS2_PLACEMENT_3D ( 'NONE', #29109, #39678, #2677 ) ;
#9453 = AXIS2_PLACEMENT_3D ( 'NONE', #3885, #30815, #45740 ) ;
#9454 = ORIENTED_EDGE ( 'NONE', *, *, #40118, .F. ) ;
#9455 = EDGE_CURVE ( 'NONE', #2177, #41443, #24506, .T. ) ;
#9456 = CARTESIAN_POINT ( 'NONE',  ( -3.249999999999999556, -13.95926121303099343, -1.199999999999999956 ) ) ;
#9457 = ORIENTED_EDGE ( 'NONE', *, *, #6131, .T. ) ;
#9458 = ORIENTED_EDGE ( 'NONE', *, *, #32634, .T. ) ;
#9459 = DIRECTION ( 'NONE',  ( -1.000000000000000000, 0.000000000000000000, 0.000000000000000000 ) ) ;
#9461 = ORIENTED_EDGE ( 'NONE', *, *, #39525, .F. ) ;
#9460 = DIRECTION ( 'NONE',  ( -1.000000000000000000, 0.000000000000000000, 0.000000000000000000 ) ) ;
#9462 = ORIENTED_EDGE ( 'NONE', *, *, #13042, .T. ) ;
#9463 = ORIENTED_EDGE ( 'NONE', *, *, #28954, .F. ) ;
#9464 = DIRECTION ( 'NONE',  ( -1.000000000000000000, -0.000000000000000000, 0.000000000000000000 ) ) ;
#9466 = ORIENTED_EDGE ( 'NONE', *, *, #8681, .T. ) ;
#9465 = DIRECTION ( 'NONE',  ( 0.000000000000000000, 0.000000000000000000, -1.000000000000000000 ) ) ;
#9467 = VECTOR ( 'NONE', #23762, 1000.000000000000000 ) ;
#9468 = CARTESIAN_POINT ( 'NONE',  ( 10.00000000000000000, 21.53537804866126137, -30.80686688396986028 ) ) ;
#9469 = EDGE_LOOP ( 'NONE', ( #26020, #32357, #4293, #17051 ) ) ;
#9470 = EDGE_LOOP ( 'NONE', ( #31667, #7250, #45533, #44943 ) ) ;
#9471 = DIRECTION ( 'NONE',  ( 0.000000000000000000, 0.000000000000000000, 1.000000000000000000 ) ) ;
#9472 = ORIENTED_EDGE ( 'NONE', *, *, #43262, .T. ) ;
#9473 = CYLINDRICAL_SURFACE ( 'NONE', #23603, 37.49900000000000233 ) ;
#9474 = VECTOR ( 'NONE', #24473, 999.9999999999998863 ) ;
#9475 = CARTESIAN_POINT ( 'NONE',  ( -2.499999999999997780, 8.494897427831771708, -10.00000000000000178 ) ) ;
#9476 = LINE ( 'NONE', #23686, #28349 ) ;
#9477 = DIRECTION ( 'NONE',  ( 0.000000000000000000, 0.000000000000000000, 1.000000000000000000 ) ) ;
#9478 = CARTESIAN_POINT ( 'NONE',  ( 12.69589495141918611, -96.69089767102708777, -2.500000000000000444 ) ) ;
#9479 = ORIENTED_EDGE ( 'NONE', *, *, #3491, .T. ) ;
#9480 = AXIS2_PLACEMENT_3D ( 'NONE', #21037, #17844, #5893 ) ;
#9481 = ORIENTED_EDGE ( 'NONE', *, *, #17819, .T. ) ;
#9482 = EDGE_CURVE ( 'NONE', #26885, #31737, #23699, .T. ) ;
#9483 = CARTESIAN_POINT ( 'NONE',  ( 10.00000000000000000, -22.64427369931191336, 30.00120703465197280 ) ) ;
#9484 = DIRECTION ( 'NONE',  ( -1.000000000000000000, -0.000000000000000000, 0.000000000000000000 ) ) ;
#9485 = EDGE_CURVE ( 'NONE', #36993, #43390, #3378, .T. ) ;
#9486 = VERTEX_POINT ( 'NONE', #23946 ) ;
#9487 = CARTESIAN_POINT ( 'NONE',  ( 0.000000000000000000, -15.48615015657610527, 39.04073710021338428 ) ) ;
#9488 = EDGE_LOOP ( 'NONE', ( #40490, #37692, #35106, #4824 ) ) ;
#9489 = AXIS2_PLACEMENT_3D ( 'NONE', #4896, #31106, #12495 ) ;
#9490 = ADVANCED_FACE ( 'NONE', ( #13404 ), #47171, .T. ) ;
#9491 = LINE ( 'NONE', #27623, #38704 ) ;
#9492 = DIRECTION ( 'NONE',  ( 0.9435911131814402886, -0.3311129884571281101, 0.000000000000000000 ) ) ;
#9493 = DIRECTION ( 'NONE',  ( -0.000000000000000000, -0.3090169943749573878, 0.9510565162951503115 ) ) ;
#9494 = FACE_OUTER_BOUND ( 'NONE', #7832, .T. ) ;
#9495 = EDGE_CURVE ( 'NONE', #40832, #26882, #8847, .T. ) ;
#9496 = CYLINDRICAL_SURFACE ( 'NONE', #14005, 16.00000000000000000 ) ;
#9497 = CARTESIAN_POINT ( 'NONE',  ( 10.00000000000000000, 0.000000000000000000, 0.000000000000000000 ) ) ;
#9498 = MECHANICAL_DESIGN_GEOMETRIC_PRESENTATION_REPRESENTATION (  '', ( #14180 ), #43704 ) ;
#9499 = ORIENTED_EDGE ( 'NONE', *, *, #47840, .T. ) ;
#9500 = CARTESIAN_POINT ( 'NONE',  ( 0.000000000000000000, 0.000000000000000000, 0.000000000000000000 ) ) ;
#9501 = CARTESIAN_POINT ( 'NONE',  ( 0.000000000000000000, 22.90783923731629201, 78.73519480814962890 ) ) ;
#9502 = DIRECTION ( 'NONE',  ( -1.000000000000000000, 0.000000000000000000, 0.000000000000000000 ) ) ;
#9503 = DIRECTION ( 'NONE',  ( -1.000000000000000000, -0.000000000000000000, -0.000000000000000000 ) ) ;
#9504 = PRESENTATION_STYLE_ASSIGNMENT (( #28351 ) ) ;
#9505 = EDGE_CURVE ( 'NONE', #38979, #10399, #24411, .T. ) ;
#9506 = VERTEX_POINT ( 'NONE', #2370 ) ;
#9507 = VECTOR ( 'NONE', #37295, 1000.000000000000114 ) ;
#9508 = DIRECTION ( 'NONE',  ( 0.000000000000000000, 0.3090169943749482839, -0.9510565162951533091 ) ) ;
#9509 = AXIS2_PLACEMENT_3D ( 'NONE', #39245, #35084, #46346 ) ;
#9510 = DIRECTION ( 'NONE',  ( 0.000000000000000000, 0.000000000000000000, 1.000000000000000000 ) ) ;
#9511 = ORIENTED_EDGE ( 'NONE', *, *, #7555, .F. ) ;
#9512 = AXIS2_PLACEMENT_3D ( 'NONE', #18527, #11910, #27562 ) ;
#9513 = EDGE_CURVE ( 'NONE', #48194, #13671, #28579, .T. ) ;
#9514 = LINE ( 'NONE', #2186, #10885 ) ;
#9515 = DIRECTION ( 'NONE',  ( -1.000000000000000000, -0.000000000000000000, -0.000000000000000000 ) ) ;
#9516 = AXIS2_PLACEMENT_3D ( 'NONE', #6590, #10253, #40127 ) ;
#9517 = VERTEX_POINT ( 'NONE', #38641 ) ;
#9518 = VERTEX_POINT ( 'NONE', #20018 ) ;
#9519 = VERTEX_POINT ( 'NONE', #35183 ) ;
#9520 = DIRECTION ( 'NONE',  ( -0.000000000000000000, -0.9510565162951506446, -0.3090169943749562220 ) ) ;
#9521 = ORIENTED_EDGE ( 'NONE', *, *, #4749, .T. ) ;
#9522 = ORIENTED_EDGE ( 'NONE', *, *, #43101, .F. ) ;
#9523 = CARTESIAN_POINT ( 'NONE',  ( 13.83832728059186046, -142.6495187161941089, 2.500000000000000000 ) ) ;
#9524 = ORIENTED_EDGE ( 'NONE', *, *, #6143, .F. ) ;
#9525 = PLANE ( 'NONE',  #3228 ) ;
#9526 = DIRECTION ( 'NONE',  ( -1.000000000000000000, -0.000000000000000000, -0.000000000000000000 ) ) ;
#9527 = CARTESIAN_POINT ( 'NONE',  ( 10.00000000000000000, 0.000000000000000000, 0.000000000000000000 ) ) ;
#9528 = ORIENTED_EDGE ( 'NONE', *, *, #18463, .F. ) ;
#9529 = CARTESIAN_POINT ( 'NONE',  ( -26.41226275915097332, -122.1546173538626761, -2.500000000000000000 ) ) ;
#9530 = ORIENTED_EDGE ( 'NONE', *, *, #32231, .T. ) ;
#9531 = AXIS2_PLACEMENT_3D ( 'NONE', #29725, #44422, #37070 ) ;
#9532 = LINE ( 'NONE', #46768, #7072 ) ;
#9533 = DIRECTION ( 'NONE',  ( 0.000000000000000000, -0.5877852522924797984, -0.8090169943749426773 ) ) ;
#9534 = DIRECTION ( 'NONE',  ( -1.000000000000000000, 0.000000000000000000, 0.000000000000000000 ) ) ;
#9535 = ORIENTED_EDGE ( 'NONE', *, *, #31745, .F. ) ;
#9536 = ORIENTED_EDGE ( 'NONE', *, *, #31691, .F. ) ;
#9537 = DIRECTION ( 'NONE',  ( 0.000000000000000000, 0.5224985647159500202, -0.8526401643540915121 ) ) ;
#9538 = CYLINDRICAL_SURFACE ( 'NONE', #43397, 42.00000000000000000 ) ;
#9539 = ORIENTED_EDGE ( 'NONE', *, *, #2701, .F. ) ;
#9540 = CIRCLE ( 'NONE', #47081, 12.49999999999999645 ) ;
#9541 = EDGE_CURVE ( 'NONE', #41064, #36905, #34612, .T. ) ;
#9542 = CARTESIAN_POINT ( 'NONE',  ( 10.00000000000000000, -38.55633173626998911, -16.65560815589452304 ) ) ;
#9543 = FACE_OUTER_BOUND ( 'NONE', #18309, .T. ) ;
#9544 = CYLINDRICAL_SURFACE ( 'NONE', #19086, 42.00000000000000000 ) ;
#9545 = CARTESIAN_POINT ( 'NONE',  ( 11.99999999999999822, 0.000000000000000000, 0.000000000000000000 ) ) ;
#9546 = EDGE_CURVE ( 'NONE', #35770, #33176, #31295, .T. ) ;
#9547 = CIRCLE ( 'NONE', #35338, 16.00000000000000000 ) ;
#9548 = CYLINDRICAL_SURFACE ( 'NONE', #31819, 31.99999999999998579 ) ;
#9549 = CARTESIAN_POINT ( 'NONE',  ( 10.00000000000000000, 2.956366410620650420, 75.11725578898469280 ) ) ;
#9550 = LINE ( 'NONE', #46541, #4415 ) ;
#9551 = VECTOR ( 'NONE', #7221, 1000.000000000000000 ) ;
#9552 = DIRECTION ( 'NONE',  ( -0.000000000000000000, 0.9781476007338042455, -0.2079116908177663092 ) ) ;
#9553 = FACE_OUTER_BOUND ( 'NONE', #39754, .T. ) ;
#9554 = CARTESIAN_POINT ( 'NONE',  ( 16.84844760790522855, -103.5491698323862124, 5.500000000000000000 ) ) ;
#9555 = CARTESIAN_POINT ( 'NONE',  ( 15.00000000000000000, -14.54903810567676636, -22.19967320028755964 ) ) ;
#9556 = DIRECTION ( 'NONE',  ( 0.000000000000000000, 0.000000000000000000, 1.000000000000000000 ) ) ;
#9557 = VERTEX_POINT ( 'NONE', #1919 ) ;
#9558 = EDGE_CURVE ( 'NONE', #31834, #34210, #28377, .T. ) ;
#9559 = DIRECTION ( 'NONE',  ( 0.000000000000000000, 0.000000000000000000, -1.000000000000000000 ) ) ;
#9560 = ADVANCED_FACE ( 'NONE', ( #9246 ), #24179, .T. ) ;
#9561 = LINE ( 'NONE', #6153, #42454 ) ;
#9562 = CIRCLE ( 'NONE', #43186, 82.00000000000000000 ) ;
#9563 = DIRECTION ( 'NONE',  ( -1.000000000000000000, 0.000000000000000000, -0.000000000000000000 ) ) ;
#9564 = ORIENTED_EDGE ( 'NONE', *, *, #41029, .T. ) ;
#9565 = EDGE_CURVE ( 'NONE', #5351, #908, #6510, .T. ) ;
#9566 = VERTEX_POINT ( 'NONE', #31792 ) ;
#9567 = VECTOR ( 'NONE', #40444, 1000.000000000000000 ) ;
#9568 = CARTESIAN_POINT ( 'NONE',  ( -10.00000000000000000, 0.000000000000000000, 0.000000000000000000 ) ) ;
#9569 = VECTOR ( 'NONE', #6593, 1000.000000000000000 ) ;
#9570 = EDGE_LOOP ( 'NONE', ( #44078, #11726, #14167, #23241 ) ) ;
#9571 = LINE ( 'NONE', #13033, #25298 ) ;
#9572 = CIRCLE ( 'NONE', #36170, 77.49899999999999523 ) ;
#9573 = ORIENTED_EDGE ( 'NONE', *, *, #4151, .F. ) ;
#9574 = LINE ( 'NONE', #20854, #3144 ) ;
#9575 = VECTOR ( 'NONE', #13066, 1000.000000000000000 ) ;
#9576 = CARTESIAN_POINT ( 'NONE',  ( 5.000000000000000000, 67.80270845531956070, -46.11716303203112943 ) ) ;
#9577 = AXIS2_PLACEMENT_3D ( 'NONE', #44649, #21885, #40736 ) ;
#9578 = DIRECTION ( 'NONE',  ( 0.000000000000000000, 0.000000000000000000, 1.000000000000000000 ) ) ;
#9579 = VERTEX_POINT ( 'NONE', #46706 ) ;
#9581 = ORIENTED_EDGE ( 'NONE', *, *, #30622, .F. ) ;
#9580 = CYLINDRICAL_SURFACE ( 'NONE', #21543, 32.00000000000000000 ) ;
#9582 = CIRCLE ( 'NONE', #40107, 77.49900000000000944 ) ;
#9583 = EDGE_LOOP ( 'NONE', ( #8971, #32310, #23132, #38544 ) ) ;
#9584 = DIRECTION ( 'NONE',  ( -0.1850432970638682395, 0.9827303690289280746, 0.000000000000000000 ) ) ;
#9585 = CARTESIAN_POINT ( 'NONE',  ( 0.000000000000000000, 22.07842321921492612, -8.187992925817130896 ) ) ;
#9586 = DIRECTION ( 'NONE',  ( -1.000000000000000000, 0.000000000000000000, -0.000000000000000000 ) ) ;
#9587 = DIRECTION ( 'NONE',  ( 1.000000000000000000, 0.000000000000000000, 0.000000000000000000 ) ) ;
#9588 = DIRECTION ( 'NONE',  ( -1.000000000000000000, -0.000000000000000000, -0.000000000000000000 ) ) ;
#9589 = EDGE_LOOP ( 'NONE', ( #30946, #26571, #23977, #47289 ) ) ;
#9590 = CARTESIAN_POINT ( 'NONE',  ( 5.000000000000000000, 59.75363087400153006, -56.15606465354897381 ) ) ;
#9591 = ORIENTED_EDGE ( 'NONE', *, *, #37247, .T. ) ;
#9592 = ORIENTED_EDGE ( 'NONE', *, *, #6096, .T. ) ;
#9593 = EDGE_CURVE ( 'NONE', #8938, #28565, #19773, .T. ) ;
#9594 = LINE ( 'NONE', #28453, #25383 ) ;
#9595 = ORIENTED_EDGE ( 'NONE', *, *, #26268, .T. ) ;
#9596 = EDGE_CURVE ( 'NONE', #7880, #13054, #19009, .T. ) ;
#9597 = DIRECTION ( 'NONE',  ( 0.000000000000000000, -0.3090169943749549453, 0.9510565162951511997 ) ) ;
#9598 = CARTESIAN_POINT ( 'NONE',  ( 11.99999999999999822, 59.03342792756263435, 46.54456581323825048 ) ) ;
#9599 = DIRECTION ( 'NONE',  ( 1.000000000000000000, -0.000000000000000000, -0.000000000000000000 ) ) ;
#9600 = EDGE_LOOP ( 'NONE', ( #28130, #734, #33604, #12330 ) ) ;
#9601 = CARTESIAN_POINT ( 'NONE',  ( 0.000000000000000000, -0.8299999999999999600, -1.199999999999999956 ) ) ;
#9602 = CARTESIAN_POINT ( 'NONE',  ( 10.00000000000000000, 0.000000000000000000, 0.000000000000000000 ) ) ;
#9603 = EDGE_CURVE ( 'NONE', #18852, #11835, #44230, .T. ) ;
#9604 = DIRECTION ( 'NONE',  ( 0.000000000000000000, -0.1564344650402170744, -0.9876883405951398798 ) ) ;
#9605 = AXIS2_PLACEMENT_3D ( 'NONE', #2451, #36227, #43582 ) ;
#9606 = PLANE ( 'NONE',  #45530 ) ;
#9607 = CARTESIAN_POINT ( 'NONE',  ( 10.00000000000000000, 0.8261519478431083030, 77.49459641780886443 ) ) ;
#9608 = EDGE_CURVE ( 'NONE', #38886, #12494, #16684, .T. ) ;
#9609 = CARTESIAN_POINT ( 'NONE',  ( 11.99999999999999822, 80.55351364060588537, 15.33399622253511829 ) ) ;
#9611 = ADVANCED_FACE ( 'NONE', ( #2862 ), #25845, .T. ) ;
#9610 = SURFACE_SIDE_STYLE ('',( #43162 ) ) ;
#9612 = DIRECTION ( 'NONE',  ( -1.000000000000000000, -0.000000000000000000, -0.000000000000000000 ) ) ;
#9613 = DIRECTION ( 'NONE',  ( 0.000000000000000000, 0.000000000000000000, 1.000000000000000000 ) ) ;
#9614 = VECTOR ( 'NONE', #2860, 1000.000000000000000 ) ;
#9615 = CARTESIAN_POINT ( 'NONE',  ( 0.000000000000000000, 44.88180994100376608, 63.18004540533043922 ) ) ;
#9616 = DIRECTION ( 'NONE',  ( 0.000000000000000000, 0.000000000000000000, 1.000000000000000000 ) ) ;
#9617 = AXIS2_PLACEMENT_3D ( 'NONE', #22265, #37190, #3659 ) ;
#9618 = VERTEX_POINT ( 'NONE', #25127 ) ;
#9619 = FACE_OUTER_BOUND ( 'NONE', #42705, .T. ) ;
#9620 = AXIS2_PLACEMENT_3D ( 'NONE', #39003, #35571, #16728 ) ;
#9621 = ORIENTED_EDGE ( 'NONE', *, *, #25340, .T. ) ;
#9622 = LINE ( 'NONE', #9878, #40087 ) ;
#9623 = VECTOR ( 'NONE', #14033, 1000.000000000000000 ) ;
#9624 = DIRECTION ( 'NONE',  ( -1.000000000000000000, -0.000000000000000000, -0.000000000000000000 ) ) ;
#9625 = VERTEX_POINT ( 'NONE', #36866 ) ;
#9626 = EDGE_CURVE ( 'NONE', #38560, #2609, #47640, .T. ) ;
#9627 = CARTESIAN_POINT ( 'NONE',  ( 11.99999999999999822, 0.000000000000000000, 0.000000000000000000 ) ) ;
#9628 = ORIENTED_EDGE ( 'NONE', *, *, #17391, .F. ) ;
#9629 = EDGE_CURVE ( 'NONE', #19662, #5981, #25286, .T. ) ;
#9630 = ORIENTED_EDGE ( 'NONE', *, *, #17748, .F. ) ;
#9631 = VECTOR ( 'NONE', #32518, 1000.000000000000000 ) ;
#9632 = ADVANCED_FACE ( 'NONE', ( #6301 ), #18264, .T. ) ;
#9633 = ORIENTED_EDGE ( 'NONE', *, *, #2817, .T. ) ;
#9634 = DIRECTION ( 'NONE',  ( -1.000000000000000000, 0.000000000000000000, 0.000000000000000000 ) ) ;
#9635 = ORIENTED_EDGE ( 'NONE', *, *, #4805, .F. ) ;
#9636 = CYLINDRICAL_SURFACE ( 'NONE', #37506, 37.49900000000000233 ) ;
#9637 = VECTOR ( 'NONE', #29240, 1000.000000000000000 ) ;
#9638 = CIRCLE ( 'NONE', #8072, 77.49899999999999523 ) ;
#9639 = CARTESIAN_POINT ( 'NONE',  ( 0.000000000000000000, -0.8299999999999999600, -1.199999999999999956 ) ) ;
#9640 = CIRCLE ( 'NONE', #37006, 17.30399999999999849 ) ;
#9641 = ORIENTED_EDGE ( 'NONE', *, *, #23582, .T. ) ;
#9642 = CARTESIAN_POINT ( 'NONE',  ( 4.999999999999999112, -2.663952781845850826, -41.91543099594819921 ) ) ;
#9643 = AXIS2_PLACEMENT_3D ( 'NONE', #17597, #10751, #7060 ) ;
#9644 = VERTEX_POINT ( 'NONE', #40792 ) ;
#9645 = AXIS2_PLACEMENT_3D ( 'NONE', #6029, #6496, #28998 ) ;
#9646 = ORIENTED_EDGE ( 'NONE', *, *, #27366, .T. ) ;
#9647 = FACE_OUTER_BOUND ( 'NONE', #36908, .T. ) ;
#9648 = DIRECTION ( 'NONE',  ( -0.2079116908177431888, 0.000000000000000000, 0.9781476007338091305 ) ) ;
#9649 = CARTESIAN_POINT ( 'NONE',  ( 0.000000000000000000, 36.13751322684449008, -21.40280677340332716 ) ) ;
#9650 = EDGE_CURVE ( 'NONE', #34450, #12269, #9685, .T. ) ;
#9651 = AXIS2_PLACEMENT_3D ( 'NONE', #46959, #5855, #21004 ) ;
#9652 = AXIS2_PLACEMENT_3D ( 'NONE', #47383, #17750, #5780 ) ;
#9653 = ORIENTED_EDGE ( 'NONE', *, *, #28013, .F. ) ;
#9654 = ORIENTED_EDGE ( 'NONE', *, *, #15439, .F. ) ;
#9655 = DIRECTION ( 'NONE',  ( 0.000000000000000000, 0.2334453638559058908, -0.9723699203976765570 ) ) ;
#9656 = ORIENTED_EDGE ( 'NONE', *, *, #8742, .T. ) ;
#9657 = AXIS2_PLACEMENT_3D ( 'NONE', #44586, #23041, #41180 ) ;
#9658 = EDGE_CURVE ( 'NONE', #19451, #13273, #15956, .T. ) ;
#9659 = FACE_BOUND ( 'NONE', #37760, .T. ) ;
#9660 = CIRCLE ( 'NONE', #24565, 77.49900000000000944 ) ;
#9661 = CARTESIAN_POINT ( 'NONE',  ( 10.00000000000000000, 0.000000000000000000, 0.000000000000000000 ) ) ;
#9662 = DIRECTION ( 'NONE',  ( 1.000000000000000000, 0.000000000000000000, 0.000000000000000000 ) ) ;
#9663 = DIRECTION ( 'NONE',  ( 1.000000000000000000, 0.000000000000000000, 0.000000000000000000 ) ) ;
#9664 = EDGE_CURVE ( 'NONE', #19091, #16230, #12051, .T. ) ;
#9665 = CYLINDRICAL_SURFACE ( 'NONE', #37814, 82.00000000000000000 ) ;
#9666 = AXIS2_PLACEMENT_3D ( 'NONE', #9894, #42459, #35103 ) ;
#9667 = CARTESIAN_POINT ( 'NONE',  ( 10.00000000000000000, 0.000000000000000000, 0.000000000000000000 ) ) ;
#9668 = DIRECTION ( 'NONE',  ( -1.000000000000000000, 0.000000000000000000, 0.000000000000000000 ) ) ;
#9669 = CARTESIAN_POINT ( 'NONE',  ( -8.826826895187510402, -94.96827758698185562, 5.500000000000000000 ) ) ;
#9670 = CARTESIAN_POINT ( 'NONE',  ( -0.9515373497862389396, -96.47140937769621871, 5.500000000000000000 ) ) ;
#9671 = DIRECTION ( 'NONE',  ( 0.000000000000000000, -0.8090169943749401238, -0.5877852522924831291 ) ) ;
#9672 = ORIENTED_EDGE ( 'NONE', *, *, #19813, .T. ) ;
#9674 = EDGE_CURVE ( 'NONE', #32864, #33539, #24544, .T. ) ;
#9673 = CARTESIAN_POINT ( 'NONE',  ( 0.000000000000000000, 0.000000000000000000, 0.000000000000000000 ) ) ;
#9675 = LINE ( 'NONE', #25084, #25154 ) ;
#9676 = CARTESIAN_POINT ( 'NONE',  ( 0.000000000000000000, 0.000000000000000000, 0.000000000000000000 ) ) ;
#9677 = CARTESIAN_POINT ( 'NONE',  ( -34.02017708624681092, -109.8571428571428470, -2.500000000000000000 ) ) ;
#9678 = CIRCLE ( 'NONE', #37031, 15.99999999999999645 ) ;
#9679 = AXIS2_PLACEMENT_3D ( 'NONE', #23823, #27751, #16723 ) ;
#9680 = CYLINDRICAL_SURFACE ( 'NONE', #42017, 31.99999999999998579 ) ;
#9681 = DIRECTION ( 'NONE',  ( 0.000000000000000000, 0.000000000000000000, 1.000000000000000000 ) ) ;
#9682 = EDGE_LOOP ( 'NONE', ( #33485, #37240, #41586, #39407 ) ) ;
#9683 = CIRCLE ( 'NONE', #37037, 37.49900000000000944 ) ;
#9685 = CIRCLE ( 'NONE', #8882, 77.49899999999999523 ) ;
#9684 = CARTESIAN_POINT ( 'NONE',  ( 12.00000000000000000, -3.948201729842355068, -23.21447184625292692 ) ) ;
#9686 = AXIS2_PLACEMENT_3D ( 'NONE', #11861, #41481, #19424 ) ;
#9687 = ORIENTED_EDGE ( 'NONE', *, *, #7105, .T. ) ;
#9688 = ORIENTED_EDGE ( 'NONE', *, *, #30411, .T. ) ;
#9689 = PRODUCT ( 'taper roller bearing_iso_ISO 355-2 - 2BD25 - 22,SI,NC,22', 'taper roller bearing_iso_ISO 355-2 - 2BD25 - 22,SI,NC,22', '', ( #12537 ) ) ;
#9690 = CARTESIAN_POINT ( 'NONE',  ( 10.00000000000000000, 41.76937507738875155, -62.50329211542393892 ) ) ;
#9691 = ORIENTED_EDGE ( 'NONE', *, *, #8156, .F. ) ;
#9692 = ORIENTED_EDGE ( 'NONE', *, *, #29666, .F. ) ;
#9693 = VECTOR ( 'NONE', #27899, 1000.000000000000000 ) ;
#9694 = CIRCLE ( 'NONE', #16734, 82.00000000000000000 ) ;
#9695 = VECTOR ( 'NONE', #24487, 1000.000000000000114 ) ;
#9696 = AXIS2_PLACEMENT_3D ( 'NONE', #8004, #33475, #31451 ) ;
#9697 = CARTESIAN_POINT ( 'NONE',  ( -10.00000000000000000, 0.000000000000000000, 0.000000000000000000 ) ) ;
#9698 = ORIENTED_EDGE ( 'NONE', *, *, #32214, .F. ) ;
#9699 = CIRCLE ( 'NONE', #5807, 82.00000000000000000 ) ;
#9700 = EDGE_LOOP ( 'NONE', ( #47177, #26755, #34048, #33469 ) ) ;
#9701 = CARTESIAN_POINT ( 'NONE',  ( 11.99999999999999822, -75.11764819372145041, -2.946379043147127064 ) ) ;
#9702 = DIRECTION ( 'NONE',  ( 0.000000000000000000, -0.1564344650402170189, -0.9876883405951399908 ) ) ;
#9703 = EDGE_CURVE ( 'NONE', #28619, #17612, #17546, .T. ) ;
#9704 = ORIENTED_EDGE ( 'NONE', *, *, #14418, .F. ) ;
#9705 = ORIENTED_EDGE ( 'NONE', *, *, #46405, .T. ) ;
#9706 = EDGE_LOOP ( 'NONE', ( #9461, #367, #9336, #34671 ) ) ;
#9707 = DIRECTION ( 'NONE',  ( 1.000000000000000000, -0.000000000000000000, -0.000000000000000000 ) ) ;
#9709 = EDGE_LOOP ( 'NONE', ( #34156, #33064, #14652, #14902 ) ) ;
#9708 = PLANE ( 'NONE',  #8660 ) ;
#9711 = DIRECTION ( 'NONE',  ( 0.000000000000000000, 0.000000000000000000, 1.000000000000000000 ) ) ;
#9710 = AXIS2_PLACEMENT_3D ( 'NONE', #31367, #47003, #35015 ) ;
#9712 = ORIENTED_EDGE ( 'NONE', *, *, #25846, .F. ) ;
#9713 = ORIENTED_EDGE ( 'NONE', *, *, #46259, .F. ) ;
#9714 = DIRECTION ( 'NONE',  ( -1.000000000000000000, -0.000000000000000000, -0.000000000000000000 ) ) ;
#9715 = ORIENTED_EDGE ( 'NONE', *, *, #44734, .F. ) ;
#9716 = DIRECTION ( 'NONE',  ( -1.000000000000000000, 0.000000000000000000, -0.000000000000000000 ) ) ;
#9717 = CARTESIAN_POINT ( 'NONE',  ( 0.000000000000000000, 0.000000000000000000, 0.000000000000000000 ) ) ;
#9718 = VECTOR ( 'NONE', #9382, 1000.000000000000000 ) ;
#9719 = LINE ( 'NONE', #16589, #38528 ) ;
#9720 = CARTESIAN_POINT ( 'NONE',  ( 10.00000000000000000, 23.16143007188426850, 73.95703589263983702 ) ) ;
#9721 = CIRCLE ( 'NONE', #7274, 31.99999999999998934 ) ;
#9722 = ADVANCED_FACE ( 'NONE', ( #37115 ), #3586, .T. ) ;
#9723 = DIRECTION ( 'NONE',  ( 1.000000000000000000, 0.000000000000000000, 0.000000000000000000 ) ) ;
#9724 = EDGE_CURVE ( 'NONE', #6346, #25011, #34693, .T. ) ;
#9725 = EDGE_CURVE ( 'NONE', #7570, #40885, #47181, .T. ) ;
#9726 = CYLINDRICAL_SURFACE ( 'NONE', #29750, 31.99999999999999289 ) ;
#9727 = DIRECTION ( 'NONE',  ( 0.000000000000000000, 0.000000000000000000, 1.000000000000000000 ) ) ;
#9728 = AXIS2_PLACEMENT_3D ( 'NONE', #28309, #36130, #28794 ) ;
#9729 = AXIS2_PLACEMENT_3D ( 'NONE', #47014, #42636, #28658 ) ;
#9730 = EDGE_LOOP ( 'NONE', ( #35885, #32627, #9213, #46242 ) ) ;
#9731 = VECTOR ( 'NONE', #9493, 1000.000000000000000 ) ;
#9733 = ADVANCED_FACE ( 'NONE', ( #9969 ), #24895, .F. ) ;
#9732 = CARTESIAN_POINT ( 'NONE',  ( -3.000000000000000000, 23.50000000000000000, -1.500000000000001332 ) ) ;
#9734 = ORIENTED_EDGE ( 'NONE', *, *, #10339, .T. ) ;
#9735 = VECTOR ( 'NONE', #23072, 1000.000000000000000 ) ;
#9736 = CARTESIAN_POINT ( 'NONE',  ( 11.99999999999999822, 28.89263327155849126, -71.91182617369157981 ) ) ;
#9737 = CARTESIAN_POINT ( 'NONE',  ( 12.50000000000000000, -132.5000000000000000, 2.500000000000000000 ) ) ;
#9738 = DIRECTION ( 'NONE',  ( -1.000000000000000000, -0.000000000000000000, 0.000000000000000000 ) ) ;
#9739 = EDGE_CURVE ( 'NONE', #13040, #21273, #16720, .T. ) ;
#9740 = ORIENTED_EDGE ( 'NONE', *, *, #30395, .T. ) ;
#9741 = DIRECTION ( 'NONE',  ( -1.000000000000000000, 0.000000000000000000, 0.000000000000000000 ) ) ;
#9742 = AXIS2_PLACEMENT_3D ( 'NONE', #15573, #7259, #26831 ) ;
#9743 = ORIENTED_EDGE ( 'NONE', *, *, #18908, .T. ) ;
#9744 = FILL_AREA_STYLE ('',( #39371 ) ) ;
#9745 = DIRECTION ( 'NONE',  ( -1.000000000000000000, 0.000000000000000000, -0.000000000000000000 ) ) ;
#9746 = ORIENTED_EDGE ( 'NONE', *, *, #10263, .T. ) ;
#9747 = CARTESIAN_POINT ( 'NONE',  ( 10.00000000000000000, -36.13751322684434797, 21.40280677340358295 ) ) ;
#9748 = CARTESIAN_POINT ( 'NONE',  ( -7.572224309238338336, -145.4393675041377492, -5.500000000000000000 ) ) ;
#9749 = CARTESIAN_POINT ( 'NONE',  ( 0.000000000000000000, 0.000000000000000000, 0.000000000000000000 ) ) ;
#9750 = EDGE_CURVE ( 'NONE', #13159, #23062, #28811, .T. ) ;
#9751 = CARTESIAN_POINT ( 'NONE',  ( -8.452893869119503023, -12.51233732111638375, 0.000000000000000000 ) ) ;
#9752 =( NAMED_UNIT ( * ) PLANE_ANGLE_UNIT ( ) SI_UNIT ( $, .RADIAN. ) );
#9753 = VERTEX_POINT ( 'NONE', #399 ) ;
#9754 = ORIENTED_EDGE ( 'NONE', *, *, #21373, .T. ) ;
#9755 = ORIENTED_EDGE ( 'NONE', *, *, #36786, .F. ) ;
#9756 = CIRCLE ( 'NONE', #30100, 82.00000000000000000 ) ;
#9757 = CIRCLE ( 'NONE', #23070, 31.99999999999999289 ) ;
#9758 = DIRECTION ( 'NONE',  ( 0.000000000000000000, -0.7604059656000227152, -0.6494480483301934282 ) ) ;
#9759 = LINE ( 'NONE', #5866, #25339 ) ;
#9760 = ORIENTED_EDGE ( 'NONE', *, *, #36543, .F. ) ;
#9761 = EDGE_CURVE ( 'NONE', #27123, #5156, #34634, .T. ) ;
#9762 = VECTOR ( 'NONE', #28254, 1000.000000000000114 ) ;
#9763 = VECTOR ( 'NONE', #11740, 1000.000000000000000 ) ;
#9764 = DIRECTION ( 'NONE',  ( 0.000000000000000000, 0.1564344650402244852, 0.9876883405951387696 ) ) ;
#9765 = EDGE_CURVE ( 'NONE', #12329, #26225, #23726, .T. ) ;
#9766 = VERTEX_POINT ( 'NONE', #638 ) ;
#9767 = EDGE_LOOP ( 'NONE', ( #2315, #46040, #46319, #35115 ) ) ;
#9768 = AXIS2_PLACEMENT_3D ( 'NONE', #41771, #36921, #44287 ) ;
#9769 = VERTEX_POINT ( 'NONE', #34165 ) ;
#9770 = EDGE_CURVE ( 'NONE', #46921, #28791, #11436, .T. ) ;
#9771 = VECTOR ( 'NONE', #21408, 1000.000000000000000 ) ;
#9772 = DIRECTION ( 'NONE',  ( 0.000000000000000000, 0.000000000000000000, -1.000000000000000000 ) ) ;
#9773 = ORIENTED_EDGE ( 'NONE', *, *, #35172, .F. ) ;
#9774 = CARTESIAN_POINT ( 'NONE',  ( 10.00000000000000000, 3.894527615417895383, 81.90746397400390322 ) ) ;
#9775 = EDGE_LOOP ( 'NONE', ( #29990, #10518, #27359, #23437 ) ) ;
#9776 = CARTESIAN_POINT ( 'NONE',  ( 10.00000000000000000, 0.000000000000000000, 0.000000000000000000 ) ) ;
#9777 = AXIS2_PLACEMENT_3D ( 'NONE', #22512, #30573, #33750 ) ;
#9778 = DIRECTION ( 'NONE',  ( 0.000000000000000000, 0.3826834323650904479, -0.9238795325112865164 ) ) ;
#9779 = CARTESIAN_POINT ( 'NONE',  ( 11.99999999999999822, -73.44644590900077219, 24.73286445877677764 ) ) ;
#9780 = ORIENTED_EDGE ( 'NONE', *, *, #22471, .T. ) ;
#9781 = ADVANCED_FACE ( 'NONE', ( #15346 ), #23387, .T. ) ;
#9782 = DIRECTION ( 'NONE',  ( 0.000000000000000000, 0.8526401643540936215, -0.5224985647159469115 ) ) ;
#9783 = EDGE_CURVE ( 'NONE', #42296, #30440, #286, .T. ) ;
#9784 = ORIENTED_EDGE ( 'NONE', *, *, #22828, .F. ) ;
#9785 = CARTESIAN_POINT ( 'NONE',  ( 10.00000000000000000, 27.13269053701096922, 25.88420570971410228 ) ) ;
#9786 = CIRCLE ( 'NONE', #12151, 77.49899999999999523 ) ;
#9787 = DIRECTION ( 'NONE',  ( -0.5200609990132993854, -0.8541291221503275466, 0.000000000000000000 ) ) ;
#9788 = ORIENTED_EDGE ( 'NONE', *, *, #3455, .T. ) ;
#9789 = VERTEX_POINT ( 'NONE', #34389 ) ;
#9790 = FACE_OUTER_BOUND ( 'NONE', #40298, .T. ) ;
#9791 = CIRCLE ( 'NONE', #37150, 77.49899999999999523 ) ;
#9792 = DIRECTION ( 'NONE',  ( -1.000000000000000000, -0.000000000000000000, 0.000000000000000000 ) ) ;
#9793 = VERTEX_POINT ( 'NONE', #864 ) ;
#9794 = DIRECTION ( 'NONE',  ( -1.000000000000000000, -0.000000000000000000, -0.000000000000000000 ) ) ;
#9795 = CARTESIAN_POINT ( 'NONE',  ( 10.00000000000000000, 33.79645857604513992, -16.45098606841138178 ) ) ;
#9796 = FACE_OUTER_BOUND ( 'NONE', #37592, .T. ) ;
#9797 = DIRECTION ( 'NONE',  ( -1.000000000000000000, 0.000000000000000000, 0.000000000000000000 ) ) ;
#9798 = PRODUCT_RELATED_PRODUCT_CATEGORY ( 'part', '', ( #42918 ) ) ;
#9799 = CARTESIAN_POINT ( 'NONE',  ( 0.000000000000000000, -15.33399622253424432, -80.55351364060604169 ) ) ;
#9800 = CIRCLE ( 'NONE', #39516, 32.00000000000000000 ) ;
#9801 = AXIS2_PLACEMENT_3D ( 'NONE', #13771, #28698, #10084 ) ;
#9802 = DIRECTION ( 'NONE',  ( -1.000000000000000000, 0.000000000000000000, -0.000000000000000000 ) ) ;
#9803 = DIRECTION ( 'NONE',  ( 1.000000000000000000, 0.000000000000000000, -0.000000000000000000 ) ) ;
#9804 = VECTOR ( 'NONE', #4026, 1000.000000000000000 ) ;
#9805 = DIRECTION ( 'NONE',  ( -1.000000000000000000, -0.000000000000000000, -0.000000000000000000 ) ) ;
#9806 = CARTESIAN_POINT ( 'NONE',  ( 0.000000000000000000, 0.000000000000000000, 0.000000000000000000 ) ) ;
#9807 = DIRECTION ( 'NONE',  ( 0.000000000000000000, 0.9876883405951371042, 0.1564344650402347547 ) ) ;
#9808 = FACE_OUTER_BOUND ( 'NONE', #40547, .T. ) ;
#9809 = AXIS2_PLACEMENT_3D ( 'NONE', #27551, #30999, #8459 ) ;
#9810 = DIRECTION ( 'NONE',  ( 1.000000000000000000, 0.000000000000000000, 0.000000000000000000 ) ) ;
#9811 = VECTOR ( 'NONE', #16177, 1000.000000000000114 ) ;
#9812 = EDGE_LOOP ( 'NONE', ( #44789, #21934 ) ) ;
#9813 = ORIENTED_EDGE ( 'NONE', *, *, #40077, .T. ) ;
#9814 = ORIENTED_EDGE ( 'NONE', *, *, #26306, .F. ) ;
#9815 = DIRECTION ( 'NONE',  ( -1.000000000000000000, -0.000000000000000000, -0.000000000000000000 ) ) ;
#9816 = CARTESIAN_POINT ( 'NONE',  ( 15.00000000000000000, -4.261787119644963262, 26.19803753235780164 ) ) ;
#9817 = VECTOR ( 'NONE', #942, 1000.000000000000000 ) ;
#9818 = DIRECTION ( 'NONE',  ( 0.000000000000000000, 0.000000000000000000, 1.000000000000000000 ) ) ;
#9819 = ORIENTED_EDGE ( 'NONE', *, *, #40840, .T. ) ;
#9820 = AXIS2_PLACEMENT_3D ( 'NONE', #16428, #17372, #46782 ) ;
#9821 = EDGE_CURVE ( 'NONE', #15030, #28496, #34661, .T. ) ;
#9822 = CARTESIAN_POINT ( 'NONE',  ( 10.00000000000000000, -33.00180498840035170, -17.80606268964575278 ) ) ;
#9823 = ORIENTED_EDGE ( 'NONE', *, *, #4868, .T. ) ;
#9824 = CARTESIAN_POINT ( 'NONE',  ( 0.000000000000000000, 0.000000000000000000, 0.000000000000000000 ) ) ;
#9825 = EDGE_CURVE ( 'NONE', #18873, #31959, #45636, .T. ) ;
#9826 = VERTEX_POINT ( 'NONE', #12160 ) ;
#9827 = CARTESIAN_POINT ( 'NONE',  ( 10.00000000000000000, -71.87247863392443037, 39.47590169984818687 ) ) ;
#9828 = EDGE_CURVE ( 'NONE', #24169, #45521, #13565, .T. ) ;
#9829 = AXIS2_PLACEMENT_3D ( 'NONE', #32756, #43319, #6586 ) ;
#9830 = DIRECTION ( 'NONE',  ( -1.000000000000000000, 0.000000000000000000, 0.000000000000000000 ) ) ;
#9831 = DIRECTION ( 'NONE',  ( -1.000000000000000000, 0.000000000000000000, 0.000000000000000000 ) ) ;
#9832 = ORIENTED_EDGE ( 'NONE', *, *, #19323, .F. ) ;
#9833 = CARTESIAN_POINT ( 'NONE',  ( 10.00000000000000000, -20.40083707022829174, -72.35432306680507963 ) ) ;
#9834 = VERTEX_POINT ( 'NONE', #41285 ) ;
#9835 = CIRCLE ( 'NONE', #24695, 31.99999999999999645 ) ;
#9836 = EDGE_LOOP ( 'NONE', ( #16168, #42856, #21238, #44365 ) ) ;
#9837 = CARTESIAN_POINT ( 'NONE',  ( 0.000000000000000000, -120.0000000000000000, 2.500000000000000000 ) ) ;
#9838 = AXIS2_PLACEMENT_3D ( 'NONE', #7447, #33616, #3036 ) ;
#9839 = EDGE_CURVE ( 'NONE', #8908, #16167, #40166, .T. ) ;
#9840 = CARTESIAN_POINT ( 'NONE',  ( 0.7195005275814480017, -121.3161758966073052, 2.500000000000000000 ) ) ;
#9841 = DIRECTION ( 'NONE',  ( 1.000000000000000000, -0.000000000000000000, 0.000000000000000000 ) ) ;
#9842 = EDGE_CURVE ( 'NONE', #842, #45536, #19040, .T. ) ;
#9843 = PLANE ( 'NONE',  #786 ) ;
#9844 = DIRECTION ( 'NONE',  ( 0.000000000000000000, -0.6494480483301741103, -0.7604059656000390355 ) ) ;
#9845 = EDGE_LOOP ( 'NONE', ( #46506, #35479, #28863, #45596 ) ) ;
#9846 = VECTOR ( 'NONE', #44427, 1000.000000000000000 ) ;
#9847 = DIRECTION ( 'NONE',  ( -1.000000000000000000, -0.000000000000000000, -0.000000000000000000 ) ) ;
#9848 = ORIENTED_EDGE ( 'NONE', *, *, #15593, .F. ) ;
#9849 = ORIENTED_EDGE ( 'NONE', *, *, #39282, .F. ) ;
#9850 = EDGE_CURVE ( 'NONE', #43802, #45904, #4327, .T. ) ;
#9851 = LINE ( 'NONE', #36275, #42665 ) ;
#9852 = DIRECTION ( 'NONE',  ( -1.000000000000000000, -0.000000000000000000, 0.000000000000000000 ) ) ;
#9853 = AXIS2_PLACEMENT_3D ( 'NONE', #23641, #34178, #4806 ) ;
#9854 = DIRECTION ( 'NONE',  ( -1.000000000000000000, 0.000000000000000000, 0.000000000000000000 ) ) ;
#9855 = DIRECTION ( 'NONE',  ( 0.000000000000000000, 0.000000000000000000, 1.000000000000000000 ) ) ;
#9856 = VERTEX_POINT ( 'NONE', #29768 ) ;
#9857 = CARTESIAN_POINT ( 'NONE',  ( 10.00000000000000000, 59.46389618802034960, -49.70050353004825894 ) ) ;
#9858 = VECTOR ( 'NONE', #7697, 1000.000000000000000 ) ;
#9859 = DIRECTION ( 'NONE',  ( 1.000000000000000000, -0.000000000000000000, -0.000000000000000000 ) ) ;
#9860 = DIRECTION ( 'NONE',  ( 0.000000000000000000, 0.2079116908177545131, -0.9781476007338066880 ) ) ;
#9861 = CARTESIAN_POINT ( 'NONE',  ( 10.00000000000000000, 8.830959090342393125, 74.65491531819122883 ) ) ;
#9862 = ADVANCED_FACE ( 'NONE', ( #44700 ), #7969, .F. ) ;
#9863 = CIRCLE ( 'NONE', #32532, 82.00000000000000000 ) ;
#9864 = DIRECTION ( 'NONE',  ( -1.000000000000000000, -0.000000000000000000, 0.000000000000000000 ) ) ;
#9865 = ORIENTED_EDGE ( 'NONE', *, *, #35820, .F. ) ;
#9866 = CARTESIAN_POINT ( 'NONE',  ( 0.000000000000000000, 12.93880638057426502, -76.41127070299258150 ) ) ;
#9867 = DIRECTION ( 'NONE',  ( -1.000000000000000000, 0.000000000000000000, 0.000000000000000000 ) ) ;
#9868 = LINE ( 'NONE', #7154, #46687 ) ;
#9869 = CARTESIAN_POINT ( 'NONE',  ( 10.00000000000000000, -24.73286445877653961, -73.44644590900085745 ) ) ;
#9870 = CYLINDRICAL_SURFACE ( 'NONE', #46308, 31.99999999999998579 ) ;
#9871 = DIRECTION ( 'NONE',  ( 0.000000000000000000, -0.8526401643540970632, 0.5224985647159409163 ) ) ;
#9872 = STYLED_ITEM ( 'NONE', ( #6027 ), #2442 ) ;
#9873 = VERTEX_POINT ( 'NONE', #26101 ) ;
#9874 = ORIENTED_EDGE ( 'NONE', *, *, #37986, .T. ) ;
#9875 = AXIS2_PLACEMENT_3D ( 'NONE', #13157, #6297, #46451 ) ;
#9876 = DIRECTION ( 'NONE',  ( -1.000000000000000000, -0.000000000000000000, -0.000000000000000000 ) ) ;
#9877 = ORIENTED_EDGE ( 'NONE', *, *, #24528, .T. ) ;
#9878 = CARTESIAN_POINT ( 'NONE',  ( 13.36581099891334645, -139.3288669181958710, -2.500000000000000000 ) ) ;
#9879 = AXIS2_PLACEMENT_3D ( 'NONE', #43579, #21050, #5655 ) ;
#9880 = LINE ( 'NONE', #46358, #18979 ) ;
#9881 = ORIENTED_EDGE ( 'NONE', *, *, #4390, .T. ) ;
#9882 = CIRCLE ( 'NONE', #38731, 82.00000000000000000 ) ;
#9883 = DIRECTION ( 'NONE',  ( -1.000000000000000000, -0.000000000000000000, 0.000000000000000000 ) ) ;
#9884 = EDGE_CURVE ( 'NONE', #8515, #10011, #7740, .T. ) ;
#9885 = VECTOR ( 'NONE', #15953, 1000.000000000000000 ) ;
#9886 = VERTEX_POINT ( 'NONE', #33916 ) ;
#9887 = ORIENTED_EDGE ( 'NONE', *, *, #41040, .T. ) ;
#9888 = CIRCLE ( 'NONE', #36439, 13.90444123027096879 ) ;
#9889 = EDGE_CURVE ( 'NONE', #26989, #1613, #7511, .T. ) ;
#9890 = ORIENTED_EDGE ( 'NONE', *, *, #1740, .F. ) ;
#9891 = EDGE_CURVE ( 'NONE', #3320, #33272, #28454, .T. ) ;
#9892 = AXIS2_PLACEMENT_3D ( 'NONE', #165, #15833, #7532 ) ;
#9893 = EDGE_CURVE ( 'NONE', #26166, #11716, #18743, .T. ) ;
#9894 = CARTESIAN_POINT ( 'NONE',  ( 0.000000000000000000, 0.000000000000000000, 0.000000000000000000 ) ) ;
#9895 = EDGE_CURVE ( 'NONE', #36949, #45729, #19800, .T. ) ;
#9896 = DIRECTION ( 'NONE',  ( 0.000000000000000000, 0.000000000000000000, 1.000000000000000000 ) ) ;
#9897 = CARTESIAN_POINT ( 'NONE',  ( -3.000000000000000000, -0.9646360437372163421, -23.52805723605591126 ) ) ;
#9898 = ORIENTED_EDGE ( 'NONE', *, *, #6568, .T. ) ;
#9899 = DIRECTION ( 'NONE',  ( -1.000000000000000000, 0.000000000000000000, -0.000000000000000000 ) ) ;
#9900 = VERTEX_POINT ( 'NONE', #5767 ) ;
#9901 = VERTEX_POINT ( 'NONE', #20201 ) ;
#9902 = VERTEX_POINT ( 'NONE', #42482 ) ;
#9903 = CARTESIAN_POINT ( 'NONE',  ( 0.000000000000000000, 0.000000000000000000, 0.000000000000000000 ) ) ;
#9904 = LINE ( 'NONE', #44159, #44241 ) ;
#9905 = EDGE_CURVE ( 'NONE', #46331, #8930, #31003, .T. ) ;
#9906 = CARTESIAN_POINT ( 'NONE',  ( 11.99999999999999822, 46.54456581323888997, -59.03342792756214408 ) ) ;
#9907 = AXIS2_PLACEMENT_3D ( 'NONE', #30491, #16056, #18976 ) ;
#9908 = EDGE_LOOP ( 'NONE', ( #263, #23972, #17455, #46178 ) ) ;
#9909 = DIRECTION ( 'NONE',  ( -1.000000000000000000, 0.000000000000000000, 0.000000000000000000 ) ) ;
#9910 = VERTEX_POINT ( 'NONE', #16783 ) ;
#9911 = ADVANCED_FACE ( 'NONE', ( #8945 ), #19956, .F. ) ;
#9912 = DIRECTION ( 'NONE',  ( -1.000000000000000000, 0.000000000000000000, -0.000000000000000000 ) ) ;
#9913 = VECTOR ( 'NONE', #35982, 1000.000000000000000 ) ;
#9914 = DIRECTION ( 'NONE',  ( -1.000000000000000000, 0.000000000000000000, 0.000000000000000000 ) ) ;
#9915 = CARTESIAN_POINT ( 'NONE',  ( 10.00000000000000000, 71.87247863392413194, 39.47590169984869135 ) ) ;
#9916 = DIRECTION ( 'NONE',  ( -1.000000000000000000, -0.000000000000000000, 0.000000000000000000 ) ) ;
#9917 = PLANE ( 'NONE',  #39361 ) ;
#9918 = DIRECTION ( 'NONE',  ( -1.000000000000000000, 0.000000000000000000, -0.000000000000000000 ) ) ;
#9919 = DIRECTION ( 'NONE',  ( -1.000000000000000000, 0.000000000000000000, -0.000000000000000000 ) ) ;
#9920 = DIRECTION ( 'NONE',  ( 5.778480238264233142E-17, -1.000000000000000000, 0.000000000000000000 ) ) ;
#9921 = CARTESIAN_POINT ( 'NONE',  ( 0.000000000000000000, -71.91182617369166508, -28.89263327155821770 ) ) ;
#9922 = EDGE_CURVE ( 'NONE', #12455, #39152, #46421, .T. ) ;
#9923 = LINE ( 'NONE', #47376, #37975 ) ;
#9924 = ORIENTED_EDGE ( 'NONE', *, *, #31299, .T. ) ;
#9925 = AXIS2_PLACEMENT_3D ( 'NONE', #13304, #20157, #16737 ) ;
#9926 = VERTEX_POINT ( 'NONE', #35369 ) ;
#9927 = DIRECTION ( 'NONE',  ( -1.000000000000000000, 0.000000000000000000, 0.000000000000000000 ) ) ;
#9928 = CARTESIAN_POINT ( 'NONE',  ( 0.000000000000000000, 27.75498641678786527, -31.52238457039571173 ) ) ;
#9929 = DIRECTION ( 'NONE',  ( -1.000000000000000000, 0.000000000000000000, 0.000000000000000000 ) ) ;
#9930 = AXIS2_PLACEMENT_3D ( 'NONE', #30037, #46172, #5781 ) ;
#9931 = CARTESIAN_POINT ( 'NONE',  ( -30.50000000000000000, -120.0000000000000000, 2.500000000000000000 ) ) ;
#9932 = CIRCLE ( 'NONE', #4483, 77.49899999999998101 ) ;
#9933 = EDGE_CURVE ( 'NONE', #7367, #42453, #31965, .T. ) ;
#9934 = DIRECTION ( 'NONE',  ( 0.000000000000000000, 0.3090169943749480619, -0.9510565162951533091 ) ) ;
#9935 = LINE ( 'NONE', #13602, #37040 ) ;
#9936 = ORIENTED_EDGE ( 'NONE', *, *, #36284, .T. ) ;
#9937 = LINE ( 'NONE', #24859, #19129 ) ;
#9938 = ORIENTED_EDGE ( 'NONE', *, *, #12131, .T. ) ;
#9939 = CARTESIAN_POINT ( 'NONE',  ( -10.90076147243505211, 0.000000000000000000, 0.000000000000000000 ) ) ;
#9940 = ORIENTED_EDGE ( 'NONE', *, *, #41952, .F. ) ;
#9941 = AXIS2_PLACEMENT_3D ( 'NONE', #34345, #23111, #41474 ) ;
#9942 = ORIENTED_EDGE ( 'NONE', *, *, #5124, .F. ) ;
#9943 = AXIS2_PLACEMENT_3D ( 'NONE', #27254, #37775, #8161 ) ;
#9944 = EDGE_LOOP ( 'NONE', ( #23082, #8649, #40611, #17050 ) ) ;
#9945 = EDGE_CURVE ( 'NONE', #28565, #8938, #10462, .T. ) ;
#9946 = CIRCLE ( 'NONE', #1327, 31.99999999999998579 ) ;
#9947 = DIRECTION ( 'NONE',  ( 0.000000000000000000, -0.9510565162951499785, -0.3090169943749582204 ) ) ;
#9948 = ORIENTED_EDGE ( 'NONE', *, *, #21905, .T. ) ;
#9949 = ADVANCED_FACE ( 'NONE', ( #35622 ), #42971, .F. ) ;
#9950 = VERTEX_POINT ( 'NONE', #38574 ) ;
#9951 = AXIS2_PLACEMENT_3D ( 'NONE', #26977, #7871, #19366 ) ;
#9952 = ADVANCED_FACE ( 'NONE', ( #28267 ), #39052, .T. ) ;
#9953 = CARTESIAN_POINT ( 'NONE',  ( 11.99999999999999822, -31.47745569255189224, 68.26794271651249346 ) ) ;
#9954 = DIRECTION ( 'NONE',  ( -1.000000000000000000, 0.000000000000000000, 0.000000000000000000 ) ) ;
#9955 = ORIENTED_EDGE ( 'NONE', *, *, #22162, .F. ) ;
#9956 = ORIENTED_EDGE ( 'NONE', *, *, #21080, .T. ) ;
#9957 = EDGE_LOOP ( 'NONE', ( #42113, #25397, #30331, #35293 ) ) ;
#9958 = DIRECTION ( 'NONE',  ( 0.8541291221503265474, -0.5200609990133007177, 0.000000000000000000 ) ) ;
#9959 = LINE ( 'NONE', #24882, #22712 ) ;
#9960 = AXIS2_PLACEMENT_3D ( 'NONE', #32097, #34595, #2455 ) ;
#9961 = FACE_OUTER_BOUND ( 'NONE', #41153, .T. ) ;
#9962 = ORIENTED_EDGE ( 'NONE', *, *, #15724, .T. ) ;
#9963 = ORIENTED_EDGE ( 'NONE', *, *, #19467, .F. ) ;
#9964 = CYLINDRICAL_SURFACE ( 'NONE', #24726, 31.99999999999998579 ) ;
#9965 = ORIENTED_EDGE ( 'NONE', *, *, #31884, .T. ) ;
#9966 = CARTESIAN_POINT ( 'NONE',  ( 11.99999999999999822, 73.73191006444551476, 14.66109333815590254 ) ) ;
#9967 = CARTESIAN_POINT ( 'NONE',  ( 10.00000000000000000, 37.22597642581158084, -5.202137450156524068 ) ) ;
#9968 = DIRECTION ( 'NONE',  ( -1.000000000000000000, 0.000000000000000000, 0.000000000000000000 ) ) ;
#9969 = FACE_OUTER_BOUND ( 'NONE', #10053, .T. ) ;
#9970 = DIRECTION ( 'NONE',  ( -0.000000000000000000, -0.6691306063588671194, 0.7431448254773862505 ) ) ;
#9971 = LINE ( 'NONE', #3096, #16490 ) ;
#9972 = CARTESIAN_POINT ( 'NONE',  ( 10.00000000000000000, 75.11764819372149304, 29.05362095685338986 ) ) ;
#9973 = ORIENTED_EDGE ( 'NONE', *, *, #16917, .T. ) ;
#9974 = CARTESIAN_POINT ( 'NONE',  ( 10.00000000000000000, 0.000000000000000000, 0.000000000000000000 ) ) ;
#9975 = ORIENTED_EDGE ( 'NONE', *, *, #5264, .T. ) ;
#9976 = CARTESIAN_POINT ( 'NONE',  ( 0.000000000000000000, 0.000000000000000000, 0.000000000000000000 ) ) ;
#9977 = CARTESIAN_POINT ( 'NONE',  ( 0.000000000000000000, -58.39081064771786345, 50.95692526931308919 ) ) ;
#9978 = LINE ( 'NONE', #35695, #20666 ) ;
#9979 = DIRECTION ( 'NONE',  ( 0.000000000000000000, 0.8090169943749487835, -0.5877852522924713607 ) ) ;
#9980 = CARTESIAN_POINT ( 'NONE',  ( 10.00000000000000000, 12.93880638057426502, -76.41127070299258150 ) ) ;
#9981 = DIRECTION ( 'NONE',  ( -1.000000000000000000, -0.000000000000000000, -0.000000000000000000 ) ) ;
#9982 = ORIENTED_EDGE ( 'NONE', *, *, #31782, .T. ) ;
#9983 = CIRCLE ( 'NONE', #43598, 31.99999999999998579 ) ;
#9984 = CARTESIAN_POINT ( 'NONE',  ( 10.00000000000000000, -0.8828120875898013420, -37.48860685352291711 ) ) ;
#9985 = DIRECTION ( 'NONE',  ( -1.000000000000000000, 0.000000000000000000, 0.000000000000000000 ) ) ;
#9986 = CYLINDRICAL_SURFACE ( 'NONE', #14513, 82.00000000000000000 ) ;
#9987 = CARTESIAN_POINT ( 'NONE',  ( -10.94538922500103162, 0.000000000000000000, 0.000000000000000000 ) ) ;
#9988 =( NAMED_UNIT ( * ) PLANE_ANGLE_UNIT ( ) SI_UNIT ( $, .RADIAN. ) );
#9989 = VERTEX_POINT ( 'NONE', #24351 ) ;
#9990 = EDGE_LOOP ( 'NONE', ( #35724, #32446, #35226, #18754 ) ) ;
#9991 = ORIENTED_EDGE ( 'NONE', *, *, #14084, .T. ) ;
#9992 = ORIENTED_EDGE ( 'NONE', *, *, #12922, .T. ) ;
#9993 = VECTOR ( 'NONE', #4325, 1000.000000000000000 ) ;
#9994 = EDGE_CURVE ( 'NONE', #4312, #25302, #5791, .T. ) ;
#9995 = EDGE_CURVE ( 'NONE', #2795, #12057, #46647, .T. ) ;
#9996 = ORIENTED_EDGE ( 'NONE', *, *, #489, .F. ) ;
#9997 = CARTESIAN_POINT ( 'NONE',  ( 12.00000000000000000, -10.45096189432344502, -21.10159698893425784 ) ) ;
#9998 = EDGE_CURVE ( 'NONE', #29279, #17516, #11269, .T. ) ;
#9999 = CARTESIAN_POINT ( 'NONE',  ( 10.00000000000000000, 63.18004540533029001, 44.88180994100400767 ) ) ;
#10000 = ORIENTED_EDGE ( 'NONE', *, *, #7642, .F. ) ;
#10001 = AXIS2_PLACEMENT_3D ( 'NONE', #27678, #4909, #20811 ) ;
#10002 = ADVANCED_FACE ( 'NONE', ( #17010 ), #42734, .T. ) ;
#10003 = DIRECTION ( 'NONE',  ( -1.000000000000000000, 0.000000000000000000, 0.000000000000000000 ) ) ;
#10004 = EDGE_LOOP ( 'NONE', ( #46594, #28977, #24822, #25352 ) ) ;
#10005 = CIRCLE ( 'NONE', #6871, 32.00000000000000000 ) ;
#10006 = ORIENTED_EDGE ( 'NONE', *, *, #8963, .T. ) ;
#10007 = ORIENTED_EDGE ( 'NONE', *, *, #1827, .T. ) ;
#10008 = EDGE_CURVE ( 'NONE', #27618, #26885, #46159, .T. ) ;
#10009 = VERTEX_POINT ( 'NONE', #28043 ) ;
#10010 = VECTOR ( 'NONE', #26091, 1000.000000000000000 ) ;
#10011 = VERTEX_POINT ( 'NONE', #16062 ) ;
#10012 = LINE ( 'NONE', #14412, #6343 ) ;
#10013 = ORIENTED_EDGE ( 'NONE', *, *, #9010, .F. ) ;
#10014 = CARTESIAN_POINT ( 'NONE',  ( 11.99999999999999822, 65.59268652807210742, 36.72794159290264560 ) ) ;
#10015 = VERTEX_POINT ( 'NONE', #9419 ) ;
#10016 = LINE ( 'NONE', #44025, #47058 ) ;
#10017 = EDGE_CURVE ( 'NONE', #5548, #38854, #17510, .T. ) ;
#10018 = CARTESIAN_POINT ( 'NONE',  ( 10.00000000000000000, 37.01155633439059756, 6.555932627142549762 ) ) ;
#10019 = AXIS2_PLACEMENT_3D ( 'NONE', #39313, #38601, #28955 ) ;
#10020 = DIRECTION ( 'NONE',  ( 1.000000000000000000, -0.000000000000000000, -0.000000000000000000 ) ) ;
#10021 = EDGE_LOOP ( 'NONE', ( #15617, #1885, #38367, #27965 ) ) ;
#10022 = CYLINDRICAL_SURFACE ( 'NONE', #47756, 32.00000000000000000 ) ;
#10023 = VERTEX_POINT ( 'NONE', #1608 ) ;
#10024 = AXIS2_PLACEMENT_3D ( 'NONE', #15712, #30644, #45558 ) ;
#10025 = PLANE ( 'NONE',  #45398 ) ;
#10026 = CARTESIAN_POINT ( 'NONE',  ( 10.00000000000000000, 0.000000000000000000, 0.000000000000000000 ) ) ;
#10027 = EDGE_LOOP ( 'NONE', ( #34751, #5204, #31875, #26669 ) ) ;
#10028 = ORIENTED_EDGE ( 'NONE', *, *, #40899, .T. ) ;
#10029 = LINE ( 'NONE', #43571, #33049 ) ;
#10030 = LINE ( 'NONE', #1732, #19896 ) ;
#10031 = ORIENTED_EDGE ( 'NONE', *, *, #18712, .F. ) ;
#10032 = ORIENTED_EDGE ( 'NONE', *, *, #43883, .T. ) ;
#10033 = DIRECTION ( 'NONE',  ( 0.7533909544171996098, 0.6575728627325955200, -7.625282249115660656E-32 ) ) ;
#10034 = CYLINDRICAL_SURFACE ( 'NONE', #9452, 31.99999999999998579 ) ;
#10035 = FACE_OUTER_BOUND ( 'NONE', #47924, .T. ) ;
#10036 = CARTESIAN_POINT ( 'NONE',  ( 10.00000000000000000, -31.47745569255092235, -68.26794271651296242 ) ) ;
#10037 = FACE_OUTER_BOUND ( 'NONE', #9957, .T. ) ;
#10038 = EDGE_CURVE ( 'NONE', #12094, #15804, #47214, .T. ) ;
#10039 = CARTESIAN_POINT ( 'NONE',  ( 0.000000000000000000, -22.32062822937469804, -14.36278369418829826 ) ) ;
#10040 = DIRECTION ( 'NONE',  ( 0.000000000000000000, 0.2334453638559058908, -0.9723699203976764460 ) ) ;
#10041 = EDGE_CURVE ( 'NONE', #39882, #10420, #2350, .T. ) ;
#10042 = AXIS2_PLACEMENT_3D ( 'NONE', #5420, #20330, #46545 ) ;
#10043 = LINE ( 'NONE', #43812, #45560 ) ;
#10044 = CIRCLE ( 'NONE', #2248, 77.49900000000000944 ) ;
#10045 = CYLINDRICAL_SURFACE ( 'NONE', #17553, 16.00000000000000000 ) ;
#10046 = CARTESIAN_POINT ( 'NONE',  ( 0.000000000000000000, 0.000000000000000000, 0.000000000000000000 ) ) ;
#10048 = AXIS2_PLACEMENT_3D ( 'NONE', #31223, #31956, #23615 ) ;
#10047 = CYLINDRICAL_SURFACE ( 'NONE', #31995, 42.00000000000000000 ) ;
#10049 = EDGE_CURVE ( 'NONE', #690, #17289, #13410, .T. ) ;
#10050 = DIRECTION ( 'NONE',  ( 0.000000000000000000, 0.000000000000000000, -1.000000000000000000 ) ) ;
#10051 = ORIENTED_EDGE ( 'NONE', *, *, #23546, .F. ) ;
#10052 = ORIENTED_EDGE ( 'NONE', *, *, #9339, .T. ) ;
#10053 = EDGE_LOOP ( 'NONE', ( #14398, #25603, #17903, #28488 ) ) ;
#10054 = LINE ( 'NONE', #47720, #41684 ) ;
#10055 = VERTEX_POINT ( 'NONE', #21881 ) ;
#10056 = ORIENTED_EDGE ( 'NONE', *, *, #37699, .T. ) ;
#10057 = ADVANCED_FACE ( 'NONE', ( #36572 ), #25553, .T. ) ;
#10058 = DIRECTION ( 'NONE',  ( 0.000000000000000000, 0.000000000000000000, 1.000000000000000000 ) ) ;
#10059 = VERTEX_POINT ( 'NONE', #17239 ) ;
#10060 = EDGE_CURVE ( 'NONE', #26557, #15072, #47583, .T. ) ;
#10061 = EDGE_CURVE ( 'NONE', #26795, #41290, #44672, .T. ) ;
#10062 =( GEOMETRIC_REPRESENTATION_CONTEXT ( 3 ) GLOBAL_UNCERTAINTY_ASSIGNED_CONTEXT ( ( #10542 ) ) GLOBAL_UNIT_ASSIGNED_CONTEXT ( ( #22993, #26916, #42085 ) ) REPRESENTATION_CONTEXT ( 'NONE', 'WORKASPACE' ) );
#10063 = ORIENTED_EDGE ( 'NONE', *, *, #7305, .T. ) ;
#10064 = CARTESIAN_POINT ( 'NONE',  ( 16.30584220631899228, -140.9432449716519784, -2.500000000000000000 ) ) ;
#10065 = ORIENTED_EDGE ( 'NONE', *, *, #3252, .F. ) ;
#10066 = DIRECTION ( 'NONE',  ( -1.000000000000000000, -0.000000000000000000, 0.000000000000000000 ) ) ;
#10067 = ORIENTED_EDGE ( 'NONE', *, *, #14432, .T. ) ;
#10068 = CYLINDRICAL_SURFACE ( 'NONE', #22723, 31.99999999999999289 ) ;
#10069 = PRODUCT_DEFINITION ( 'UNKNOWN', '', #14715, #26193 ) ;
#10070 = VERTEX_POINT ( 'NONE', #36809 ) ;
#10071 = CARTESIAN_POINT ( 'NONE',  ( 0.000000000000000000, -75.11725578898470701, 2.956366410620372864 ) ) ;
#10072 = DIRECTION ( 'NONE',  ( 1.000000000000000000, -0.000000000000000000, 0.000000000000000000 ) ) ;
#10073 = ORIENTED_EDGE ( 'NONE', *, *, #43051, .T. ) ;
#10074 = DIRECTION ( 'NONE',  ( -1.000000000000000000, 0.000000000000000000, 0.000000000000000000 ) ) ;
#10075 = ORIENTED_EDGE ( 'NONE', *, *, #47559, .T. ) ;
#10076 = AXIS2_PLACEMENT_3D ( 'NONE', #13642, #29044, #36624 ) ;
#10077 = ORIENTED_EDGE ( 'NONE', *, *, #29253, .T. ) ;
#10078 = AXIS2_PLACEMENT_3D ( 'NONE', #24831, #24598, #17948 ) ;
#10079 = CARTESIAN_POINT ( 'NONE',  ( -235.0000123116479926, -123.0000000000000284, 2.500000000000000000 ) ) ;
#10080 = CARTESIAN_POINT ( 'NONE',  ( -3.000000000000000000, 23.59884966291538078, -12.14883922797231541 ) ) ;
#10081 = CARTESIAN_POINT ( 'NONE',  ( 0.000000000000000000, -54.21277698773636899, -55.38113227695839669 ) ) ;
#10083 = EDGE_LOOP ( 'NONE', ( #48110, #12964, #29712, #17525 ) ) ;
#10082 = DIRECTION ( 'NONE',  ( 0.000000000000000000, 0.000000000000000000, -1.000000000000000000 ) ) ;
#10084 = DIRECTION ( 'NONE',  ( 0.000000000000000000, -0.7071067811865536790, 0.7071067811865414665 ) ) ;
#10085 = ORIENTED_EDGE ( 'NONE', *, *, #42785, .T. ) ;
#10086 = CARTESIAN_POINT ( 'NONE',  ( 5.000000000000002665, -76.69515212746036070, 29.01471420065537643 ) ) ;
#10087 = ORIENTED_EDGE ( 'NONE', *, *, #32887, .T. ) ;
#10088 = VERTEX_POINT ( 'NONE', #9915 ) ;
#10089 = DIRECTION ( 'NONE',  ( -1.000000000000000000, 0.000000000000000000, -0.000000000000000000 ) ) ;
#10090 = CARTESIAN_POINT ( 'NONE',  ( 10.00000000000000000, 37.58145647212453611, 0.6853352020791767529 ) ) ;
#10091 = VERTEX_POINT ( 'NONE', #17961 ) ;
#10092 = DIRECTION ( 'NONE',  ( 1.000000000000000000, 0.000000000000000000, 0.000000000000000000 ) ) ;
#10093 = CARTESIAN_POINT ( 'NONE',  ( 10.00000000000000000, -38.55633173626998911, -16.65560815589452304 ) ) ;
#10094 = DIRECTION ( 'NONE',  ( 0.000000000000000000, -0.3090169943749563330, 0.9510565162951507556 ) ) ;
#10095 = ORIENTED_EDGE ( 'NONE', *, *, #41708, .F. ) ;
#10096 = CARTESIAN_POINT ( 'NONE',  ( 21.85433023846372436, -135.0628101570779620, 2.500000000000000000 ) ) ;
#10097 = PRODUCT_DEFINITION_SHAPE ( 'NONE', 'NONE',  #33713 ) ;
#10098 = CARTESIAN_POINT ( 'NONE',  ( 10.00000000000000000, 0.000000000000000000, 0.000000000000000000 ) ) ;
#10099 = CARTESIAN_POINT ( 'NONE',  ( 11.99999999999999822, 74.18225833017937987, -34.94270380257559339 ) ) ;
#10100 =( GEOMETRIC_REPRESENTATION_CONTEXT ( 3 ) GLOBAL_UNCERTAINTY_ASSIGNED_CONTEXT ( ( #11989 ) ) GLOBAL_UNIT_ASSIGNED_CONTEXT ( ( #4101, #15371, #27109 ) ) REPRESENTATION_CONTEXT ( 'NONE', 'WORKASPACE' ) );
#10101 = CARTESIAN_POINT ( 'NONE',  ( -7.469491406282116941, 4.756046723998916370, -55.00000000000000000 ) ) ;
#10102 = VERTEX_POINT ( 'NONE', #43920 ) ;
#10103 = EDGE_CURVE ( 'NONE', #1846, #40367, #29817, .T. ) ;
#10104 = DIRECTION ( 'NONE',  ( -1.000000000000000000, 0.000000000000000000, 0.000000000000000000 ) ) ;
#10105 = CARTESIAN_POINT ( 'NONE',  ( 19.12409105625796357, -101.5943176906707919, -2.500000000000000000 ) ) ;
#10106 = FACE_OUTER_BOUND ( 'NONE', #17070, .T. ) ;
#10107 = DIRECTION ( 'NONE',  ( 0.000000000000000000, -0.3826834323650772363, -0.9238795325112919565 ) ) ;
#10108 = ADVANCED_FACE ( 'NONE', ( #14305 ), #25788, .T. ) ;
#10109 = DIRECTION ( 'NONE',  ( 0.000000000000000000, 0.000000000000000000, -1.000000000000000000 ) ) ;
#10110 = DIRECTION ( 'NONE',  ( 0.000000000000000000, 0.000000000000000000, 1.000000000000000000 ) ) ;
#10111 = EDGE_CURVE ( 'NONE', #1904, #41511, #19640, .T. ) ;
#10112 = ORIENTED_EDGE ( 'NONE', *, *, #7946, .F. ) ;
#10113 = ORIENTED_EDGE ( 'NONE', *, *, #31970, .T. ) ;
#10114 = VECTOR ( 'NONE', #41183, 1000.000000000000000 ) ;
#10115 = LINE ( 'NONE', #33109, #13643 ) ;
#10116 = AXIS2_PLACEMENT_3D ( 'NONE', #7951, #34148, #619 ) ;
#10117 = VERTEX_POINT ( 'NONE', #32195 ) ;
#10118 = FACE_OUTER_BOUND ( 'NONE', #46979, .T. ) ;
#10119 = CIRCLE ( 'NONE', #27316, 31.99999999999998579 ) ;
#10120 = LINE ( 'NONE', #1816, #11984 ) ;
#10121 = ORIENTED_EDGE ( 'NONE', *, *, #23197, .T. ) ;
#10122 = EDGE_CURVE ( 'NONE', #36840, #12477, #40732, .T. ) ;
#10123 = EDGE_CURVE ( 'NONE', #38585, #33302, #7839, .T. ) ;
#10124 = AXIS2_PLACEMENT_3D ( 'NONE', #27606, #42542, #23941 ) ;
#10125 = ORIENTED_EDGE ( 'NONE', *, *, #47448, .T. ) ;
#10126 = DIRECTION ( 'NONE',  ( 0.000000000000000000, 0.9876883405951371042, 0.1564344650402347547 ) ) ;
#10127 = ORIENTED_EDGE ( 'NONE', *, *, #33805, .F. ) ;
#10128 = ORIENTED_EDGE ( 'NONE', *, *, #24401, .F. ) ;
#10129 = EDGE_CURVE ( 'NONE', #20327, #7093, #39891, .T. ) ;
#10130 = CARTESIAN_POINT ( 'NONE',  ( 10.00000000000000000, -21.32104025579091910, -30.84782396557241313 ) ) ;
#10131 = FACE_OUTER_BOUND ( 'NONE', #16018, .T. ) ;
#10132 = DIRECTION ( 'NONE',  ( -1.000000000000000000, 0.000000000000000000, 0.000000000000000000 ) ) ;
#10133 = EDGE_LOOP ( 'NONE', ( #20923, #47742, #26447, #24480 ) ) ;
#10134 = CARTESIAN_POINT ( 'NONE',  ( 0.000000000000000000, -27.05870788708250885, 26.08949754953014022 ) ) ;
#10135 = ORIENTED_EDGE ( 'NONE', *, *, #34739, .F. ) ;
#10136 = LINE ( 'NONE', #36328, #32721 ) ;
#10137 = CARTESIAN_POINT ( 'NONE',  ( -3.000000000000000000, -3.948201729842038432, -23.21447184625298021 ) ) ;
#10138 = DIRECTION ( 'NONE',  ( -1.000000000000000000, -0.000000000000000000, 0.000000000000000000 ) ) ;
#10139 = AXIS2_PLACEMENT_3D ( 'NONE', #18589, #13721, #22266 ) ;
#10140 = EDGE_LOOP ( 'NONE', ( #7067, #23923, #45046, #35225 ) ) ;
#10141 = VECTOR ( 'NONE', #36075, 1000.000000000000000 ) ;
#10142 = LINE ( 'NONE', #47813, #23218 ) ;
#10143 = VERTEX_POINT ( 'NONE', #10389 ) ;
#10144 = VERTEX_POINT ( 'NONE', #7196 ) ;
#10145 = CARTESIAN_POINT ( 'NONE',  ( -3.702536634196120335, 8.043911037661892749, -55.00000000000000000 ) ) ;
#10146 = AXIS2_PLACEMENT_3D ( 'NONE', #33536, #25209, #32578 ) ;
#10147 = CARTESIAN_POINT ( 'NONE',  ( 5.999999999999999112, 81.96053171279902472, -2.543863470248677316 ) ) ;
#10148 = CARTESIAN_POINT ( 'NONE',  ( 10.00000000000000000, 0.000000000000000000, 0.000000000000000000 ) ) ;
#10149 = DIRECTION ( 'NONE',  ( 0.000000000000000000, -0.5877852522924624790, -0.8090169943749551118 ) ) ;
#10150 = DIRECTION ( 'NONE',  ( 0.000000000000000000, 0.000000000000000000, 1.000000000000000000 ) ) ;
#10151 = DIRECTION ( 'NONE',  ( 1.000000000000000000, -0.000000000000000000, -0.000000000000000000 ) ) ;
#10152 = VECTOR ( 'NONE', #1376, 1000.000000000000000 ) ;
#10153 = CARTESIAN_POINT ( 'NONE',  ( 0.000000000000000000, -30.84782396557201878, -21.32104025579148399 ) ) ;
#10154 = DIRECTION ( 'NONE',  ( 0.000000000000000000, 0.000000000000000000, 1.000000000000000000 ) ) ;
#10155 = DIRECTION ( 'NONE',  ( 1.000000000000000000, -0.000000000000000000, 0.000000000000000000 ) ) ;
#10156 = CARTESIAN_POINT ( 'NONE',  ( 10.00000000000000000, 0.000000000000000000, 0.000000000000000000 ) ) ;
#10157 = ORIENTED_EDGE ( 'NONE', *, *, #978, .F. ) ;
#10158 = AXIS2_PLACEMENT_3D ( 'NONE', #2038, #39721, #16714 ) ;
#10159 = CARTESIAN_POINT ( 'NONE',  ( 10.00000000000000000, 37.48860685352291000, 0.8828120875901893649 ) ) ;
#10160 = EDGE_CURVE ( 'NONE', #10554, #34876, #21158, .T. ) ;
#10161 = DIRECTION ( 'NONE',  ( -1.000000000000000000, 0.000000000000000000, 0.000000000000000000 ) ) ;
#10162 = DIRECTION ( 'NONE',  ( -1.000000000000000000, 0.000000000000000000, 0.000000000000000000 ) ) ;
#10163 = CARTESIAN_POINT ( 'NONE',  ( 0.000000000000000000, -3.894527615418464705, 81.90746397400387480 ) ) ;
#10164 = CARTESIAN_POINT ( 'NONE',  ( 11.99999999999999822, 41.19522573413733113, 65.64334221924924861 ) ) ;
#10165 = DIRECTION ( 'NONE',  ( 1.000000000000000000, -0.000000000000000000, -0.000000000000000000 ) ) ;
#10167 = EDGE_CURVE ( 'NONE', #28423, #48250, #16447, .T. ) ;
#10166 = ORIENTED_EDGE ( 'NONE', *, *, #24212, .F. ) ;
#10168 = DIRECTION ( 'NONE',  ( 0.000000000000000000, 0.000000000000000000, 1.000000000000000000 ) ) ;
#10169 = DIRECTION ( 'NONE',  ( -1.000000000000000000, -0.000000000000000000, 0.000000000000000000 ) ) ;
#10170 = ORIENTED_EDGE ( 'NONE', *, *, #4137, .F. ) ;
#10171 = ORIENTED_EDGE ( 'NONE', *, *, #27871, .F. ) ;
#10172 = EDGE_CURVE ( 'NONE', #32236, #33332, #10645, .T. ) ;
#10173 = CIRCLE ( 'NONE', #26608, 12.49999999999999822 ) ;
#10174 = ORIENTED_EDGE ( 'NONE', *, *, #9495, .F. ) ;
#10175 = AXIS2_PLACEMENT_3D ( 'NONE', #39940, #43840, #32359 ) ;
#10176 = EDGE_CURVE ( 'NONE', #22407, #43729, #47111, .T. ) ;
#10177 = ORIENTED_EDGE ( 'NONE', *, *, #31969, .T. ) ;
#10178 = CIRCLE ( 'NONE', #16441, 31.99999999999999289 ) ;
#10179 = AXIS2_PLACEMENT_3D ( 'NONE', #45520, #37951, #22770 ) ;
#10180 = AXIS2_PLACEMENT_3D ( 'NONE', #12480, #43306, #23724 ) ;
#10181 = FACE_OUTER_BOUND ( 'NONE', #25701, .T. ) ;
#10182 = EDGE_LOOP ( 'NONE', ( #48117, #46192, #46504, #43371 ) ) ;
#10183 = AXIS2_PLACEMENT_3D ( 'NONE', #38486, #2024, #43126 ) ;
#10184 = CIRCLE ( 'NONE', #36074, 37.49900000000000944 ) ;
#10185 = ORIENTED_EDGE ( 'NONE', *, *, #47774, .F. ) ;
#10186 = EDGE_CURVE ( 'NONE', #26622, #46824, #33626, .T. ) ;
#10187 = CIRCLE ( 'NONE', #32112, 42.00000000000000000 ) ;
#10188 = CARTESIAN_POINT ( 'NONE',  ( 0.000000000000000000, -35.53030884539094103, 12.26510123303246935 ) ) ;
#10189 = CARTESIAN_POINT ( 'NONE',  ( 10.00000000000000000, 50.95692526931328104, 58.39081064771769292 ) ) ;
#10190 = ORIENTED_EDGE ( 'NONE', *, *, #4426, .T. ) ;
#10191 = CARTESIAN_POINT ( 'NONE',  ( 11.99999999999999822, -66.50666863321974631, -39.78640506895675344 ) ) ;
#10192 = EDGE_LOOP ( 'NONE', ( #12017, #22, #12678, #38471 ) ) ;
#10193 = VERTEX_POINT ( 'NONE', #2799 ) ;
#10194 = CARTESIAN_POINT ( 'NONE',  ( -10.00000000000000000, 0.000000000000000000, 0.000000000000000000 ) ) ;
#10195 = CARTESIAN_POINT ( 'NONE',  ( 0.000000000000000000, -36.72794159290197769, -65.59268652807249111 ) ) ;
#10196 = ADVANCED_FACE ( 'NONE', ( #32659 ), #28984, .T. ) ;
#10197 = CARTESIAN_POINT ( 'NONE',  ( -11.59517495878806947, -96.12423995607481686, 5.500000000000000000 ) ) ;
#10198 = ORIENTED_EDGE ( 'NONE', *, *, #26210, .F. ) ;
#10199 = ORIENTED_EDGE ( 'NONE', *, *, #376, .F. ) ;
#10200 = DIRECTION ( 'NONE',  ( -1.000000000000000000, 0.000000000000000000, -0.000000000000000000 ) ) ;
#10201 = ORIENTED_EDGE ( 'NONE', *, *, #1665, .F. ) ;
#10202 = LINE ( 'NONE', #32249, #38178 ) ;
#10203 = DIRECTION ( 'NONE',  ( 0.000000000000000000, 0.000000000000000000, 1.000000000000000000 ) ) ;
#10204 = DIRECTION ( 'NONE',  ( 0.6862798483830534479, 0.7273375899149810975, 0.000000000000000000 ) ) ;
#10205 = CARTESIAN_POINT ( 'NONE',  ( 11.99999999999999822, 36.72794159290334903, -65.59268652807170952 ) ) ;
#10206 = CARTESIAN_POINT ( 'NONE',  ( 15.00000000000000000, 23.49999999999999645, -1.500000000000003997 ) ) ;
#10207 = AXIS2_PLACEMENT_3D ( 'NONE', #8174, #1559, #42427 ) ;
#10208 = DIRECTION ( 'NONE',  ( -1.000000000000000000, 0.000000000000000000, 0.000000000000000000 ) ) ;
#10209 = ORIENTED_EDGE ( 'NONE', *, *, #19533, .T. ) ;
#10210 = VECTOR ( 'NONE', #39713, 1000.000000000000114 ) ;
#10211 = EDGE_CURVE ( 'NONE', #10070, #19886, #28948, .T. ) ;
#10212 = DIRECTION ( 'NONE',  ( -1.000000000000000000, 0.000000000000000000, 0.000000000000000000 ) ) ;
#10213 = ORIENTED_EDGE ( 'NONE', *, *, #43219, .T. ) ;
#10214 = VECTOR ( 'NONE', #24769, 999.9999999999998863 ) ;
#10215 = ADVANCED_FACE ( 'NONE', ( #8168 ), #38036, .F. ) ;
#10216 = CARTESIAN_POINT ( 'NONE',  ( 10.00000000000000000, 34.94270380257741948, -74.18225833017854143 ) ) ;
#10217 = DIRECTION ( 'NONE',  ( -1.000000000000000000, 0.000000000000000000, 0.000000000000000000 ) ) ;
#10218 = CARTESIAN_POINT ( 'NONE',  ( 0.000000000000000000, -38.55633173626998911, -16.65560815589452304 ) ) ;
#10219 = EDGE_CURVE ( 'NONE', #7964, #16286, #10184, .T. ) ;
#10220 = CIRCLE ( 'NONE', #47, 31.99999999999999289 ) ;
#10221 = EDGE_LOOP ( 'NONE', ( #32229, #31143, #14541, #18015 ) ) ;
#10222 = DIRECTION ( 'NONE',  ( 1.000000000000000000, 0.000000000000000000, 0.000000000000000000 ) ) ;
#10223 = DIRECTION ( 'NONE',  ( 0.000000000000000000, 0.9135454576426010886, -0.4067366430757998752 ) ) ;
#10224 = CARTESIAN_POINT ( 'NONE',  ( 26.47460221209471598, -121.8961639463267090, 5.500000000000000000 ) ) ;
#10225 = AXIS2_PLACEMENT_3D ( 'NONE', #27616, #43269, #12451 ) ;
#10226 = DIRECTION ( 'NONE',  ( -1.000000000000000000, -0.000000000000000000, -0.000000000000000000 ) ) ;
#10227 = LINE ( 'NONE', #25149, #43445 ) ;
#10228 = EDGE_CURVE ( 'NONE', #46458, #36027, #14992, .T. ) ;
#10229 = CARTESIAN_POINT ( 'NONE',  ( 11.99999999999999822, -77.16300072079681627, 27.74655509720640367 ) ) ;
#10230 = ORIENTED_EDGE ( 'NONE', *, *, #893, .T. ) ;
#10231 = ORIENTED_EDGE ( 'NONE', *, *, #16460, .T. ) ;
#10232 = EDGE_LOOP ( 'NONE', ( #22997, #18685, #18658, #32995 ) ) ;
#10233 = DIRECTION ( 'NONE',  ( 0.000000000000000000, -0.9781476007338041345, -0.2079116908177664480 ) ) ;
#10234 = FACE_OUTER_BOUND ( 'NONE', #19948, .T. ) ;
#10235 = ORIENTED_EDGE ( 'NONE', *, *, #37463, .T. ) ;
#10236 = EDGE_CURVE ( 'NONE', #37895, #32575, #22694, .T. ) ;
#10237 = AXIS2_PLACEMENT_3D ( 'NONE', #37104, #18508, #43732 ) ;
#10238 = DIRECTION ( 'NONE',  ( -0.000000000000000000, -0.000000000000000000, -1.000000000000000000 ) ) ;
#10239 = AXIS2_PLACEMENT_3D ( 'NONE', #34390, #15347, #8225 ) ;
#10240 = VECTOR ( 'NONE', #9520, 1000.000000000000227 ) ;
#10241 = ORIENTED_EDGE ( 'NONE', *, *, #10330, .F. ) ;
#10242 = ORIENTED_EDGE ( 'NONE', *, *, #36889, .F. ) ;
#10243 = ORIENTED_EDGE ( 'NONE', *, *, #48191, .T. ) ;
#10244 = ORIENTED_EDGE ( 'NONE', *, *, #456, .T. ) ;
#10245 = ADVANCED_FACE ( 'NONE', ( #23100 ), #30444, .T. ) ;
#10246 = CIRCLE ( 'NONE', #44632, 16.00000000000000355 ) ;
#10247 = AXIS2_PLACEMENT_3D ( 'NONE', #13949, #21766, #17365 ) ;
#10248 = CARTESIAN_POINT ( 'NONE',  ( 10.00000000000000000, -31.46837873495025306, 68.27212725128265447 ) ) ;
#10249 = VECTOR ( 'NONE', #27085, 1000.000000000000227 ) ;
#10250 = VERTEX_POINT ( 'NONE', #41957 ) ;
#10251 = CYLINDRICAL_SURFACE ( 'NONE', #36427, 82.00000000000000000 ) ;
#10252 = ORIENTED_EDGE ( 'NONE', *, *, #22385, .T. ) ;
#10253 = DIRECTION ( 'NONE',  ( -1.000000000000000000, 0.000000000000000000, 0.000000000000000000 ) ) ;
#10254 = CARTESIAN_POINT ( 'NONE',  ( 0.000000000000000000, 0.000000000000000000, 0.000000000000000000 ) ) ;
#10255 = DIRECTION ( 'NONE',  ( 1.000000000000000000, 0.000000000000000000, 0.000000000000000000 ) ) ;
#10256 = ORIENTED_EDGE ( 'NONE', *, *, #13428, .F. ) ;
#10257 = DIRECTION ( 'NONE',  ( -1.000000000000000000, 0.000000000000000000, 0.000000000000000000 ) ) ;
#10258 = ORIENTED_EDGE ( 'NONE', *, *, #4216, .T. ) ;
#10259 = CARTESIAN_POINT ( 'NONE',  ( -3.000000000000000000, 0.000000000000000000, 0.000000000000000000 ) ) ;
#10260 = FACE_OUTER_BOUND ( 'NONE', #9292, .T. ) ;
#10261 = ORIENTED_EDGE ( 'NONE', *, *, #37960, .T. ) ;
#10262 = ORIENTED_EDGE ( 'NONE', *, *, #15529, .T. ) ;
#10263 = EDGE_CURVE ( 'NONE', #44807, #46921, #4019, .T. ) ;
#10264 = CARTESIAN_POINT ( 'NONE',  ( 10.00000000000000000, -12.42422080174614862, -35.38097989696524337 ) ) ;
#10265 = LINE ( 'NONE', #17848, #16032 ) ;
#10266 = EDGE_LOOP ( 'NONE', ( #36371, #28776, #40455, #29392 ) ) ;
#10267 = ORIENTED_EDGE ( 'NONE', *, *, #6264, .T. ) ;
#10268 = CARTESIAN_POINT ( 'NONE',  ( 10.00000000000000000, -10.96151621346514382, 35.95386929396252640 ) ) ;
#10269 = CARTESIAN_POINT ( 'NONE',  ( 10.00000000000000000, 0.000000000000000000, 0.000000000000000000 ) ) ;
#10270 = CARTESIAN_POINT ( 'NONE',  ( -10.00000000000000000, 0.000000000000000000, 0.000000000000000000 ) ) ;
#10271 = EDGE_CURVE ( 'NONE', #5836, #47967, #37548, .T. ) ;
#10272 = DIRECTION ( 'NONE',  ( -1.000000000000000000, 0.000000000000000000, 0.000000000000000000 ) ) ;
#10274 = AXIS2_PLACEMENT_3D ( 'NONE', #23173, #14865, #15827 ) ;
#10273 = DIRECTION ( 'NONE',  ( -1.000000000000000000, 0.000000000000000000, -0.000000000000000000 ) ) ;
#10275 = VECTOR ( 'NONE', #29758, 1000.000000000000000 ) ;
#10276 = DIRECTION ( 'NONE',  ( -1.000000000000000000, 0.000000000000000000, 0.000000000000000000 ) ) ;
#10277 = DIRECTION ( 'NONE',  ( -1.000000000000000000, -0.000000000000000000, 0.000000000000000000 ) ) ;
#10278 = EDGE_CURVE ( 'NONE', #13273, #47647, #35207, .T. ) ;
#10279 = CIRCLE ( 'NONE', #111, 37.49900000000000944 ) ;
#10280 = AXIS2_PLACEMENT_3D ( 'NONE', #11425, #3819, #18734 ) ;
#10281 = EDGE_CURVE ( 'NONE', #35877, #44453, #3527, .T. ) ;
#10282 = DIRECTION ( 'NONE',  ( 0.3853207896976547087, -0.9227826878668540234, 0.000000000000000000 ) ) ;
#10283 = LINE ( 'NONE', #44537, #20663 ) ;
#10284 = DIRECTION ( 'NONE',  ( -1.000000000000000000, 0.000000000000000000, -0.000000000000000000 ) ) ;
#10285 = DIRECTION ( 'NONE',  ( -1.000000000000000000, 0.000000000000000000, -0.000000000000000000 ) ) ;
#10286 = VECTOR ( 'NONE', #23889, 1000.000000000000000 ) ;
#10287 = ORIENTED_EDGE ( 'NONE', *, *, #26993, .T. ) ;
#10288 = ORIENTED_EDGE ( 'NONE', *, *, #26691, .T. ) ;
#10289 = CARTESIAN_POINT ( 'NONE',  ( 10.00000000000000000, -35.38097989696520074, 12.42422080174625520 ) ) ;
#10290 = VECTOR ( 'NONE', #12262, 1000.000000000000000 ) ;
#10291 = CARTESIAN_POINT ( 'NONE',  ( -3.000000000000000000, 9.615535125378775305, 24.73947219025917121 ) ) ;
#10292 = ORIENTED_EDGE ( 'NONE', *, *, #32060, .T. ) ;
#10293 = DIRECTION ( 'NONE',  ( -1.000000000000000000, 0.000000000000000000, 0.000000000000000000 ) ) ;
#10294 = EDGE_LOOP ( 'NONE', ( #8346, #46683, #15996, #38874 ) ) ;
#10295 = CARTESIAN_POINT ( 'NONE',  ( 10.00000000000000000, 25.88420570971438650, -27.13269053701069566 ) ) ;
#10296 = ORIENTED_EDGE ( 'NONE', *, *, #43226, .T. ) ;
#10297 = CARTESIAN_POINT ( 'NONE',  ( 0.000000000000000000, 37.16516213103277266, 4.992566952385114831 ) ) ;
#10298 = AXIS2_PLACEMENT_3D ( 'NONE', #31017, #17022, #12886 ) ;
#10299 = ORIENTED_EDGE ( 'NONE', *, *, #1530, .T. ) ;
#10300 = FACE_OUTER_BOUND ( 'NONE', #70, .T. ) ;
#10301 = VERTEX_POINT ( 'NONE', #12100 ) ;
#10302 = DIRECTION ( 'NONE',  ( -1.000000000000000000, 0.000000000000000000, -0.000000000000000000 ) ) ;
#10303 = ORIENTED_EDGE ( 'NONE', *, *, #15599, .T. ) ;
#10304 = LINE ( 'NONE', #25223, #40003 ) ;
#10305 = VECTOR ( 'NONE', #45065, 1000.000000000000000 ) ;
#10306 = EDGE_CURVE ( 'NONE', #11779, #42231, #4271, .T. ) ;
#10307 = ORIENTED_EDGE ( 'NONE', *, *, #9061, .T. ) ;
#10308 = DIRECTION ( 'NONE',  ( -1.000000000000000000, 0.000000000000000000, 0.000000000000000000 ) ) ;
#10309 = DIRECTION ( 'NONE',  ( 0.000000000000000000, 0.4067366430757989870, 0.9135454576426015327 ) ) ;
#10310 = EDGE_CURVE ( 'NONE', #33538, #12545, #14881, .T. ) ;
#10311 = AXIS2_PLACEMENT_3D ( 'NONE', #9198, #24131, #46890 ) ;
#10312 = DIRECTION ( 'NONE',  ( -1.000000000000000000, -0.000000000000000000, -0.000000000000000000 ) ) ;
#10313 = DIRECTION ( 'NONE',  ( 1.000000000000000000, 0.000000000000000000, 0.000000000000000000 ) ) ;
#10314 = DIRECTION ( 'NONE',  ( 1.000000000000000000, 0.000000000000000000, 0.000000000000000000 ) ) ;
#10315 = CARTESIAN_POINT ( 'NONE',  ( 10.00000000000000000, -6.736453364083292428, -36.88895765772640800 ) ) ;
#10316 = VERTEX_POINT ( 'NONE', #22850 ) ;
#10317 = CARTESIAN_POINT ( 'NONE',  ( 13.83832728059186046, -142.6495187161941089, -5.500000000000000000 ) ) ;
#10318 = EDGE_LOOP ( 'NONE', ( #33965, #4481, #12484, #764 ) ) ;
#10319 = ORIENTED_EDGE ( 'NONE', *, *, #23644, .T. ) ;
#10320 = DIRECTION ( 'NONE',  ( -0.4796670183876294291, 0.8774505977381983346, 0.000000000000000000 ) ) ;
#10321 = DIRECTION ( 'NONE',  ( 0.000000000000000000, 0.000000000000000000, 1.000000000000000000 ) ) ;
#10322 = ORIENTED_EDGE ( 'NONE', *, *, #12664, .T. ) ;
#10323 = VECTOR ( 'NONE', #17832, 1000.000000000000000 ) ;
#10324 = DIRECTION ( 'NONE',  ( 0.000000000000000000, -0.9876883405951359940, -0.1564344650402420267 ) ) ;
#10325 = DIRECTION ( 'NONE',  ( 0.000000000000000000, 0.000000000000000000, 1.000000000000000000 ) ) ;
#10326 = DIRECTION ( 'NONE',  ( -1.000000000000000000, 0.000000000000000000, -0.000000000000000000 ) ) ;
#10327 = ORIENTED_EDGE ( 'NONE', *, *, #42211, .T. ) ;
#10328 = EDGE_CURVE ( 'NONE', #34129, #36599, #47021, .T. ) ;
#10329 = CARTESIAN_POINT ( 'NONE',  ( 0.000000000000000000, -14.67089635893658794, -73.72996012237454977 ) ) ;
#10330 = EDGE_CURVE ( 'NONE', #25379, #31758, #25898, .T. ) ;
#10331 = EDGE_CURVE ( 'NONE', #47530, #12539, #30215, .T. ) ;
#10332 = DIRECTION ( 'NONE',  ( 0.000000000000000000, 0.3090169943749480619, -0.9510565162951533091 ) ) ;
#10333 = PLANE ( 'NONE',  #48165 ) ;
#10334 = ORIENTED_EDGE ( 'NONE', *, *, #26979, .F. ) ;
#10335 = CARTESIAN_POINT ( 'NONE',  ( 0.000000000000000000, -35.91791733033426226, -68.67312586195033930 ) ) ;
#10336 = LINE ( 'NONE', #2275, #3558 ) ;
#10337 = DIRECTION ( 'NONE',  ( -1.000000000000000000, -0.000000000000000000, -0.000000000000000000 ) ) ;
#10338 = DIRECTION ( 'NONE',  ( 1.390371824233641368E-16, -1.000000000000000000, 0.000000000000000000 ) ) ;
#10339 = EDGE_CURVE ( 'NONE', #22480, #3571, #33393, .T. ) ;
#10340 = CIRCLE ( 'NONE', #39269, 13.90444123027096879 ) ;
#10341 = ORIENTED_EDGE ( 'NONE', *, *, #42452, .F. ) ;
#10342 = EDGE_CURVE ( 'NONE', #45628, #1817, #48313, .T. ) ;
#10343 = DIRECTION ( 'NONE',  ( 0.000000000000000000, 0.000000000000000000, 1.000000000000000000 ) ) ;
#10344 = LINE ( 'NONE', #18651, #12821 ) ;
#10345 = CARTESIAN_POINT ( 'NONE',  ( 10.00000000000000000, -26.08949754953044220, 27.05870788708222818 ) ) ;
#10346 = DIRECTION ( 'NONE',  ( -1.000000000000000000, -0.000000000000000000, 0.000000000000000000 ) ) ;
#10347 = VERTEX_POINT ( 'NONE', #37783 ) ;
#10348 = CIRCLE ( 'NONE', #15065, 31.99999999999999289 ) ;
#10349 = VERTEX_POINT ( 'NONE', #87 ) ;
#10350 = CIRCLE ( 'NONE', #41618, 37.49900000000001654 ) ;
#10351 = DIRECTION ( 'NONE',  ( 0.000000000000000000, -0.5000000000000028866, -0.8660254037844369313 ) ) ;
#10352 = ORIENTED_EDGE ( 'NONE', *, *, #40618, .T. ) ;
#10353 = DIRECTION ( 'NONE',  ( -1.000000000000000000, 0.000000000000000000, 0.000000000000000000 ) ) ;
#10354 = CIRCLE ( 'NONE', #42396, 0.5000000000000004441 ) ;
#10355 =( LENGTH_UNIT ( ) NAMED_UNIT ( * ) SI_UNIT ( .MILLI., .METRE. ) );
#10356 = DIRECTION ( 'NONE',  ( -1.000000000000000000, -0.000000000000000000, -0.000000000000000000 ) ) ;
#10357 = CIRCLE ( 'NONE', #25193, 16.00000000000000000 ) ;
#10358 = ORIENTED_EDGE ( 'NONE', *, *, #27721, .T. ) ;
#10359 = VECTOR ( 'NONE', #25313, 1000.000000000000000 ) ;
#10360 = AXIS2_PLACEMENT_3D ( 'NONE', #23655, #31029, #34664 ) ;
#10361 = CARTESIAN_POINT ( 'NONE',  ( 10.00000000000000000, -22.48208911017525580, 35.47612816024516036 ) ) ;
#10362 = ORIENTED_EDGE ( 'NONE', *, *, #31922, .T. ) ;
#10363 = ADVANCED_FACE ( 'NONE', ( #15034 ), #29954, .T. ) ;
#10364 = EDGE_CURVE ( 'NONE', #14290, #12132, #9136, .T. ) ;
#10365 = DIRECTION ( 'NONE',  ( 0.000000000000000000, 0.000000000000000000, 1.000000000000000000 ) ) ;
#10366 = ORIENTED_EDGE ( 'NONE', *, *, #19208, .F. ) ;
#10367 = DIRECTION ( 'NONE',  ( 0.000000000000000000, 0.000000000000000000, 1.000000000000000000 ) ) ;
#10368 = DIRECTION ( 'NONE',  ( 0.000000000000000000, 0.000000000000000000, 1.000000000000000000 ) ) ;
#10369 = AXIS2_PLACEMENT_3D ( 'NONE', #48197, #32551, #37182 ) ;
#10370 = EDGE_CURVE ( 'NONE', #451, #20, #13290, .T. ) ;
#10371 = ORIENTED_EDGE ( 'NONE', *, *, #18887, .T. ) ;
#10372 = CARTESIAN_POINT ( 'NONE',  ( 0.000000000000000000, -34.94270380257693631, 74.18225833017875459 ) ) ;
#10373 = VECTOR ( 'NONE', #15968, 1000.000000000000000 ) ;
#10374 = EDGE_CURVE ( 'NONE', #30611, #1277, #40646, .T. ) ;
#10375 = ORIENTED_EDGE ( 'NONE', *, *, #41446, .F. ) ;
#10376 = DIRECTION ( 'NONE',  ( 0.000000000000000000, 0.000000000000000000, 1.000000000000000000 ) ) ;
#10377 = CARTESIAN_POINT ( 'NONE',  ( 10.00000000000000000, 33.79645857604513992, -16.45098606841138178 ) ) ;
#10378 = LINE ( 'NONE', #32429, #20401 ) ;
#10379 = VECTOR ( 'NONE', #29375, 1000.000000000000000 ) ;
#10380 = VECTOR ( 'NONE', #11549, 1000.000000000000114 ) ;
#10381 = VERTEX_POINT ( 'NONE', #27753 ) ;
#10382 = DIRECTION ( 'NONE',  ( 1.000000000000000000, -0.000000000000000000, 0.000000000000000000 ) ) ;
#10383 = VERTEX_POINT ( 'NONE', #42677 ) ;
#10384 = VERTEX_POINT ( 'NONE', #28213 ) ;
#10385 = VECTOR ( 'NONE', #14668, 1000.000000000000000 ) ;
#10386 = DIRECTION ( 'NONE',  ( -1.000000000000000000, 0.000000000000000000, -0.000000000000000000 ) ) ;
#10387 = CARTESIAN_POINT ( 'NONE',  ( -10.00000000000000000, 0.000000000000000000, 0.000000000000000000 ) ) ;
#10388 = AXIS2_PLACEMENT_3D ( 'NONE', #35426, #8753, #46213 ) ;
#10389 = CARTESIAN_POINT ( 'NONE',  ( 0.000000000000000000, 74.18225833017888249, 34.94270380257665209 ) ) ;
#10390 = DIRECTION ( 'NONE',  ( 0.000000000000000000, -0.9510565162951500895, -0.3090169943749583314 ) ) ;
#10391 = ORIENTED_EDGE ( 'NONE', *, *, #39800, .T. ) ;
#10392 = DIRECTION ( 'NONE',  ( -1.000000000000000000, 0.000000000000000000, 0.000000000000000000 ) ) ;
#10393 = DIRECTION ( 'NONE',  ( 1.000000000000000000, 0.000000000000000000, 0.000000000000000000 ) ) ;
#10394 = EDGE_CURVE ( 'NONE', #3684, #46691, #19898, .T. ) ;
#10395 = EDGE_CURVE ( 'NONE', #36977, #17963, #4708, .T. ) ;
#10396 = DIRECTION ( 'NONE',  ( -1.000000000000000000, 0.000000000000000000, 0.000000000000000000 ) ) ;
#10397 = CARTESIAN_POINT ( 'NONE',  ( 0.000000000000000000, -33.79645857604501913, -16.45098606841161626 ) ) ;
#10398 = DIRECTION ( 'NONE',  ( 0.000000000000000000, 0.4067366430757887730, -0.9135454576426059736 ) ) ;
#10399 = VERTEX_POINT ( 'NONE', #46592 ) ;
#10400 = AXIS2_PLACEMENT_3D ( 'NONE', #9602, #24304, #17427 ) ;
#10401 = ORIENTED_EDGE ( 'NONE', *, *, #31339, .T. ) ;
#10402 = DIRECTION ( 'NONE',  ( -1.000000000000000000, -0.000000000000000000, -0.000000000000000000 ) ) ;
#10403 = AXIS2_PLACEMENT_3D ( 'NONE', #1341, #45895, #34131 ) ;
#10404 = CARTESIAN_POINT ( 'NONE',  ( -114.1267819554185365, -82.91796067500661138, 5.500000000000000000 ) ) ;
#10405 = DIRECTION ( 'NONE',  ( -0.6575728627325957421, 0.7533909544171994987, 0.000000000000000000 ) ) ;
#10406 = CYLINDRICAL_SURFACE ( 'NONE', #11410, 16.00000000000000000 ) ;
#10407 = EDGE_CURVE ( 'NONE', #8188, #40043, #14142, .T. ) ;
#10408 = FACE_OUTER_BOUND ( 'NONE', #31470, .T. ) ;
#10409 = CARTESIAN_POINT ( 'NONE',  ( 10.00000000000000000, -31.52238457039619490, 27.75498641678731104 ) ) ;
#10410 = VERTEX_POINT ( 'NONE', #5459 ) ;
#10411 = PLANE ( 'NONE',  #44961 ) ;
#10412 = CIRCLE ( 'NONE', #20576, 77.49900000000000944 ) ;
#10413 = LINE ( 'NONE', #11144, #5659 ) ;
#10414 = ORIENTED_EDGE ( 'NONE', *, *, #19943, .F. ) ;
#10415 = EDGE_LOOP ( 'NONE', ( #43856, #16283, #41653, #36118 ) ) ;
#10416 = ORIENTED_EDGE ( 'NONE', *, *, #30802, .F. ) ;
#10417 = VECTOR ( 'NONE', #20203, 1000.000000000000000 ) ;
#10418 = CIRCLE ( 'NONE', #30769, 42.00000000000000000 ) ;
#10419 = DIRECTION ( 'NONE',  ( -1.000000000000000000, -0.000000000000000000, 0.000000000000000000 ) ) ;
#10420 = VERTEX_POINT ( 'NONE', #13057 ) ;
#10421 = CIRCLE ( 'NONE', #4181, 16.00000000000000000 ) ;
#10422 = VERTEX_POINT ( 'NONE', #20625 ) ;
#10423 = ADVANCED_FACE ( 'NONE', ( #30944 ), #38999, .T. ) ;
#10424 = AXIS2_PLACEMENT_3D ( 'NONE', #11090, #4710, #38743 ) ;
#10425 = AXIS2_PLACEMENT_3D ( 'NONE', #1869, #35636, #24620 ) ;
#10426 = FACE_OUTER_BOUND ( 'NONE', #34734, .T. ) ;
#10427 = AXIS2_PLACEMENT_3D ( 'NONE', #20820, #28396, #35747 ) ;
#10428 = CYLINDRICAL_SURFACE ( 'NONE', #45287, 42.00000000000000000 ) ;
#10429 = CIRCLE ( 'NONE', #34631, 77.49900000000000944 ) ;
#10430 = PLANE ( 'NONE',  #10540 ) ;
#10431 = EDGE_CURVE ( 'NONE', #1684, #44007, #12811, .T. ) ;
#10432 = ORIENTED_EDGE ( 'NONE', *, *, #31700, .F. ) ;
#10433 = FACE_OUTER_BOUND ( 'NONE', #24106, .T. ) ;
#10434 = EDGE_LOOP ( 'NONE', ( #4529, #14508, #36398, #9440 ) ) ;
#10435 = ORIENTED_EDGE ( 'NONE', *, *, #38081, .F. ) ;
#10436 = EDGE_CURVE ( 'NONE', #23140, #33476, #34833, .T. ) ;
#10437 = ORIENTED_EDGE ( 'NONE', *, *, #14266, .F. ) ;
#10438 = CIRCLE ( 'NONE', #15132, 16.00000000000000000 ) ;
#10439 = LINE ( 'NONE', #40540, #27222 ) ;
#10440 = DIRECTION ( 'NONE',  ( 0.000000000000000000, 0.000000000000000000, 1.000000000000000000 ) ) ;
#10441 = PLANE ( 'NONE',  #18058 ) ;
#10442 = ORIENTED_EDGE ( 'NONE', *, *, #5131, .T. ) ;
#10443 = ORIENTED_EDGE ( 'NONE', *, *, #6674, .T. ) ;
#10444 = LINE ( 'NONE', #25605, #3647 ) ;
#10445 = ORIENTED_EDGE ( 'NONE', *, *, #9703, .T. ) ;
#10446 = DIRECTION ( 'NONE',  ( 0.000000000000000000, -0.9781476007338040235, -0.2079116908177671419 ) ) ;
#10447 = DIRECTION ( 'NONE',  ( 0.000000000000000000, 0.000000000000000000, 1.000000000000000000 ) ) ;
#10448 = DIRECTION ( 'NONE',  ( -1.000000000000000000, -0.000000000000000000, 0.000000000000000000 ) ) ;
#10449 = VERTEX_POINT ( 'NONE', #31914 ) ;
#10450 = CARTESIAN_POINT ( 'NONE',  ( 6.938893903907228378E-15, 0.000000000000000000, 0.000000000000000000 ) ) ;
#10451 = DIRECTION ( 'NONE',  ( -1.000000000000000000, -0.000000000000000000, -0.000000000000000000 ) ) ;
#10452 = DIRECTION ( 'NONE',  ( 0.000000000000000000, 0.000000000000000000, 1.000000000000000000 ) ) ;
#10453 = ADVANCED_FACE ( 'NONE', ( #5234 ), #20376, .T. ) ;
#10454 = EDGE_CURVE ( 'NONE', #32354, #5700, #35566, .T. ) ;
#10455 = AXIS2_PLACEMENT_3D ( 'NONE', #2396, #13675, #43762 ) ;
#10456 = FACE_OUTER_BOUND ( 'NONE', #254, .T. ) ;
#10457 = DIRECTION ( 'NONE',  ( -1.000000000000000000, -0.000000000000000000, -0.000000000000000000 ) ) ;
#10458 = ORIENTED_EDGE ( 'NONE', *, *, #14991, .F. ) ;
#10459 = EDGE_CURVE ( 'NONE', #45965, #10316, #39929, .T. ) ;
#10460 = CARTESIAN_POINT ( 'NONE',  ( 10.00000000000000000, 0.000000000000000000, 0.000000000000000000 ) ) ;
#10461 = EDGE_LOOP ( 'NONE', ( #44314, #4163, #13938, #26516 ) ) ;
#10462 = CIRCLE ( 'NONE', #1880, 12.50000000000000000 ) ;
#10463 = AXIS2_PLACEMENT_3D ( 'NONE', #11462, #26381, #37630 ) ;
#10464 = CARTESIAN_POINT ( 'NONE',  ( -3.000000000000000000, -10.45096189432314837, -21.10159698893440350 ) ) ;
#10465 = CARTESIAN_POINT ( 'NONE',  ( 10.00000000000000000, -71.27951684758046724, 30.41916302227088309 ) ) ;
#10466 = CYLINDRICAL_SURFACE ( 'NONE', #23668, 42.00000000000000000 ) ;
#10467 = FACE_OUTER_BOUND ( 'NONE', #1160, .T. ) ;
#10468 = CARTESIAN_POINT ( 'NONE',  ( 10.00000000000000000, -6.555932627142676772, 37.01155633439056203 ) ) ;
#10469 = EDGE_CURVE ( 'NONE', #29809, #21999, #23334, .T. ) ;
#10470 = EDGE_LOOP ( 'NONE', ( #27142, #8258, #34593, #10729 ) ) ;
#10471 = AXIS2_PLACEMENT_3D ( 'NONE', #29137, #44077, #10555 ) ;
#10472 = VECTOR ( 'NONE', #16741, 1000.000000000000000 ) ;
#10473 = LINE ( 'NONE', #21489, #19282 ) ;
#10474 = CARTESIAN_POINT ( 'NONE',  ( 0.000000000000000000, 41.81611651403868990, -3.925862922255709542 ) ) ;
#10475 = CIRCLE ( 'NONE', #16738, 16.00000000000000000 ) ;
#10476 = AXIS2_PLACEMENT_3D ( 'NONE', #24979, #6391, #25459 ) ;
#10477 = CARTESIAN_POINT ( 'NONE',  ( 0.000000000000000000, -75.11764819372145041, -2.946379043147127064 ) ) ;
#10478 = SURFACE_SIDE_STYLE ('',( #10958 ) ) ;
#10479 = CIRCLE ( 'NONE', #22220, 82.00000000000000000 ) ;
#10480 = ORIENTED_EDGE ( 'NONE', *, *, #19923, .F. ) ;
#10481 = ORIENTED_EDGE ( 'NONE', *, *, #8458, .F. ) ;
#10482 = DIRECTION ( 'NONE',  ( -1.000000000000000000, -0.000000000000000000, -0.000000000000000000 ) ) ;
#10483 = LINE ( 'NONE', #35943, #44122 ) ;
#10484 = EDGE_LOOP ( 'NONE', ( #5312, #16880, #42672, #47593 ) ) ;
#10485 = DIRECTION ( 'NONE',  ( -1.000000000000000000, -0.000000000000000000, -0.000000000000000000 ) ) ;
#10486 = VECTOR ( 'NONE', #16727, 1000.000000000000000 ) ;
#10487 = VECTOR ( 'NONE', #3548, 1000.000000000000114 ) ;
#10488 = ADVANCED_FACE ( 'NONE', ( #8886 ), #16724, .T. ) ;
#10489 = ORIENTED_EDGE ( 'NONE', *, *, #19347, .T. ) ;
#10490 = ORIENTED_EDGE ( 'NONE', *, *, #14264, .T. ) ;
#10491 = VECTOR ( 'NONE', #10865, 1000.000000000000000 ) ;
#10492 = PRODUCT ( 'big gear_ISO - Spur gear 2M 80T 20PA 10FW ---S80A75H50L20.0N', 'big gear_ISO - Spur gear 2M 80T 20PA 10FW ---S80A75H50L20.0N', '', ( #45329 ) ) ;
#10493 = EDGE_CURVE ( 'NONE', #37347, #22843, #7881, .T. ) ;
#10494 = ADVANCED_FACE ( 'NONE', ( #2046 ), #23825, .T. ) ;
#10495 = EDGE_CURVE ( 'NONE', #39822, #2924, #38357, .T. ) ;
#10496 = CARTESIAN_POINT ( 'NONE',  ( 10.00000000000000000, 0.000000000000000000, 0.000000000000000000 ) ) ;
#10497 = VECTOR ( 'NONE', #14926, 1000.000000000000000 ) ;
#10498 = EDGE_CURVE ( 'NONE', #33807, #1013, #36769, .T. ) ;
#10499 = ORIENTED_EDGE ( 'NONE', *, *, #47869, .F. ) ;
#10500 = CARTESIAN_POINT ( 'NONE',  ( 5.000000000000002665, 34.94270380257639630, 74.18225833017899618 ) ) ;
#10501 = EDGE_CURVE ( 'NONE', #23315, #27986, #24790, .T. ) ;
#10502 = VERTEX_POINT ( 'NONE', #32607 ) ;
#10503 = AXIS2_PLACEMENT_3D ( 'NONE', #12402, #4569, #26602 ) ;
#10504 = DIRECTION ( 'NONE',  ( -1.000000000000000000, 0.000000000000000000, 0.000000000000000000 ) ) ;
#10505 = CIRCLE ( 'NONE', #28478, 15.99999999999999822 ) ;
#10506 = DIRECTION ( 'NONE',  ( -1.000000000000000000, 0.000000000000000000, 0.000000000000000000 ) ) ;
#10507 = DIRECTION ( 'NONE',  ( 0.000000000000000000, -0.000000000000000000, 1.000000000000000000 ) ) ;
#10509 = ORIENTED_EDGE ( 'NONE', *, *, #4690, .T. ) ;
#10508 = AXIS2_PLACEMENT_3D ( 'NONE', #29857, #30115, #45040 ) ;
#10510 = ORIENTED_EDGE ( 'NONE', *, *, #37028, .T. ) ;
#10511 = DIRECTION ( 'NONE',  ( -1.000000000000000000, -0.000000000000000000, -0.000000000000000000 ) ) ;
#10512 = DIRECTION ( 'NONE',  ( 0.000000000000000000, 0.7431448254773939111, 0.6691306063588584596 ) ) ;
#10513 = ORIENTED_EDGE ( 'NONE', *, *, #41227, .T. ) ;
#10514 = VERTEX_POINT ( 'NONE', #39489 ) ;
#10515 = EDGE_CURVE ( 'NONE', #28565, #30318, #39965, .T. ) ;
#10516 = FACE_OUTER_BOUND ( 'NONE', #29643, .T. ) ;
#10517 = CARTESIAN_POINT ( 'NONE',  ( 15.00000000000000000, -23.29833615347109088, -3.418703333116486665 ) ) ;
#10518 = ORIENTED_EDGE ( 'NONE', *, *, #24319, .T. ) ;
#10519 = ORIENTED_EDGE ( 'NONE', *, *, #26869, .T. ) ;
#10520 = DIRECTION ( 'NONE',  ( -1.000000000000000000, -0.000000000000000000, 0.000000000000000000 ) ) ;
#10521 = DIRECTION ( 'NONE',  ( 0.000000000000000000, 0.000000000000000000, 1.000000000000000000 ) ) ;
#10522 = CARTESIAN_POINT ( 'NONE',  ( -10.00000000000000000, 0.000000000000000000, 0.000000000000000000 ) ) ;
#10523 = ORIENTED_EDGE ( 'NONE', *, *, #12779, .T. ) ;
#10524 = CYLINDRICAL_SURFACE ( 'NONE', #39854, 37.49900000000000233 ) ;
#10525 = DIRECTION ( 'NONE',  ( -1.000000000000000000, 0.000000000000000000, 0.000000000000000000 ) ) ;
#10526 = EDGE_CURVE ( 'NONE', #46424, #30381, #32141, .T. ) ;
#10527 = ORIENTED_EDGE ( 'NONE', *, *, #4510, .F. ) ;
#10528 = CYLINDRICAL_SURFACE ( 'NONE', #1278, 42.00000000000000000 ) ;
#10529 = DIRECTION ( 'NONE',  ( 0.000000000000000000, -0.7071067811865388020, -0.7071067811865561215 ) ) ;
#10530 = CIRCLE ( 'NONE', #30061, 42.00000000000000000 ) ;
#10531 = AXIS2_PLACEMENT_3D ( 'NONE', #21362, #17927, #36771 ) ;
#10532 = CYLINDRICAL_SURFACE ( 'NONE', #11219, 16.00000000000000000 ) ;
#10533 = DIRECTION ( 'NONE',  ( -0.000000000000000000, -0.000000000000000000, 1.000000000000000000 ) ) ;
#10534 = CARTESIAN_POINT ( 'NONE',  ( 0.000000000000000000, 0.000000000000000000, 0.000000000000000000 ) ) ;
#10535 = ORIENTED_EDGE ( 'NONE', *, *, #31522, .T. ) ;
#10536 = ORIENTED_EDGE ( 'NONE', *, *, #10436, .T. ) ;
#10537 = ORIENTED_EDGE ( 'NONE', *, *, #31152, .T. ) ;
#10538 = ORIENTED_EDGE ( 'NONE', *, *, #36519, .F. ) ;
#10539 = EDGE_CURVE ( 'NONE', #46560, #41161, #27423, .T. ) ;
#10540 = AXIS2_PLACEMENT_3D ( 'NONE', #48352, #25348, #14833 ) ;
#10541 = VECTOR ( 'NONE', #3788, 1000.000000000000000 ) ;
#10542 = UNCERTAINTY_MEASURE_WITH_UNIT (LENGTH_MEASURE( 1.000000000000000082E-05 ), #22993, 'distance_accuracy_value', 'NONE');
#10543 = VECTOR ( 'NONE', #8475, 1000.000000000000000 ) ;
#10544 = DIRECTION ( 'NONE',  ( 0.000000000000000000, 0.9945218953682740670, 0.1045284632676459352 ) ) ;
#10545 = ORIENTED_EDGE ( 'NONE', *, *, #45822, .T. ) ;
#10546 = VECTOR ( 'NONE', #24, 1000.000000000000000 ) ;
#10547 = DIRECTION ( 'NONE',  ( 1.000000000000000000, -0.000000000000000000, -0.000000000000000000 ) ) ;
#10548 = VECTOR ( 'NONE', #33672, 1000.000000000000000 ) ;
#10549 = VERTEX_POINT ( 'NONE', #2499 ) ;
#10550 = EDGE_CURVE ( 'NONE', #19364, #13412, #40207, .T. ) ;
#10551 = ORIENTED_EDGE ( 'NONE', *, *, #31424, .F. ) ;
#10552 = EDGE_CURVE ( 'NONE', #40846, #5216, #43629, .T. ) ;
#10553 = CARTESIAN_POINT ( 'NONE',  ( 0.000000000000000000, -4.992566952384716927, -37.16516213103282951 ) ) ;
#10554 = VERTEX_POINT ( 'NONE', #10093 ) ;
#10555 = DIRECTION ( 'NONE',  ( 0.000000000000000000, 0.000000000000000000, 1.000000000000000000 ) ) ;
#10556 = ORIENTED_EDGE ( 'NONE', *, *, #40243, .F. ) ;
#10558 = EDGE_CURVE ( 'NONE', #17233, #9394, #36516, .T. ) ;
#10557 = DIRECTION ( 'NONE',  ( -1.000000000000000000, -0.000000000000000000, -0.000000000000000000 ) ) ;
#10559 = ADVANCED_FACE ( 'NONE', ( #44108 ), #43865, .F. ) ;
#10560 = AXIS2_PLACEMENT_3D ( 'NONE', #44418, #37066, #13414 ) ;
#10561 = DIRECTION ( 'NONE',  ( 0.000000000000000000, 1.000000000000000000, 3.491481338843133355E-15 ) ) ;
#10562 = ORIENTED_EDGE ( 'NONE', *, *, #31766, .T. ) ;
#10563 = ADVANCED_FACE ( 'NONE', ( #21823 ), #2981, .T. ) ;
#10564 = FACE_OUTER_BOUND ( 'NONE', #40227, .T. ) ;
#10565 = ORIENTED_EDGE ( 'NONE', *, *, #15103, .T. ) ;
#10566 = VECTOR ( 'NONE', #22124, 1000.000000000000000 ) ;
#10567 = CARTESIAN_POINT ( 'NONE',  ( -10.00000000000000000, 0.000000000000000000, 0.000000000000000000 ) ) ;
#10568 = VERTEX_POINT ( 'NONE', #25244 ) ;
#10569 = DIRECTION ( 'NONE',  ( -1.000000000000000000, 0.000000000000000000, -0.000000000000000000 ) ) ;
#10570 = CARTESIAN_POINT ( 'NONE',  ( 0.000000000000000000, 10.96151621346540317, -35.95386929396244113 ) ) ;
#10571 = ORIENTED_EDGE ( 'NONE', *, *, #38834, .F. ) ;
#10572 = CARTESIAN_POINT ( 'NONE',  ( -3.000000000000000000, -10.45096189432314837, -21.10159698893440350 ) ) ;
#10573 = CARTESIAN_POINT ( 'NONE',  ( 0.000000000000000000, 31.52238457039599595, 27.75498641678753842 ) ) ;
#10575 = ORIENTED_EDGE ( 'NONE', *, *, #5566, .T. ) ;
#10574 = CARTESIAN_POINT ( 'NONE',  ( 0.000000000000000000, 0.000000000000000000, 0.000000000000000000 ) ) ;
#10576 = LINE ( 'NONE', #25004, #7469 ) ;
#10577 = AXIS2_PLACEMENT_3D ( 'NONE', #12608, #23861, #19680 ) ;
#10578 = CIRCLE ( 'NONE', #12966, 82.00000000000000000 ) ;
#10579 = ORIENTED_EDGE ( 'NONE', *, *, #25018, .F. ) ;
#10580 = DIRECTION ( 'NONE',  ( -1.000000000000000000, 0.000000000000000000, -0.000000000000000000 ) ) ;
#10581 = EDGE_LOOP ( 'NONE', ( #25840, #22171, #3812, #19930 ) ) ;
#10582 = ORIENTED_EDGE ( 'NONE', *, *, #36569, .T. ) ;
#10583 = CARTESIAN_POINT ( 'NONE',  ( 10.00000000000000000, 27.13269053701096922, 25.88420570971410228 ) ) ;
#10584 = DIRECTION ( 'NONE',  ( 1.000000000000000000, 0.000000000000000000, 0.000000000000000000 ) ) ;
#10585 = EDGE_LOOP ( 'NONE', ( #36497, #36781, #7710, #37356 ) ) ;
#10586 = FACE_OUTER_BOUND ( 'NONE', #15395, .T. ) ;
#10587 = CIRCLE ( 'NONE', #9768, 77.49899999999999523 ) ;
#10588 = CARTESIAN_POINT ( 'NONE',  ( -3.000000000000000000, -25.60904388321925396, 6.976881207771172377 ) ) ;
#10589 = FACE_OUTER_BOUND ( 'NONE', #11641, .T. ) ;
#10590 = ORIENTED_EDGE ( 'NONE', *, *, #22772, .T. ) ;
#10591 = VECTOR ( 'NONE', #37302, 1000.000000000000114 ) ;
#10592 = CARTESIAN_POINT ( 'NONE',  ( 11.99999999999999822, 0.000000000000000000, 0.000000000000000000 ) ) ;
#10593 = VECTOR ( 'NONE', #12987, 1000.000000000000114 ) ;
#10594 = LINE ( 'NONE', #15233, #40746 ) ;
#10595 = CARTESIAN_POINT ( 'NONE',  ( 5.000000000000000000, -16.65560815589439159, 38.55633173627004595 ) ) ;
#10596 = ORIENTED_EDGE ( 'NONE', *, *, #39300, .T. ) ;
#10597 = CIRCLE ( 'NONE', #47346, 37.49900000000000233 ) ;
#10598 = DIRECTION ( 'NONE',  ( 0.000000000000000000, 0.000000000000000000, 1.000000000000000000 ) ) ;
#10599 = FACE_OUTER_BOUND ( 'NONE', #25779, .T. ) ;
#10600 = CARTESIAN_POINT ( 'NONE',  ( 10.00000000000000000, 6.555932627142418312, 37.01155633439060466 ) ) ;
#10601 = CARTESIAN_POINT ( 'NONE',  ( 0.000000000000000000, -80.28980883073747066, -16.65972982745017461 ) ) ;
#10602 = AXIS2_PLACEMENT_3D ( 'NONE', #46233, #23969, #1451 ) ;
#10603 = FACE_OUTER_BOUND ( 'NONE', #19809, .T. ) ;
#10604 = FACE_OUTER_BOUND ( 'NONE', #31453, .T. ) ;
#10605 = CYLINDRICAL_SURFACE ( 'NONE', #34215, 31.99999999999999289 ) ;
#10606 = CYLINDRICAL_SURFACE ( 'NONE', #18655, 16.00000000000000000 ) ;
#10607 = ORIENTED_EDGE ( 'NONE', *, *, #39431, .F. ) ;
#10608 = CIRCLE ( 'NONE', #46561, 31.99999999999999289 ) ;
#10609 = EDGE_CURVE ( 'NONE', #25493, #19520, #3215, .T. ) ;
#10610 = DIRECTION ( 'NONE',  ( 0.000000000000000000, 0.000000000000000000, 1.000000000000000000 ) ) ;
#10611 = ORIENTED_EDGE ( 'NONE', *, *, #14550, .F. ) ;
#10612 = CARTESIAN_POINT ( 'NONE',  ( -26.53422223201112828, -120.6595836127786043, -2.500000000000000444 ) ) ;
#10613 = CARTESIAN_POINT ( 'NONE',  ( 11.99999999999999822, 0.000000000000000000, 0.000000000000000000 ) ) ;
#10614 = ORIENTED_EDGE ( 'NONE', *, *, #40289, .F. ) ;
#10615 = ADVANCED_FACE ( 'NONE', ( #28707 ), #18139, .T. ) ;
#10616 = DIRECTION ( 'NONE',  ( 0.000000000000000000, 0.000000000000000000, 1.000000000000000000 ) ) ;
#10617 = CIRCLE ( 'NONE', #8268, 16.00000000000000000 ) ;
#10618 = VERTEX_POINT ( 'NONE', #36279 ) ;
#10619 = ADVANCED_FACE ( 'NONE', ( #14007 ), #33081, .T. ) ;
#10620 = ORIENTED_EDGE ( 'NONE', *, *, #7782, .T. ) ;
#10621 = AXIS2_PLACEMENT_3D ( 'NONE', #41953, #12097, #8405 ) ;
#10622 = EDGE_CURVE ( 'NONE', #37774, #23927, #29748, .T. ) ;
#10623 = DIRECTION ( 'NONE',  ( -1.000000000000000000, 0.000000000000000000, -0.000000000000000000 ) ) ;
#10624 = VERTEX_POINT ( 'NONE', #35801 ) ;
#10625 = EDGE_CURVE ( 'NONE', #45724, #47714, #35229, .T. ) ;
#10626 = DIRECTION ( 'NONE',  ( 1.000000000000000000, -0.000000000000000000, 0.000000000000000000 ) ) ;
#10627 = CARTESIAN_POINT ( 'NONE',  ( -10.00000000000000000, 0.000000000000000000, 0.000000000000000000 ) ) ;
#10628 = ORIENTED_EDGE ( 'NONE', *, *, #34174, .F. ) ;
#10629 = LINE ( 'NONE', #17469, #42653 ) ;
#10630 = AXIS2_PLACEMENT_3D ( 'NONE', #46731, #38404, #12235 ) ;
#10631 = ADVANCED_FACE ( 'NONE', ( #33336 ), #41643, .F. ) ;
#10632 = AXIS2_PLACEMENT_3D ( 'NONE', #18939, #7930, #34123 ) ;
#10633 = EDGE_LOOP ( 'NONE', ( #6513, #1603, #27465, #14120, #33764, #29148 ) ) ;
#10634 = DIRECTION ( 'NONE',  ( 0.000000000000000000, 0.000000000000000000, 1.000000000000000000 ) ) ;
#10635 = PLANE ( 'NONE',  #25457 ) ;
#10636 = LINE ( 'NONE', #36799, #7134 ) ;
#10637 = AXIS2_PLACEMENT_3D ( 'NONE', #6436, #40932, #25987 ) ;
#10638 = EDGE_LOOP ( 'NONE', ( #29815, #24937, #12881, #37631 ) ) ;
#10639 = DIRECTION ( 'NONE',  ( -1.000000000000000000, 0.000000000000000000, -0.000000000000000000 ) ) ;
#10640 = EDGE_LOOP ( 'NONE', ( #19927, #42283, #12724, #5147 ) ) ;
#10641 = ORIENTED_EDGE ( 'NONE', *, *, #38509, .T. ) ;
#10642 = CARTESIAN_POINT ( 'NONE',  ( 10.00000000000000000, 0.000000000000000000, 0.000000000000000000 ) ) ;
#10643 = EDGE_CURVE ( 'NONE', #44958, #16459, #16487, .T. ) ;
#10644 = DIRECTION ( 'NONE',  ( -1.000000000000000000, -0.000000000000000000, -0.000000000000000000 ) ) ;
#10645 = LINE ( 'NONE', #2319, #8715 ) ;
#10646 = CARTESIAN_POINT ( 'NONE',  ( 0.000000000000000000, 0.000000000000000000, 42.00000000000001421 ) ) ;
#10647 = VERTEX_POINT ( 'NONE', #23040 ) ;
#10648 = PLANE ( 'NONE',  #14379 ) ;
#10649 = AXIS2_PLACEMENT_3D ( 'NONE', #23894, #1867, #28053 ) ;
#10650 = DIRECTION ( 'NONE',  ( -1.000000000000000000, 0.000000000000000000, -0.000000000000000000 ) ) ;
#10651 = CARTESIAN_POINT ( 'NONE',  ( 0.000000000000000000, 0.000000000000000000, 0.000000000000000000 ) ) ;
#10652 = DIRECTION ( 'NONE',  ( 0.000000000000000000, -9.787530781167598712E-16, -1.000000000000000000 ) ) ;
#10653 = CARTESIAN_POINT ( 'NONE',  ( 10.00000000000000000, -32.34446384429989507, 26.79245525562703278 ) ) ;
#10654 = CIRCLE ( 'NONE', #45842, 31.99999999999998934 ) ;
#10655 = ORIENTED_EDGE ( 'NONE', *, *, #42878, .F. ) ;
#10656 = CARTESIAN_POINT ( 'NONE',  ( -7.469491406282117829, 4.756046723998917258, -64.01812422950395387 ) ) ;
#10657 = AXIS2_PLACEMENT_3D ( 'NONE', #10829, #25739, #7151 ) ;
#10658 = CARTESIAN_POINT ( 'NONE',  ( 10.00000000000000000, -68.67312586194971402, -35.91791733033549860 ) ) ;
#10659 = LINE ( 'NONE', #21893, #7313 ) ;
#10660 = DIRECTION ( 'NONE',  ( -1.000000000000000000, -0.000000000000000000, -0.000000000000000000 ) ) ;
#10661 = EDGE_CURVE ( 'NONE', #43536, #31088, #3980, .T. ) ;
#10662 = CARTESIAN_POINT ( 'NONE',  ( 5.000000000000000000, -15.48615015657610705, 39.04073710021338428 ) ) ;
#10663 = DIRECTION ( 'NONE',  ( -1.000000000000000000, -0.000000000000000000, 0.000000000000000000 ) ) ;
#10664 = CLOSED_SHELL ( 'NONE', ( #3639, #16505, #7671, #37342, #47079, #28099, #13063, #35542, #40522, #1891, #38968, #8440, #14662, #10245, #24264, #8942, #44877, #930, #48411, #13644, #28031, #24379, #19276, #28682, #12239, #30004, #11855, #41631, #24698, #6909, #34096, #28182, #35766, #32687, #44140, #11711, #26201, #6150, #13362, #362, #4817, #17957, #39497, #46866, #22654, #25923, #18348, #5921, #14589, #13016, #1172, #18580, #36521, #16207, #16369, #13977, #39589, #8936, #14194, #20081, #34915, #373, #23477, #13212, #34351, #15852, #3017, #7533, #40566, #46763, #22936, #41581, #37287, #2692, #24900, #29310, #5421, #45470, #24779, #34559, #1434, #31459, #5625, #16046, #1566, #23857, #33933, #14806, #8604, #5190, #215, #15135, #18046, #35477, #2524, #46427, #28489, #4591, #42681, #34423, #47242, #43254, #17797, #23418, #26868, #10363, #21567, #13440, #42498, #15728, #13028, #1896, #39745, #6038, #14672, #2111, #16034, #8391, #19501, #36011, #43058, #4283, #47920, #6705, #16963, #19990, #13538, #33106, #34436, #20333, #32974, #20600, #29304, #5752, #21387, #39817, #35114, #19643, #12564, #14494, #39021, #42502, #10936, #7775, #21505, #18409, #18047, #25856, #8124, #39265, #26685, #223, #31641, #15419, #7481, #10108, #37980, #19716, #39683, #8282, #21442, #3650, #31401, #2568, #33425, #4813, #45443, #19431, #42738, #25762, #33641, #34246, #42384, #18060, #39844, #5417, #28163, #11656, #44929, #2550, #39024, #29341, #29667, #37513, #46194, #16921, #38373, #15591, #15488, #13776, #48030, #46773, #3295, #41772, #27533, #44517, #6090, #28586, #573, #30587, #24694, #5582, #37809, #44107, #17085, #45836, #13695, #42525, #34250, #26742, #33758, #32275, #44861, #15363, #12657, #11081, #35310, #29822, #15151, #28030, #6582, #47952, #345, #23504, #38204, #40591, #41404, #25129, #14561, #5741, #45318, #32571, #20024, #39332, #492, #11101, #13788, #46302, #17274, #43241, #3877, #2620, #37736, #37467, #745, #38191, #16634, #6637, #12949, #46811, #37801, #43760, #26801, #31474, #709, #9781, #6514, #20185, #32173, #29370, #46986, #4423, #27991, #40755, #31020, #5864, #46923, #867, #36841, #40693, #43848, #9722, #1222, #9068, #30839, #24811, #21895, #24057, #33740, #41724, #37691, #26675, #22876, #2269, #21872, #24490, #40619, #6263, #41910, #15383, #29035, #16562, #7843, #11129, #10494, #43475, #31398, #16622, #14268, #36941, #30111, #10615, #161, #5322, #33858, #33392, #32560, #32220, #44931, #43918, #7986, #13018, #32193, #11348, #14153, #42043, #5086, #28451, #611, #19649, #32856, #14545, #32587, #35340, #11156, #32095, #15580, #121, #44868, #28455, #1401, #20428, #19481, #39749, #36136, #47520, #24560, #37088, #11303, #16313, #26648, #36403, #18784, #40291, #46489, #25425, #43128, #39474, #25582, #4277, #34983, #14769, #4045, #12847, #39686, #31296, #41338, #4860, #2413, #15493, #23236, #33954, #12391, #34679, #445, #41612, #8596, #20261, #2716, #25635, #9733, #2071, #1388, #11095, #28334, #47359, #36662, #4485, #48347, #42684, #2698, #7759, #1683, #22702, #31570, #26110, #11991, #38259, #14114, #40609, #40082, #45574, #42834, #33484, #29876, #20002, #40007, #39859, #37083, #40022, #42568, #29840, #32652, #43107 ) ) ;
#10665 = ORIENTED_EDGE ( 'NONE', *, *, #45855, .F. ) ;
#10666 = DIRECTION ( 'NONE',  ( 1.000000000000000000, -0.000000000000000000, -0.000000000000000000 ) ) ;
#10667 = ADVANCED_FACE ( 'NONE', ( #22062 ), #33569, .F. ) ;
#10668 = CIRCLE ( 'NONE', #42704, 31.99999999999998934 ) ;
#10669 = CIRCLE ( 'NONE', #29430, 82.00000000000000000 ) ;
#10670 = ADVANCED_FACE ( 'NONE', ( #37977 ), #48262, .T. ) ;
#10671 = DIRECTION ( 'NONE',  ( 0.000000000000000000, 0.000000000000000000, 1.000000000000000000 ) ) ;
#10672 = ORIENTED_EDGE ( 'NONE', *, *, #32695, .T. ) ;
#10673 = AXIS2_PLACEMENT_3D ( 'NONE', #27395, #42571, #13422 ) ;
#10674 = ORIENTED_EDGE ( 'NONE', *, *, #32760, .F. ) ;
#10675 = DIRECTION ( 'NONE',  ( 0.000000000000000000, 0.9876883405951383255, -0.1564344650402277048 ) ) ;
#10676 = ADVANCED_FACE ( 'NONE', ( #531 ), #14739, .T. ) ;
#10677 = ORIENTED_EDGE ( 'NONE', *, *, #47082, .F. ) ;
#10678 = EDGE_CURVE ( 'NONE', #20089, #11046, #29897, .T. ) ;
#10679 = EDGE_CURVE ( 'NONE', #26682, #28743, #3714, .T. ) ;
#10680 = ORIENTED_EDGE ( 'NONE', *, *, #16686, .T. ) ;
#10681 = CIRCLE ( 'NONE', #38044, 31.99999999999998579 ) ;
#10682 = DIRECTION ( 'NONE',  ( 0.000000000000000000, -0.4067366430757881068, -0.9135454576426063067 ) ) ;
#10683 = CARTESIAN_POINT ( 'NONE',  ( 11.99999999999999822, -33.71516098798685590, -74.74816331893465815 ) ) ;
#10685 = ORIENTED_EDGE ( 'NONE', *, *, #27036, .F. ) ;
#10684 = CARTESIAN_POINT ( 'NONE',  ( 11.99999999999999822, 30.41916302227114599, 71.27951684758035356 ) ) ;
#10686 = ORIENTED_EDGE ( 'NONE', *, *, #10976, .F. ) ;
#10687 = AXIS2_PLACEMENT_3D ( 'NONE', #21772, #10525, #14922 ) ;
#10688 = DIRECTION ( 'NONE',  ( 0.000000000000000000, 0.000000000000000000, 1.000000000000000000 ) ) ;
#10689 = ORIENTED_EDGE ( 'NONE', *, *, #14886, .T. ) ;
#10690 = EDGE_LOOP ( 'NONE', ( #4317, #47839, #24053, #28957 ) ) ;
#10691 = ORIENTED_EDGE ( 'NONE', *, *, #30296, .F. ) ;
#10692 = CARTESIAN_POINT ( 'NONE',  ( 0.000000000000000000, -41.81611651403859042, -3.925862922256606602 ) ) ;
#10693 = EDGE_CURVE ( 'NONE', #8092, #8291, #47690, .T. ) ;
#10694 = FACE_OUTER_BOUND ( 'NONE', #3024, .T. ) ;
#10695 = CARTESIAN_POINT ( 'NONE',  ( 10.00000000000000000, 81.34940948281335693, 10.30890764327412690 ) ) ;
#10696 = ORIENTED_EDGE ( 'NONE', *, *, #772, .F. ) ;
#10697 = AXIS2_PLACEMENT_3D ( 'NONE', #4401, #34228, #42075 ) ;
#10698 = ORIENTED_EDGE ( 'NONE', *, *, #47425, .T. ) ;
#10699 = CARTESIAN_POINT ( 'NONE',  ( 0.000000000000000000, 0.000000000000000000, 0.000000000000000000 ) ) ;
#10700 = VERTEX_POINT ( 'NONE', #26476 ) ;
#10701 = DIRECTION ( 'NONE',  ( -0.9580045777625459946, -0.2867529058022011412, 0.000000000000000000 ) ) ;
#10702 = DIRECTION ( 'NONE',  ( -1.000000000000000000, 0.000000000000000000, -0.000000000000000000 ) ) ;
#10703 = PLANE ( 'NONE',  #23701 ) ;
#10704 = EDGE_LOOP ( 'NONE', ( #37108, #38646, #3770, #28414 ) ) ;
#10705 = DIRECTION ( 'NONE',  ( 0.000000000000000000, 0.000000000000000000, 1.000000000000000000 ) ) ;
#10706 = CARTESIAN_POINT ( 'NONE',  ( -12.50000000000000000, -132.5000000000000000, 40.00000000000000000 ) ) ;
#10707 = PLANE ( 'NONE',  #22519 ) ;
#10708 = LINE ( 'NONE', #13650, #4013 ) ;
#10709 = AXIS2_PLACEMENT_3D ( 'NONE', #5786, #9437, #16318 ) ;
#10710 = CARTESIAN_POINT ( 'NONE',  ( 5.250000000000000000, -13.95926121303099343, 0.000000000000000000 ) ) ;
#10711 = ORIENTED_EDGE ( 'NONE', *, *, #31372, .T. ) ;
#10712 = DIRECTION ( 'NONE',  ( -1.000000000000000000, 0.000000000000000000, 0.000000000000000000 ) ) ;
#10713 = DIRECTION ( 'NONE',  ( -1.000000000000000000, -0.000000000000000000, -0.000000000000000000 ) ) ;
#10714 = DIRECTION ( 'NONE',  ( 0.000000000000000000, 0.000000000000000000, 1.000000000000000000 ) ) ;
#10715 = CARTESIAN_POINT ( 'NONE',  ( 0.000000000000000000, -37.58145647212455032, 0.6853352020789044152 ) ) ;
#10716 = CARTESIAN_POINT ( 'NONE',  ( 11.99999999999999822, 0.8261519478441983200, -77.49459641780885022 ) ) ;
#10717 = DIRECTION ( 'NONE',  ( 0.000000000000000000, 0.000000000000000000, 1.000000000000000000 ) ) ;
#10718 = VECTOR ( 'NONE', #14298, 1000.000000000000000 ) ;
#10719 = EDGE_CURVE ( 'NONE', #46082, #22693, #45369, .T. ) ;
#10720 = DIRECTION ( 'NONE',  ( 1.000000000000000000, -0.000000000000000000, 0.000000000000000000 ) ) ;
#10721 = CARTESIAN_POINT ( 'NONE',  ( -3.000000000000000000, 23.50000000000000000, 1.499999999999997780 ) ) ;
#10722 = APPLICATION_CONTEXT ( 'automotive_design' ) ;
#10723 = ADVANCED_FACE ( 'NONE', ( #27, #26717 ), #18639, .T. ) ;
#10724 = AXIS2_PLACEMENT_3D ( 'NONE', #41593, #31317, #22987 ) ;
#10725 = DIRECTION ( 'NONE',  ( 0.000000000000000000, 0.8526401643540936215, -0.5224985647159469115 ) ) ;
#10726 = FILL_AREA_STYLE_COLOUR ( '', #9222 ) ;
#10727 = ADVANCED_FACE ( 'NONE', ( #34283 ), #754, .T. ) ;
#10728 = DIRECTION ( 'NONE',  ( -1.000000000000000000, 0.000000000000000000, 0.000000000000000000 ) ) ;
#10729 = ORIENTED_EDGE ( 'NONE', *, *, #27208, .T. ) ;
#10730 = ORIENTED_EDGE ( 'NONE', *, *, #18885, .F. ) ;
#10731 = ORIENTED_EDGE ( 'NONE', *, *, #721, .T. ) ;
#10732 = VECTOR ( 'NONE', #42690, 1000.000000000000000 ) ;
#10733 = EDGE_LOOP ( 'NONE', ( #11768, #31209, #15853, #3985 ) ) ;
#10734 = CARTESIAN_POINT ( 'NONE',  ( -10.00000000000000000, 0.000000000000000000, 0.000000000000000000 ) ) ;
#10735 = DIRECTION ( 'NONE',  ( 0.000000000000000000, 8.881784197001252323E-16, 1.000000000000000000 ) ) ;
#10736 = ORIENTED_EDGE ( 'NONE', *, *, #27272, .T. ) ;
#10737 = EDGE_CURVE ( 'NONE', #37330, #30853, #44829, .T. ) ;
#10738 = EDGE_CURVE ( 'NONE', #10741, #41750, #27464, .T. ) ;
#10739 = CIRCLE ( 'NONE', #31863, 82.00000000000000000 ) ;
#10740 = DIRECTION ( 'NONE',  ( 0.000000000000000000, 0.000000000000000000, 1.000000000000000000 ) ) ;
#10741 = VERTEX_POINT ( 'NONE', #36991 ) ;
#10742 = ORIENTED_EDGE ( 'NONE', *, *, #36190, .T. ) ;
#10743 = EDGE_CURVE ( 'NONE', #7609, #4936, #22760, .T. ) ;
#10744 = VECTOR ( 'NONE', #10871, 1000.000000000000000 ) ;
#10745 = FACE_OUTER_BOUND ( 'NONE', #33530, .T. ) ;
#10746 = ORIENTED_EDGE ( 'NONE', *, *, #44968, .F. ) ;
#10747 = DIRECTION ( 'NONE',  ( -1.000000000000000000, 0.000000000000000000, 0.000000000000000000 ) ) ;
#10748 = ORIENTED_EDGE ( 'NONE', *, *, #3021, .T. ) ;
#10749 = DIRECTION ( 'NONE',  ( -1.000000000000000000, -0.000000000000000000, -0.000000000000000000 ) ) ;
#10750 = AXIS2_PLACEMENT_3D ( 'NONE', #884, #15831, #30763 ) ;
#10751 = DIRECTION ( 'NONE',  ( -1.000000000000000000, 0.000000000000000000, 0.000000000000000000 ) ) ;
#10752 = DIRECTION ( 'NONE',  ( 0.000000000000000000, 0.5877852522924742473, -0.8090169943749465631 ) ) ;
#10753 = ORIENTED_EDGE ( 'NONE', *, *, #29902, .F. ) ;
#10754 = ORIENTED_EDGE ( 'NONE', *, *, #38296, .T. ) ;
#10755 = DIRECTION ( 'NONE',  ( -1.000000000000000000, -0.000000000000000000, 0.000000000000000000 ) ) ;
#10756 = DIRECTION ( 'NONE',  ( 0.9966891607226785466, 0.08130631524009969413, 0.000000000000000000 ) ) ;
#10757 = CIRCLE ( 'NONE', #27963, 31.99999999999999645 ) ;
#10758 = ORIENTED_EDGE ( 'NONE', *, *, #30985, .F. ) ;
#10759 = ORIENTED_EDGE ( 'NONE', *, *, #47774, .T. ) ;
#10760 = FACE_OUTER_BOUND ( 'NONE', #35664, .T. ) ;
#10761 = DIRECTION ( 'NONE',  ( 0.000000000000000000, 0.5877852522924685852, 0.8090169943749508930 ) ) ;
#10762 = EDGE_LOOP ( 'NONE', ( #20425, #26920, #12967, #47423 ) ) ;
#10763 = ORIENTED_EDGE ( 'NONE', *, *, #34708, .T. ) ;
#10764 = DIRECTION ( 'NONE',  ( -1.000000000000000000, 0.000000000000000000, 0.000000000000000000 ) ) ;
#10765 = DIRECTION ( 'NONE',  ( -1.000000000000000000, -0.000000000000000000, 0.000000000000000000 ) ) ;
#10766 = CARTESIAN_POINT ( 'NONE',  ( -6.509281303079589520, -14.89695620656361008, -1.199999999999999956 ) ) ;
#10767 = FACE_OUTER_BOUND ( 'NONE', #27469, .T. ) ;
#10768 = CARTESIAN_POINT ( 'NONE',  ( -3.000000000000000000, -14.54903810567645195, -22.19967320028775504 ) ) ;
#10769 = AXIS2_PLACEMENT_3D ( 'NONE', #28408, #35758, #47017 ) ;
#10770 = LINE ( 'NONE', #44053, #3683 ) ;
#10771 = DIRECTION ( 'NONE',  ( 0.000000000000000000, 0.000000000000000000, 1.000000000000000000 ) ) ;
#10772 = CARTESIAN_POINT ( 'NONE',  ( 5.000000000000002665, 44.99326035066052043, 68.55367621811159040 ) ) ;
#10773 = VERTEX_POINT ( 'NONE', #22562 ) ;
#10774 = EDGE_CURVE ( 'NONE', #11405, #39311, #1672, .T. ) ;
#10775 = DIRECTION ( 'NONE',  ( -1.000000000000000000, 0.000000000000000000, 0.000000000000000000 ) ) ;
#10776 = LINE ( 'NONE', #25681, #10497 ) ;
#10777 = FILL_AREA_STYLE_COLOUR ( '', #14784 ) ;
#10778 = CYLINDRICAL_SURFACE ( 'NONE', #13119, 11.59999999999999964 ) ;
#10779 = EDGE_CURVE ( 'NONE', #46892, #23962, #18835, .T. ) ;
#10780 = ORIENTED_EDGE ( 'NONE', *, *, #16020, .F. ) ;
#10781 = ORIENTED_EDGE ( 'NONE', *, *, #15216, .T. ) ;
#10782 = VERTEX_POINT ( 'NONE', #1497 ) ;
#10783 = AXIS2_PLACEMENT_3D ( 'NONE', #7856, #11778, #26710 ) ;
#10784 = EDGE_CURVE ( 'NONE', #41873, #13148, #46982, .T. ) ;
#10785 = CARTESIAN_POINT ( 'NONE',  ( -9.332068499558245023, 6.890028847512374988, 52.00000000000002132 ) ) ;
#10786 = CIRCLE ( 'NONE', #42829, 16.00000000000000000 ) ;
#10787 = LINE ( 'NONE', #29388, #19057 ) ;
#10788 = ORIENTED_EDGE ( 'NONE', *, *, #28069, .F. ) ;
#10789 = EDGE_CURVE ( 'NONE', #41629, #15072, #1258, .T. ) ;
#10790 = EDGE_CURVE ( 'NONE', #23962, #3340, #30557, .T. ) ;
#10791 = FACE_OUTER_BOUND ( 'NONE', #8667, .T. ) ;
#10792 = VERTEX_POINT ( 'NONE', #9311 ) ;
#10793 = CARTESIAN_POINT ( 'NONE',  ( 10.00000000000000000, 0.000000000000000000, 0.000000000000000000 ) ) ;
#10794 = VERTEX_POINT ( 'NONE', #16420 ) ;
#10795 = ORIENTED_EDGE ( 'NONE', *, *, #19163, .F. ) ;
#10796 = ORIENTED_EDGE ( 'NONE', *, *, #36365, .F. ) ;
#10797 = DIRECTION ( 'NONE',  ( -1.000000000000000000, 0.000000000000000000, 0.000000000000000000 ) ) ;
#10798 = AXIS2_PLACEMENT_3D ( 'NONE', #26099, #11434, #15090 ) ;
#10799 = EDGE_CURVE ( 'NONE', #47158, #44507, #12282, .T. ) ;
#10800 = LINE ( 'NONE', #14473, #31336 ) ;
#10801 = ORIENTED_EDGE ( 'NONE', *, *, #29941, .F. ) ;
#10802 = ORIENTED_EDGE ( 'NONE', *, *, #6572, .T. ) ;
#10803 = LINE ( 'NONE', #25708, #46252 ) ;
#10804 = ORIENTED_EDGE ( 'NONE', *, *, #26016, .T. ) ;
#10805 = CYLINDRICAL_SURFACE ( 'NONE', #19933, 31.99999999999998579 ) ;
#10806 = DIRECTION ( 'NONE',  ( -1.000000000000000000, -0.000000000000000000, -0.000000000000000000 ) ) ;
#10807 = ORIENTED_EDGE ( 'NONE', *, *, #12401, .T. ) ;
#10808 = CARTESIAN_POINT ( 'NONE',  ( -10.00000000000000000, 0.000000000000000000, 0.000000000000000000 ) ) ;
#10809 = DIRECTION ( 'NONE',  ( 0.000000000000000000, 0.9945218953682742891, 0.1045284632676436315 ) ) ;
#10810 = ADVANCED_FACE ( 'NONE', ( #45544 ), #30884, .F. ) ;
#10812 = ORIENTED_EDGE ( 'NONE', *, *, #3866, .F. ) ;
#10811 = DIRECTION ( 'NONE',  ( 0.000000000000000000, -0.5877852522924802425, 0.8090169943749422332 ) ) ;
#10813 = CARTESIAN_POINT ( 'NONE',  ( 4.999999999999999112, 2.663952781846732343, -41.91543099594814947 ) ) ;
#10814 = ORIENTED_EDGE ( 'NONE', *, *, #39805, .F. ) ;
#10815 = DIRECTION ( 'NONE',  ( 1.000000000000000000, 0.000000000000000000, 0.000000000000000000 ) ) ;
#10816 = ORIENTED_EDGE ( 'NONE', *, *, #24427, .T. ) ;
#10817 = ORIENTED_EDGE ( 'NONE', *, *, #4161, .F. ) ;
#10818 = DIRECTION ( 'NONE',  ( 0.000000000000000000, 2.312964634635746211E-15, -1.000000000000000000 ) ) ;
#10819 = DIRECTION ( 'NONE',  ( -1.000000000000000000, -0.000000000000000000, -0.000000000000000000 ) ) ;
#10820 = CIRCLE ( 'NONE', #37396, 16.00000000000000000 ) ;
#10821 = DIRECTION ( 'NONE',  ( 0.000000000000000000, 0.000000000000000000, 1.000000000000000000 ) ) ;
#10822 = ORIENTED_EDGE ( 'NONE', *, *, #47579, .F. ) ;
#10823 = DIRECTION ( 'NONE',  ( 0.000000000000000000, 0.000000000000000000, 1.000000000000000000 ) ) ;
#10824 = CARTESIAN_POINT ( 'NONE',  ( 11.99999999999999822, 76.66974797899837313, 11.30684508768366747 ) ) ;
#10825 = ORIENTED_EDGE ( 'NONE', *, *, #34124, .F. ) ;
#10826 = AXIS2_PLACEMENT_3D ( 'NONE', #28747, #25541, #47808 ) ;
#10827 = DIRECTION ( 'NONE',  ( -0.9038112904824853189, 0.4279312458752977943, 0.000000000000000000 ) ) ;
#10828 = DIRECTION ( 'NONE',  ( 0.000000000000000000, 0.6691306063588672304, -0.7431448254773862505 ) ) ;
#10829 = CARTESIAN_POINT ( 'NONE',  ( 10.00000000000000000, -41.76937507738831812, 62.50329211542423025 ) ) ;
#10830 = ORIENTED_EDGE ( 'NONE', *, *, #33225, .F. ) ;
#10831 = CYLINDRICAL_SURFACE ( 'NONE', #16098, 32.00000000000000000 ) ;
#10832 = CARTESIAN_POINT ( 'NONE',  ( 10.00000000000000000, -2.543863470248951320, 81.96053171279901051 ) ) ;
#10833 = CARTESIAN_POINT ( 'NONE',  ( 0.000000000000000000, 72.35160999960844208, -20.41045688087747223 ) ) ;
#10834 = DIRECTION ( 'NONE',  ( -1.000000000000000000, 0.000000000000000000, 0.000000000000000000 ) ) ;
#10835 = ADVANCED_FACE ( 'NONE', ( #24242 ), #5648, .T. ) ;
#10836 = EDGE_CURVE ( 'NONE', #9989, #6694, #5406, .T. ) ;
#10837 = DIRECTION ( 'NONE',  ( 1.000000000000000000, -0.000000000000000000, 0.000000000000000000 ) ) ;
#10838 = DIRECTION ( 'NONE',  ( 0.000000000000000000, 0.000000000000000000, 1.000000000000000000 ) ) ;
#10839 = AXIS2_PLACEMENT_3D ( 'NONE', #37022, #29683, #22089 ) ;
#10840 = DIRECTION ( 'NONE',  ( -1.000000000000000000, 0.000000000000000000, 0.000000000000000000 ) ) ;
#10841 = DIRECTION ( 'NONE',  ( 1.000000000000000000, 0.000000000000000000, 0.000000000000000000 ) ) ;
#10842 = EDGE_CURVE ( 'NONE', #23745, #2128, #38390, .T. ) ;
#10843 = AXIS2_PLACEMENT_3D ( 'NONE', #11079, #43882, #25262 ) ;
#10844 = EDGE_LOOP ( 'NONE', ( #35824, #34921, #22420, #1538 ) ) ;
#10845 = DIRECTION ( 'NONE',  ( -1.000000000000000000, 0.000000000000000000, -0.000000000000000000 ) ) ;
#10846 = ORIENTED_EDGE ( 'NONE', *, *, #39456, .T. ) ;
#10847 = EDGE_CURVE ( 'NONE', #40486, #25055, #2415, .T. ) ;
#10848 = CARTESIAN_POINT ( 'NONE',  ( 15.00000000000000000, 22.07842321921492612, 8.187992925817123790 ) ) ;
#10849 = CARTESIAN_POINT ( 'NONE',  ( 4.574237413256307008E-15, 3.992474787516313146E-15, 42.00000000000001421 ) ) ;
#10850 = DIRECTION ( 'NONE',  ( -1.000000000000000000, 0.000000000000000000, -0.000000000000000000 ) ) ;
#10851 = ORIENTED_EDGE ( 'NONE', *, *, #22397, .T. ) ;
#10852 = CARTESIAN_POINT ( 'NONE',  ( -3.000000000000000000, -22.67460108101774807, -6.353146135318215038 ) ) ;
#10853 = CIRCLE ( 'NONE', #10076, 77.49899999999999523 ) ;
#10854 = EDGE_LOOP ( 'NONE', ( #983, #14089, #6999, #13904 ) ) ;
#10855 = VECTOR ( 'NONE', #44472, 1000.000000000000000 ) ;
#10856 = VECTOR ( 'NONE', #9648, 1000.000000000000114 ) ;
#10857 = EDGE_CURVE ( 'NONE', #46024, #26165, #20411, .T. ) ;
#10858 = DIRECTION ( 'NONE',  ( -1.000000000000000000, -0.000000000000000000, -0.000000000000000000 ) ) ;
#10859 = LINE ( 'NONE', #566, #22643 ) ;
#10860 = CARTESIAN_POINT ( 'NONE',  ( 0.000000000000000000, 0.000000000000000000, -105.0000000000000000 ) ) ;
#10861 = ORIENTED_EDGE ( 'NONE', *, *, #4440, .T. ) ;
#10862 = LINE ( 'NONE', #40972, #16832 ) ;
#10863 = AXIS2_PLACEMENT_3D ( 'NONE', #12720, #20290, #28365 ) ;
#10864 = ORIENTED_EDGE ( 'NONE', *, *, #927, .F. ) ;
#10865 = DIRECTION ( 'NONE',  ( -0.000000000000000000, -0.000000000000000000, -1.000000000000000000 ) ) ;
#10866 = CARTESIAN_POINT ( 'NONE',  ( 11.99999999999999822, 74.65374052328648702, 8.840884882375350529 ) ) ;
#10867 = DIRECTION ( 'NONE',  ( 0.000000000000000000, 0.000000000000000000, 1.000000000000000000 ) ) ;
#10868 = EDGE_CURVE ( 'NONE', #6289, #11748, #42303, .T. ) ;
#10869 = DIRECTION ( 'NONE',  ( -1.000000000000000000, 0.000000000000000000, 0.000000000000000000 ) ) ;
#10870 = ORIENTED_EDGE ( 'NONE', *, *, #10495, .F. ) ;
#10871 = DIRECTION ( 'NONE',  ( -0.000000000000000000, 0.9781476007338069101, -0.2079116908177532363 ) ) ;
#10872 = ORIENTED_EDGE ( 'NONE', *, *, #47668, .T. ) ;
#10873 = VERTEX_POINT ( 'NONE', #1735 ) ;
#10874 = CARTESIAN_POINT ( 'NONE',  ( 0.000000000000000000, -44.99326035066101781, 68.55367621811127776 ) ) ;
#10875 = DIRECTION ( 'NONE',  ( 0.000000000000000000, 0.000000000000000000, 1.000000000000000000 ) ) ;
#10876 = DIRECTION ( 'NONE',  ( 0.000000000000000000, 1.000000000000000000, 3.491481338843133750E-15 ) ) ;
#10877 = CYLINDRICAL_SURFACE ( 'NONE', #5614, 31.99999999999997868 ) ;
#10878 = VERTEX_POINT ( 'NONE', #16662 ) ;
#10879 = CYLINDRICAL_SURFACE ( 'NONE', #23725, 31.99999999999998579 ) ;
#10880 = DIRECTION ( 'NONE',  ( 0.000000000000000000, 0.000000000000000000, 1.000000000000000000 ) ) ;
#10881 = CARTESIAN_POINT ( 'NONE',  ( 6.719258119307966126, -15.35072898742050462, -1.199999999999999956 ) ) ;
#10882 = DIRECTION ( 'NONE',  ( -0.7585478161175716050, -0.6516173805718067369, 0.000000000000000000 ) ) ;
#10883 = CARTESIAN_POINT ( 'NONE',  ( 11.99999999999999822, 14.66109333815460225, 73.73191006444577056 ) ) ;
#10884 = ORIENTED_EDGE ( 'NONE', *, *, #29284, .T. ) ;
#10885 = VECTOR ( 'NONE', #46974, 1000.000000000000227 ) ;
#10886 = DIRECTION ( 'NONE',  ( -0.000000000000000000, 0.9781476007338042455, -0.2079116908177663092 ) ) ;
#10887 = CARTESIAN_POINT ( 'NONE',  ( 10.00000000000000000, -70.52718814184240159, -26.02418014898383802 ) ) ;
#10888 = DIRECTION ( 'NONE',  ( -1.000000000000000000, -0.000000000000000000, 0.000000000000000000 ) ) ;
#10889 = EDGE_CURVE ( 'NONE', #35339, #35674, #8822, .T. ) ;
#10890 = VECTOR ( 'NONE', #42039, 1000.000000000000000 ) ;
#10891 = DIRECTION ( 'NONE',  ( 0.000000000000000000, 0.000000000000000000, 1.000000000000000000 ) ) ;
#10892 = CARTESIAN_POINT ( 'NONE',  ( -12.40464318976452596, 10.41032311384371489, 42.00000000000001421 ) ) ;
#10893 = EDGE_CURVE ( 'NONE', #13081, #11259, #38217, .T. ) ;
#10894 = DIRECTION ( 'NONE',  ( -1.000000000000000000, -0.000000000000000000, -0.000000000000000000 ) ) ;
#10895 = FACE_OUTER_BOUND ( 'NONE', #19159, .T. ) ;
#10896 = CARTESIAN_POINT ( 'NONE',  ( 10.00000000000000000, -27.75498641678764855, 31.52238457039589647 ) ) ;
#10897 = VECTOR ( 'NONE', #23088, 1000.000000000000000 ) ;
#10898 = CARTESIAN_POINT ( 'NONE',  ( 17.82587367876289974, -104.6869915565625320, -2.500000000000000000 ) ) ;
#10899 = EDGE_CURVE ( 'NONE', #47426, #17270, #21186, .T. ) ;
#10900 = CARTESIAN_POINT ( 'NONE',  ( 11.99999999999999822, 24.73286445877808148, -73.44644590900034586 ) ) ;
#10901 = ADVANCED_FACE ( 'NONE', ( #9082 ), #4680, .F. ) ;
#10902 = PRODUCT_DEFINITION_SHAPE ( 'NONE', 'NONE',  #48467 ) ;
#10903 = LINE ( 'NONE', #114, #9551 ) ;
#10904 = EDGE_LOOP ( 'NONE', ( #8343, #33504, #18373, #15885 ) ) ;
#10905 = EDGE_LOOP ( 'NONE', ( #43125, #40318, #3281, #47524 ) ) ;
#10906 = ADVANCED_FACE ( 'NONE', ( #8580 ), #23513, .T. ) ;
#10907 = DIRECTION ( 'NONE',  ( -1.000000000000000000, -0.000000000000000000, 0.000000000000000000 ) ) ;
#10908 = ORIENTED_EDGE ( 'NONE', *, *, #45855, .T. ) ;
#10909 = AXIS2_PLACEMENT_3D ( 'NONE', #33572, #29659, #7147 ) ;
#10910 = DIRECTION ( 'NONE',  ( 0.000000000000000000, 0.9510565162951503115, -0.3090169943749573878 ) ) ;
#10911 = VECTOR ( 'NONE', #1901, 1000.000000000000000 ) ;
#10912 = DIRECTION ( 'NONE',  ( 1.000000000000000000, 0.000000000000000000, 0.000000000000000000 ) ) ;
#10913 = DIRECTION ( 'NONE',  ( -1.000000000000000000, -0.000000000000000000, -0.000000000000000000 ) ) ;
#10914 = CIRCLE ( 'NONE', #47659, 16.00000000000000000 ) ;
#10915 = ORIENTED_EDGE ( 'NONE', *, *, #39126, .F. ) ;
#10916 = DIRECTION ( 'NONE',  ( -1.000000000000000000, -0.000000000000000000, -0.000000000000000000 ) ) ;
#10917 = ORIENTED_EDGE ( 'NONE', *, *, #46973, .F. ) ;
#10918 = VERTEX_POINT ( 'NONE', #36219 ) ;
#10919 = ORIENTED_EDGE ( 'NONE', *, *, #44262, .F. ) ;
#10920 = ORIENTED_EDGE ( 'NONE', *, *, #5021, .T. ) ;
#10921 = CYLINDRICAL_SURFACE ( 'NONE', #13136, 12.50000000000000000 ) ;
#10922 = CARTESIAN_POINT ( 'NONE',  ( 11.99999999999999822, -59.46389618801929089, -49.70050353004953081 ) ) ;
#10923 = FACE_OUTER_BOUND ( 'NONE', #22650, .T. ) ;
#10924 = EDGE_CURVE ( 'NONE', #4123, #37702, #6608, .T. ) ;
#10925 = EDGE_LOOP ( 'NONE', ( #39136, #8983, #30712, #25678 ) ) ;
#10926 = ORIENTED_EDGE ( 'NONE', *, *, #23324, .T. ) ;
#10927 = VECTOR ( 'NONE', #12089, 1000.000000000000000 ) ;
#10928 = DIRECTION ( 'NONE',  ( 1.000000000000000000, 0.000000000000000000, 0.000000000000000000 ) ) ;
#10929 = ORIENTED_EDGE ( 'NONE', *, *, #31578, .F. ) ;
#10930 = DIRECTION ( 'NONE',  ( -1.000000000000000000, -0.000000000000000000, 0.000000000000000000 ) ) ;
#10931 = ADVANCED_FACE ( 'NONE', ( #6133 ), #14189, .T. ) ;
#10932 = CARTESIAN_POINT ( 'NONE',  ( 5.000000000000002665, 81.50828551894227303, 8.966570791700979370 ) ) ;
#10933 = CARTESIAN_POINT ( 'NONE',  ( 15.00000000000000000, 23.49999999999999645, 1.499999999999995337 ) ) ;
#10934 = CARTESIAN_POINT ( 'NONE',  ( 0.000000000000000000, 0.000000000000000000, 0.000000000000000000 ) ) ;
#10935 = DIRECTION ( 'NONE',  ( -0.9227826878668540234, -0.3853207896976547642, 0.000000000000000000 ) ) ;
#10936 = ADVANCED_FACE ( 'NONE', ( #32778 ), #10034, .T. ) ;
#10937 = DIRECTION ( 'NONE',  ( -1.000000000000000000, 0.000000000000000000, 0.000000000000000000 ) ) ;
#10938 = CYLINDRICAL_SURFACE ( 'NONE', #6350, 30.50000000000000000 ) ;
#10939 = CARTESIAN_POINT ( 'NONE',  ( 12.00000000000000000, 9.615535125378768200, -24.73947219025917121 ) ) ;
#10940 = DIRECTION ( 'NONE',  ( -0.000000000000000000, 0.8090169943749503378, 0.5877852522924690293 ) ) ;
#10941 = ORIENTED_EDGE ( 'NONE', *, *, #37125, .F. ) ;
#10942 = CARTESIAN_POINT ( 'NONE',  ( 0.6180191030787338669, -93.50720753887522108, -2.500000000000000000 ) ) ;
#10943 = LINE ( 'NONE', #31015, #1929 ) ;
#10944 = FACE_OUTER_BOUND ( 'NONE', #30301, .T. ) ;
#10945 = LINE ( 'NONE', #44477, #18238 ) ;
#10946 = ADVANCED_FACE ( 'NONE', ( #40391 ), #17615, .T. ) ;
#10947 = EDGE_CURVE ( 'NONE', #12242, #44442, #14943, .T. ) ;
#10948 = ADVANCED_FACE ( 'NONE', ( #32085 ), #13469, .T. ) ;
#10949 = CARTESIAN_POINT ( 'NONE',  ( 0.000000000000000000, 0.000000000000000000, 0.000000000000000000 ) ) ;
#10950 = LINE ( 'NONE', #18536, #27174 ) ;
#10951 = ORIENTED_EDGE ( 'NONE', *, *, #13649, .T. ) ;
#10952 = DIRECTION ( 'NONE',  ( -0.1045284632676570929, 0.9945218953682730678, 0.000000000000000000 ) ) ;
#10953 = DIRECTION ( 'NONE',  ( -0.7273375899149812085, 0.6862798483830533369, 0.000000000000000000 ) ) ;
#10954 = AXIS2_PLACEMENT_3D ( 'NONE', #20916, #13819, #44149 ) ;
#10955 = AXIS2_PLACEMENT_3D ( 'NONE', #37456, #16164, #4885 ) ;
#10956 = PLANE ( 'NONE',  #26875 ) ;
#10957 = ADVANCED_FACE ( 'NONE', ( #9543 ), #21538, .F. ) ;
#10958 = SURFACE_STYLE_FILL_AREA ( #25633 ) ;
#10959 = CYLINDRICAL_SURFACE ( 'NONE', #28419, 42.00000000000000000 ) ;
#10960 = CIRCLE ( 'NONE', #35203, 31.99999999999997868 ) ;
#10961 = ORIENTED_EDGE ( 'NONE', *, *, #38970, .F. ) ;
#10962 = EDGE_LOOP ( 'NONE', ( #26455, #34328, #27277, #12216 ) ) ;
#10963 = AXIS2_PLACEMENT_3D ( 'NONE', #11376, #4976, #42177 ) ;
#10964 = AXIS2_PLACEMENT_3D ( 'NONE', #33322, #25967, #2969 ) ;
#10965 = ORIENTED_EDGE ( 'NONE', *, *, #32758, .F. ) ;
#10966 = EDGE_CURVE ( 'NONE', #19037, #11173, #33697, .T. ) ;
#10967 = DIRECTION ( 'NONE',  ( -0.9227826878668540234, -0.3853207896976547642, 0.000000000000000000 ) ) ;
#10968 = CYLINDRICAL_SURFACE ( 'NONE', #20668, 82.00000000000000000 ) ;
#10969 = VERTEX_POINT ( 'NONE', #36463 ) ;
#10970 = VERTEX_POINT ( 'NONE', #2927 ) ;
#10971 = DIRECTION ( 'NONE',  ( 1.000000000000000000, 0.000000000000000000, 0.000000000000000000 ) ) ;
#10972 = ORIENTED_EDGE ( 'NONE', *, *, #34800, .F. ) ;
#10973 = ORIENTED_EDGE ( 'NONE', *, *, #44033, .T. ) ;
#10974 = AXIS2_PLACEMENT_3D ( 'NONE', #41995, #45654, #23373 ) ;
#10975 = CARTESIAN_POINT ( 'NONE',  ( -22.67106064244952535, -113.6342314410295842, -2.500000000000000000 ) ) ;
#10976 = EDGE_CURVE ( 'NONE', #17725, #21364, #35979, .T. ) ;
#10978 = ORIENTED_EDGE ( 'NONE', *, *, #12662, .T. ) ;
#10977 = CIRCLE ( 'NONE', #11752, 42.00000000000000000 ) ;
#10979 = DIRECTION ( 'NONE',  ( 0.000000000000000000, 0.000000000000000000, 1.000000000000000000 ) ) ;
#10980 = ORIENTED_EDGE ( 'NONE', *, *, #39463, .T. ) ;
#10981 = CYLINDRICAL_SURFACE ( 'NONE', #18906, 31.99999999999998579 ) ;
#10982 = VECTOR ( 'NONE', #31734, 999.9999999999998863 ) ;
#10983 = CIRCLE ( 'NONE', #3139, 31.99999999999999289 ) ;
#10984 = EDGE_CURVE ( 'NONE', #12855, #43965, #45395, .T. ) ;
#10985 = CYLINDRICAL_SURFACE ( 'NONE', #26242, 42.00000000000000000 ) ;
#10986 = DIRECTION ( 'NONE',  ( 0.000000000000000000, 0.000000000000000000, -1.000000000000000000 ) ) ;
#10987 = EDGE_CURVE ( 'NONE', #46304, #44570, #31389, .T. ) ;
#10988 = VERTEX_POINT ( 'NONE', #6851 ) ;
#10989 = VECTOR ( 'NONE', #25969, 1000.000000000000000 ) ;
#10990 = ORIENTED_EDGE ( 'NONE', *, *, #30605, .F. ) ;
#10991 = VECTOR ( 'NONE', #42914, 1000.000000000000000 ) ;
#10992 = LINE ( 'NONE', #14428, #46152 ) ;
#10993 = CYLINDRICAL_SURFACE ( 'NONE', #18062, 32.00000000000000000 ) ;
#10994 = VERTEX_POINT ( 'NONE', #43805 ) ;
#10995 = AXIS2_PLACEMENT_3D ( 'NONE', #36682, #10755, #44035 ) ;
#10996 = ORIENTED_EDGE ( 'NONE', *, *, #42812, .T. ) ;
#10997 = CARTESIAN_POINT ( 'NONE',  ( -24.50849501662245800, -109.8101191361138831, -5.500000000000000000 ) ) ;
#10998 = LINE ( 'NONE', #36688, #41861 ) ;
#10999 = ORIENTED_EDGE ( 'NONE', *, *, #24101, .T. ) ;
#11000 = CARTESIAN_POINT ( 'NONE',  ( 0.000000000000000000, 36.72794159290334903, -65.59268652807170952 ) ) ;
#11001 = CARTESIAN_POINT ( 'NONE',  ( 10.00000000000000000, -0.6853352020787742971, -37.58145647212455032 ) ) ;
#11002 = FACE_OUTER_BOUND ( 'NONE', #14788, .T. ) ;
#11003 = FACE_OUTER_BOUND ( 'NONE', #4371, .T. ) ;
#11004 = DIRECTION ( 'NONE',  ( -1.000000000000000000, 0.000000000000000000, -0.000000000000000000 ) ) ;
#11005 = DIRECTION ( 'NONE',  ( 1.000000000000000000, -0.000000000000000000, 0.000000000000000000 ) ) ;
#11006 = EDGE_CURVE ( 'NONE', #41954, #33176, #26649, .T. ) ;
#11007 = EDGE_CURVE ( 'NONE', #17038, #29594, #16907, .T. ) ;
#11008 = DIRECTION ( 'NONE',  ( 0.000000000000000000, 0.000000000000000000, -1.000000000000000000 ) ) ;
#11009 = CARTESIAN_POINT ( 'NONE',  ( 0.000000000000000000, -41.76106447765533147, 62.50884508063410294 ) ) ;
#11010 = CARTESIAN_POINT ( 'NONE',  ( 19.12409105625795291, -101.5943176906707919, 5.500000000000000000 ) ) ;
#11011 = CARTESIAN_POINT ( 'NONE',  ( -21.67772167707813935, -110.8034581014852762, -5.500000000000000000 ) ) ;
#11012 = CARTESIAN_POINT ( 'NONE',  ( 0.000000000000000000, 21.40280677340421889, -36.13751322684397138 ) ) ;
#11013 = FACE_OUTER_BOUND ( 'NONE', #13867, .T. ) ;
#11014 = ORIENTED_EDGE ( 'NONE', *, *, #29102, .F. ) ;
#11015 = EDGE_CURVE ( 'NONE', #30305, #19681, #32885, .T. ) ;
#11016 = ORIENTED_EDGE ( 'NONE', *, *, #5330, .F. ) ;
#11017 = CIRCLE ( 'NONE', #8659, 16.00000000000000000 ) ;
#11018 = PRODUCT_DEFINITION_CONTEXT ( 'detailed design', #40098, 'design' ) ;
#11019 = CARTESIAN_POINT ( 'NONE',  ( 6.000000000000000000, -15.33399622253541317, 80.55351364060584274 ) ) ;
#11020 = VECTOR ( 'NONE', #38512, 999.9999999999998863 ) ;
#11021 = CIRCLE ( 'NONE', #11798, 31.99999999999998579 ) ;
#11022 = CARTESIAN_POINT ( 'NONE',  ( 0.000000000000000000, 27.74655509720779634, -77.16300072079631889 ) ) ;
#11023 = ORIENTED_EDGE ( 'NONE', *, *, #15294, .F. ) ;
#11024 = CIRCLE ( 'NONE', #29011, 42.00000000000000000 ) ;
#11025 = ORIENTED_EDGE ( 'NONE', *, *, #11459, .F. ) ;
#11026 = AXIS2_PLACEMENT_3D ( 'NONE', #9016, #46712, #31546 ) ;
#11027 = DIRECTION ( 'NONE',  ( 1.000000000000000000, 0.000000000000000000, -0.000000000000000000 ) ) ;
#11028 = VERTEX_POINT ( 'NONE', #39428 ) ;
#11029 = CARTESIAN_POINT ( 'NONE',  ( 10.00000000000000000, -0.8261519478425671803, -77.49459641780887864 ) ) ;
#11030 = ORIENTED_EDGE ( 'NONE', *, *, #6790, .T. ) ;
#11031 = ORIENTED_EDGE ( 'NONE', *, *, #38591, .T. ) ;
#11032 = ORIENTED_EDGE ( 'NONE', *, *, #26572, .T. ) ;
#11033 = DIRECTION ( 'NONE',  ( -1.000000000000000000, -0.000000000000000000, -0.000000000000000000 ) ) ;
#11034 = CARTESIAN_POINT ( 'NONE',  ( 10.00000000000000000, 0.000000000000000000, 0.000000000000000000 ) ) ;
#11035 = ORIENTED_EDGE ( 'NONE', *, *, #43551, .T. ) ;
#11036 = ORIENTED_EDGE ( 'NONE', *, *, #32452, .T. ) ;
#11037 = DIRECTION ( 'NONE',  ( -0.6862798483830533369, -0.7273375899149812085, 0.000000000000000000 ) ) ;
#11038 = ORIENTED_EDGE ( 'NONE', *, *, #24257, .T. ) ;
#11039 = ADVANCED_FACE ( 'NONE', ( #13719 ), #28648, .T. ) ;
#11040 = CARTESIAN_POINT ( 'NONE',  ( 11.99999999999999822, 65.59268652807263322, -36.72794159290169347 ) ) ;
#11041 = LINE ( 'NONE', #40655, #901 ) ;
#11042 = ADVANCED_FACE ( 'NONE', ( #3897 ), #26422, .T. ) ;
#11043 = ORIENTED_EDGE ( 'NONE', *, *, #32214, .T. ) ;
#11044 = CARTESIAN_POINT ( 'NONE',  ( 11.99999999999999822, 70.52718814184260054, 26.02418014898334420 ) ) ;
#11045 = DIRECTION ( 'NONE',  ( 0.000000000000000000, 0.000000000000000000, 1.000000000000000000 ) ) ;
#11046 = VERTEX_POINT ( 'NONE', #3398 ) ;
#11047 = CIRCLE ( 'NONE', #7129, 32.00000000000000000 ) ;
#11048 = LINE ( 'NONE', #37232, #22661 ) ;
#11049 = CARTESIAN_POINT ( 'NONE',  ( 0.000000000000000000, 0.000000000000000000, 52.00000000000002132 ) ) ;
#11050 = VERTEX_POINT ( 'NONE', #30095 ) ;
#11051 = VECTOR ( 'NONE', #30260, 1000.000000000000000 ) ;
#11052 = CARTESIAN_POINT ( 'NONE',  ( 0.000000000000000000, 15.33399622253483408, 80.55351364060595643 ) ) ;
#11053 = ORIENTED_EDGE ( 'NONE', *, *, #33419, .F. ) ;
#11054 = ORIENTED_EDGE ( 'NONE', *, *, #44897, .T. ) ;
#11055 = CARTESIAN_POINT ( 'NONE',  ( 10.00000000000000000, 26.08949754953024325, 27.05870788708241648 ) ) ;
#11056 = DIRECTION ( 'NONE',  ( 0.000000000000000000, 0.000000000000000000, 1.000000000000000000 ) ) ;
#11057 = VECTOR ( 'NONE', #37361, 1000.000000000000000 ) ;
#11058 = CIRCLE ( 'NONE', #45436, 16.00000000000000000 ) ;
#11059 = CARTESIAN_POINT ( 'NONE',  ( 10.00000000000000000, 0.000000000000000000, 0.000000000000000000 ) ) ;
#11060 = DIRECTION ( 'NONE',  ( 0.000000000000000000, -0.3090169943749449533, -0.9510565162951543083 ) ) ;
#11061 = CARTESIAN_POINT ( 'NONE',  ( 0.000000000000000000, 0.000000000000000000, 0.000000000000000000 ) ) ;
#11062 = CARTESIAN_POINT ( 'NONE',  ( 0.000000000000000000, 0.000000000000000000, 0.000000000000000000 ) ) ;
#11063 = AXIS2_PLACEMENT_3D ( 'NONE', #40080, #21218, #32255 ) ;
#11064 = EDGE_CURVE ( 'NONE', #14109, #12152, #3181, .T. ) ;
#11065 = PLANE ( 'NONE',  #11816 ) ;
#11066 = EDGE_CURVE ( 'NONE', #15059, #5004, #13376, .T. ) ;
#11067 = CARTESIAN_POINT ( 'NONE',  ( -8.826826895187510402, -94.96827758698185562, -2.500000000000000444 ) ) ;
#11068 = ORIENTED_EDGE ( 'NONE', *, *, #26783, .T. ) ;
#11069 = DIRECTION ( 'NONE',  ( 1.000000000000000000, 0.000000000000000000, 0.000000000000000000 ) ) ;
#11070 = EDGE_CURVE ( 'NONE', #43520, #17292, #37187, .T. ) ;
#11071 = PLANE ( 'NONE',  #13628 ) ;
#11072 = VECTOR ( 'NONE', #45359, 1000.000000000000000 ) ;
#11073 = CARTESIAN_POINT ( 'NONE',  ( 5.000000000000000000, -31.52238457039619490, 27.75498641678731104 ) ) ;
#11074 = DIRECTION ( 'NONE',  ( -0.000000000000000000, -0.000000000000000000, -1.000000000000000000 ) ) ;
#11075 = CONICAL_SURFACE ( 'NONE', #25139, 20.64000000000000057, 0.7853981633974482790 ) ;
#11076 = CARTESIAN_POINT ( 'NONE',  ( 11.99999999999999822, 0.000000000000000000, 0.000000000000000000 ) ) ;
#11077 = CYLINDRICAL_SURFACE ( 'NONE', #42555, 31.99999999999999289 ) ;
#11078 = DIRECTION ( 'NONE',  ( 0.000000000000000000, -0.1564344650402380854, 0.9876883405951365491 ) ) ;
#11079 = CARTESIAN_POINT ( 'NONE',  ( 10.00000000000000000, 22.64427369931212297, -30.00120703465181293 ) ) ;
#11080 = ORIENTED_EDGE ( 'NONE', *, *, #6469, .F. ) ;
#11081 = ADVANCED_FACE ( 'NONE', ( #25919 ), #7079, .T. ) ;
#11082 = DIRECTION ( 'NONE',  ( 0.9227826878668540234, 0.3853207896976547087, -0.000000000000000000 ) ) ;
#11083 = VERTEX_POINT ( 'NONE', #30337 ) ;
#11084 = CARTESIAN_POINT ( 'NONE',  ( 6.000000000000000000, -2.543863470247820224, -81.96053171279903893 ) ) ;
#11085 = DIRECTION ( 'NONE',  ( 1.000000000000000000, 0.000000000000000000, 0.000000000000000000 ) ) ;
#11086 = CYLINDRICAL_SURFACE ( 'NONE', #12783, 31.99999999999998579 ) ;
#11087 = ORIENTED_EDGE ( 'NONE', *, *, #40052, .F. ) ;
#11088 = AXIS2_PLACEMENT_3D ( 'NONE', #18281, #14383, #1993 ) ;
#11089 = AXIS2_PLACEMENT_3D ( 'NONE', #4316, #19876, #25835 ) ;
#11090 = CARTESIAN_POINT ( 'NONE',  ( 15.00000000000000000, -10.45096189432314127, 21.10159698893440350 ) ) ;
#11091 = EDGE_LOOP ( 'NONE', ( #3821, #20292, #36054, #14889 ) ) ;
#11092 =( GEOMETRIC_REPRESENTATION_CONTEXT ( 3 ) GLOBAL_UNCERTAINTY_ASSIGNED_CONTEXT ( ( #15425 ) ) GLOBAL_UNIT_ASSIGNED_CONTEXT ( ( #4990, #17195, #35813 ) ) REPRESENTATION_CONTEXT ( 'NONE', 'WORKASPACE' ) );
#11093 = VECTOR ( 'NONE', #12878, 1000.000000000000114 ) ;
#11094 = CARTESIAN_POINT ( 'NONE',  ( 0.000000000000000000, 0.000000000000000000, 0.000000000000000000 ) ) ;
#11095 = ADVANCED_FACE ( 'NONE', ( #33274 ), #40614, .F. ) ;
#11096 = DIRECTION ( 'NONE',  ( -1.000000000000000000, -0.000000000000000000, 0.000000000000000000 ) ) ;
#11098 = ORIENTED_EDGE ( 'NONE', *, *, #28327, .T. ) ;
#11097 = CARTESIAN_POINT ( 'NONE',  ( 6.000000000000000000, -10.30890764327441289, 81.34940948281332851 ) ) ;
#11099 = VECTOR ( 'NONE', #42292, 1000.000000000000000 ) ;
#11100 = EDGE_LOOP ( 'NONE', ( #39952, #17539, #35827, #9472 ) ) ;
#11101 = ADVANCED_FACE ( 'NONE', ( #47950 ), #7323, .T. ) ;
#11102 = DIRECTION ( 'NONE',  ( -1.000000000000000000, 0.000000000000000000, 0.000000000000000000 ) ) ;
#11103 = ORIENTED_EDGE ( 'NONE', *, *, #13668, .F. ) ;
#11104 = EDGE_CURVE ( 'NONE', #39227, #6663, #41117, .T. ) ;
#11105 = DIRECTION ( 'NONE',  ( -1.000000000000000000, 0.000000000000000000, 0.000000000000000000 ) ) ;
#11106 = LINE ( 'NONE', #41216, #19463 ) ;
#11107 = PLANE ( 'NONE',  #23590 ) ;
#11108 = ADVANCED_FACE ( 'NONE', ( #33742 ), #22736, .T. ) ;
#11109 = CARTESIAN_POINT ( 'NONE',  ( 0.000000000000000000, 0.8828120875905820508, -37.48860685352290290 ) ) ;
#11110 = ORIENTED_EDGE ( 'NONE', *, *, #15088, .T. ) ;
#11111 = EDGE_CURVE ( 'NONE', #14894, #41873, #19060, .T. ) ;
#11112 = CARTESIAN_POINT ( 'NONE',  ( 12.49999999999999822, -120.0000000000000000, 125.0000000000000000 ) ) ;
#11113 = ORIENTED_EDGE ( 'NONE', *, *, #19438, .F. ) ;
#11114 = ORIENTED_EDGE ( 'NONE', *, *, #45721, .T. ) ;
#11115 = EDGE_CURVE ( 'NONE', #22715, #13193, #18063, .T. ) ;
#11116 = DIRECTION ( 'NONE',  ( 1.000000000000000000, 0.000000000000000000, 0.000000000000000000 ) ) ;
#11117 = VECTOR ( 'NONE', #1439, 1000.000000000000000 ) ;
#11118 = CARTESIAN_POINT ( 'NONE',  ( 11.99999999999999822, 14.66109333815564852, -73.73191006444555740 ) ) ;
#11119 = DIRECTION ( 'NONE',  ( -1.000000000000000000, 0.000000000000000000, -0.000000000000000000 ) ) ;
#11120 = CARTESIAN_POINT ( 'NONE',  ( -16.06301359042743115, -102.7814171781257357, -2.500000000000000000 ) ) ;
#11121 = ORIENTED_EDGE ( 'NONE', *, *, #37282, .T. ) ;
#11122 = DIRECTION ( 'NONE',  ( 0.000000000000000000, 0.7071067811865437980, 0.7071067811865512365 ) ) ;
#11123 = DIRECTION ( 'NONE',  ( 0.000000000000000000, -1.000000000000000000, 0.000000000000000000 ) ) ;
#11124 = CARTESIAN_POINT ( 'NONE',  ( 10.00000000000000000, 41.91543099594818500, 2.663952781846293139 ) ) ;
#11125 = CIRCLE ( 'NONE', #7202, 31.99999999999999645 ) ;
#11126 = CARTESIAN_POINT ( 'NONE',  ( -22.53294031248082163, -134.0273518838794757, 2.500000000000000000 ) ) ;
#11127 = DIRECTION ( 'NONE',  ( 1.000000000000000000, 0.000000000000000000, -0.000000000000000000 ) ) ;
#11128 = FACE_OUTER_BOUND ( 'NONE', #19913, .T. ) ;
#11129 = ADVANCED_FACE ( 'NONE', ( #14917 ), #29836, .T. ) ;
#11130 = LINE ( 'NONE', #7460, #25540 ) ;
#11131 = CARTESIAN_POINT ( 'NONE',  ( 13.83832728059186046, -142.6495187161941089, 5.500000000000000000 ) ) ;
#11132 = CIRCLE ( 'NONE', #6448, 82.00000000000000000 ) ;
#11133 = CYLINDRICAL_SURFACE ( 'NONE', #43169, 82.00000000000000000 ) ;
#11134 = DIRECTION ( 'NONE',  ( 0.000000000000000000, 0.000000000000000000, 1.000000000000000000 ) ) ;
#11135 = CIRCLE ( 'NONE', #40865, 31.99999999999998224 ) ;
#11136 = CARTESIAN_POINT ( 'NONE',  ( 10.00000000000000000, 21.53537804866081373, 30.80686688397018358 ) ) ;
#11137 = ADVANCED_FACE ( 'NONE', ( #11002 ), #44528, .T. ) ;
#11138 = DIRECTION ( 'NONE',  ( -0.6862798483830534479, -0.7273375899149810975, 0.000000000000000000 ) ) ;
#11139 = CYLINDRICAL_SURFACE ( 'NONE', #40205, 31.99999999999999289 ) ;
#11140 = CARTESIAN_POINT ( 'NONE',  ( 11.99999999999999822, 0.000000000000000000, 0.000000000000000000 ) ) ;
#11141 = DIRECTION ( 'NONE',  ( -1.000000000000000000, -0.000000000000000000, 0.000000000000000000 ) ) ;
#11142 = CIRCLE ( 'NONE', #26789, 32.00000000000000000 ) ;
#11143 = ADVANCED_FACE ( 'NONE', ( #26660 ), #8043, .T. ) ;
#11144 = CARTESIAN_POINT ( 'NONE',  ( 2.117611129180199558, -93.54218975225703048, 5.500000000000000000 ) ) ;
#11145 = VERTEX_POINT ( 'NONE', #33019 ) ;
#11146 = ORIENTED_EDGE ( 'NONE', *, *, #38509, .F. ) ;
#11147 = EDGE_CURVE ( 'NONE', #20756, #42271, #14438, .T. ) ;
#11148 = VERTEX_POINT ( 'NONE', #45991 ) ;
#11149 = VERTEX_POINT ( 'NONE', #12457 ) ;
#11150 = CARTESIAN_POINT ( 'NONE',  ( 10.00000000000000000, -33.17418723428319538, 17.67226234102814431 ) ) ;
#11151 = VECTOR ( 'NONE', #1338, 1000.000000000000000 ) ;
#11152 = ORIENTED_EDGE ( 'NONE', *, *, #33361, .T. ) ;
#11153 = AXIS2_PLACEMENT_3D ( 'NONE', #28003, #9378, #31440 ) ;
#11154 = EDGE_CURVE ( 'NONE', #25587, #14954, #6778, .T. ) ;
#11155 = DIRECTION ( 'NONE',  ( 0.9580045777625452175, 0.2867529058022035837, -0.000000000000000000 ) ) ;
#11156 = ADVANCED_FACE ( 'NONE', ( #9024 ), #42311, .T. ) ;
#11157 = DIRECTION ( 'NONE',  ( -1.000000000000000000, -0.000000000000000000, 0.000000000000000000 ) ) ;
#11158 = FACE_OUTER_BOUND ( 'NONE', #15604, .T. ) ;
#11159 = ORIENTED_EDGE ( 'NONE', *, *, #22634, .F. ) ;
#11160 = DIRECTION ( 'NONE',  ( -1.000000000000000000, -0.000000000000000000, -0.000000000000000000 ) ) ;
#11161 = CIRCLE ( 'NONE', #14304, 16.00000000000000000 ) ;
#11162 = ORIENTED_EDGE ( 'NONE', *, *, #19702, .T. ) ;
#11163 = EDGE_CURVE ( 'NONE', #6523, #14170, #8765, .T. ) ;
#11164 = AXIS2_PLACEMENT_3D ( 'NONE', #28107, #35921, #9979 ) ;
#11165 = ORIENTED_EDGE ( 'NONE', *, *, #22555, .F. ) ;
#11166 = CARTESIAN_POINT ( 'NONE',  ( -23.25244084006223133, -132.7111759872722416, 2.500000000000000000 ) ) ;
#11167 = CYLINDRICAL_SURFACE ( 'NONE', #5567, 31.99999999999998579 ) ;
#11168 = FACE_BOUND ( 'NONE', #1947, .T. ) ;
#11169 = AXIS2_PLACEMENT_3D ( 'NONE', #45925, #38579, #35127 ) ;
#11170 = ORIENTED_EDGE ( 'NONE', *, *, #23984, .T. ) ;
#11171 = ORIENTED_EDGE ( 'NONE', *, *, #808, .F. ) ;
#11172 = FACE_OUTER_BOUND ( 'NONE', #33771, .T. ) ;
#11173 = VERTEX_POINT ( 'NONE', #38658 ) ;
#11174 = EDGE_CURVE ( 'NONE', #33176, #18905, #33325, .T. ) ;
#11175 = CARTESIAN_POINT ( 'NONE',  ( 10.00000000000000000, 0.000000000000000000, 0.000000000000000000 ) ) ;
#11176 = CIRCLE ( 'NONE', #18173, 31.99999999999999289 ) ;
#11177 = DIRECTION ( 'NONE',  ( -1.000000000000000000, 0.000000000000000000, -0.000000000000000000 ) ) ;
#11178 = FACE_OUTER_BOUND ( 'NONE', #9416, .T. ) ;
#11179 = CARTESIAN_POINT ( 'NONE',  ( -13.05994868825747446, -139.5943292883446532, 5.500000000000000000 ) ) ;
#11180 = FACE_OUTER_BOUND ( 'NONE', #24376, .T. ) ;
#11181 = FACE_OUTER_BOUND ( 'NONE', #3135, .T. ) ;
#11182 = LINE ( 'NONE', #44233, #29542 ) ;
#11183 =( NAMED_UNIT ( * ) PLANE_ANGLE_UNIT ( ) SI_UNIT ( $, .RADIAN. ) );
#11184 = DIRECTION ( 'NONE',  ( -1.000000000000000000, 0.000000000000000000, 0.000000000000000000 ) ) ;
#11185 = DIRECTION ( 'NONE',  ( 0.000000000000000000, 0.9510565162951523099, 0.3090169943749517811 ) ) ;
#11186 = ORIENTED_EDGE ( 'NONE', *, *, #26696, .F. ) ;
#11187 = FACE_OUTER_BOUND ( 'NONE', #12485, .T. ) ;
#11188 = VERTEX_POINT ( 'NONE', #700 ) ;
#11189 = DIRECTION ( 'NONE',  ( 0.000000000000000000, 0.3090169943749410675, 0.9510565162951556406 ) ) ;
#11190 = CYLINDRICAL_SURFACE ( 'NONE', #10274, 37.49900000000000233 ) ;
#11191 = AXIS2_PLACEMENT_3D ( 'NONE', #29923, #26264, #44854 ) ;
#11192 = DIRECTION ( 'NONE',  ( 0.000000000000000000, 0.000000000000000000, 1.000000000000000000 ) ) ;
#11193 = CARTESIAN_POINT ( 'NONE',  ( 10.00000000000000000, 0.000000000000000000, 0.000000000000000000 ) ) ;
#11195 = CIRCLE ( 'NONE', #22114, 12.49999999999999645 ) ;
#11194 = FACE_OUTER_BOUND ( 'NONE', #31785, .T. ) ;
#11196 = ORIENTED_EDGE ( 'NONE', *, *, #6452, .F. ) ;
#11197 = LINE ( 'NONE', #42256, #34910 ) ;
#11198 = DIRECTION ( 'NONE',  ( -0.6862798483830533369, -0.7273375899149812085, 0.000000000000000000 ) ) ;
#11199 = VECTOR ( 'NONE', #14622, 1000.000000000000000 ) ;
#11200 = CIRCLE ( 'NONE', #32299, 77.49899999999999523 ) ;
#11201 = DIRECTION ( 'NONE',  ( 0.000000000000000000, -0.8090169943749531134, 0.5877852522924653655 ) ) ;
#11202 = CIRCLE ( 'NONE', #11978, 31.99999999999998579 ) ;
#11203 = FACE_OUTER_BOUND ( 'NONE', #10027, .T. ) ;
#11204 = VERTEX_POINT ( 'NONE', #19523 ) ;
#11205 = ORIENTED_EDGE ( 'NONE', *, *, #47365, .T. ) ;
#11206 = AXIS2_PLACEMENT_3D ( 'NONE', #32865, #29453, #10616 ) ;
#11207 = AXIS2_PLACEMENT_3D ( 'NONE', #45330, #8603, #37754 ) ;
#11208 = EDGE_CURVE ( 'NONE', #12844, #32530, #30232, .T. ) ;
#11209 = VERTEX_POINT ( 'NONE', #4865 ) ;
#11210 = DIRECTION ( 'NONE',  ( 0.000000000000000000, -0.6494480483301904306, 0.7604059656000251577 ) ) ;
#11211 = LINE ( 'NONE', #34198, #43323 ) ;
#11212 = ORIENTED_EDGE ( 'NONE', *, *, #3304, .F. ) ;
#11213 = ORIENTED_EDGE ( 'NONE', *, *, #43142, .T. ) ;
#11214 = DIRECTION ( 'NONE',  ( -1.000000000000000000, -0.000000000000000000, -0.000000000000000000 ) ) ;
#11215 = ORIENTED_EDGE ( 'NONE', *, *, #23473, .T. ) ;
#11216 = ORIENTED_EDGE ( 'NONE', *, *, #32874, .T. ) ;
#11217 = ORIENTED_EDGE ( 'NONE', *, *, #18721, .T. ) ;
#11218 = EDGE_CURVE ( 'NONE', #7093, #23167, #13038, .T. ) ;
#11219 = AXIS2_PLACEMENT_3D ( 'NONE', #11985, #20281, #34238 ) ;
#11220 = DIRECTION ( 'NONE',  ( -1.000000000000000000, 0.000000000000000000, 0.000000000000000000 ) ) ;
#11221 = EDGE_CURVE ( 'NONE', #45989, #6258, #45073, .T. ) ;
#11222 = ORIENTED_EDGE ( 'NONE', *, *, #44618, .T. ) ;
#11223 = CARTESIAN_POINT ( 'NONE',  ( 11.99999999999999822, 0.000000000000000000, 0.000000000000000000 ) ) ;
#11224 = ORIENTED_EDGE ( 'NONE', *, *, #7937, .F. ) ;
#11225 = CARTESIAN_POINT ( 'NONE',  ( 0.000000000000000000, 26.01480285779837232, 70.53064760720326376 ) ) ;
#11226 = ORIENTED_EDGE ( 'NONE', *, *, #8053, .T. ) ;
#11227 = ORIENTED_EDGE ( 'NONE', *, *, #6697, .T. ) ;
#11228 = EDGE_CURVE ( 'NONE', #18553, #17403, #23960, .T. ) ;
#11229 = DIRECTION ( 'NONE',  ( -1.000000000000000000, 0.000000000000000000, 0.000000000000000000 ) ) ;
#11230 = AXIS2_PLACEMENT_3D ( 'NONE', #25791, #16252, #27507 ) ;
#11231 = VECTOR ( 'NONE', #21707, 999.9999999999998863 ) ;
#11232 = VECTOR ( 'NONE', #7884, 1000.000000000000000 ) ;
#11233 = EDGE_CURVE ( 'NONE', #8001, #13193, #1443, .T. ) ;
#11234 = CARTESIAN_POINT ( 'NONE',  ( 11.99999999999999822, -31.46837873495025306, 68.27212725128265447 ) ) ;
#11235 = CARTESIAN_POINT ( 'NONE',  ( 0.000000000000000000, 0.000000000000000000, 0.000000000000000000 ) ) ;
#11236 = ORIENTED_EDGE ( 'NONE', *, *, #25890, .F. ) ;
#11237 = ORIENTED_EDGE ( 'NONE', *, *, #26934, .T. ) ;
#11238 = CARTESIAN_POINT ( 'NONE',  ( 10.00000000000000000, 6.555932627142952995, -37.01155633439051940 ) ) ;
#11239 = DIRECTION ( 'NONE',  ( 0.000000000000000000, 0.000000000000000000, 1.000000000000000000 ) ) ;
#11240 = AXIS2_PLACEMENT_3D ( 'NONE', #31646, #6162, #2022 ) ;
#11241 = AXIS2_PLACEMENT_3D ( 'NONE', #35088, #8182, #8902 ) ;
#11242 = ORIENTED_EDGE ( 'NONE', *, *, #42333, .T. ) ;
#11243 = ORIENTED_EDGE ( 'NONE', *, *, #12788, .F. ) ;
#11244 = AXIS2_PLACEMENT_3D ( 'NONE', #30160, #7863, #30629 ) ;
#11245 = DIRECTION ( 'NONE',  ( 0.000000000000000000, 0.000000000000000000, -1.000000000000000000 ) ) ;
#11246 = VERTEX_POINT ( 'NONE', #16602 ) ;
#11247 = VECTOR ( 'NONE', #43595, 1000.000000000000000 ) ;
#11248 = LINE ( 'NONE', #3894, #26924 ) ;
#11250 = EDGE_CURVE ( 'NONE', #38548, #19364, #31554, .T. ) ;
#11249 = FACE_OUTER_BOUND ( 'NONE', #32888, .T. ) ;
#11251 = DIRECTION ( 'NONE',  ( -1.000000000000000000, 0.000000000000000000, 0.000000000000000000 ) ) ;
#11252 = CARTESIAN_POINT ( 'NONE',  ( 0.000000000000000000, -29.81001611431024045, 22.74946021919122430 ) ) ;
#11253 = CARTESIAN_POINT ( 'NONE',  ( 0.000000000000000000, -62.50329211542407393, -41.76937507738853839 ) ) ;
#11254 = DIRECTION ( 'NONE',  ( -1.000000000000000000, 0.000000000000000000, 0.000000000000000000 ) ) ;
#11255 = AXIS2_PLACEMENT_3D ( 'NONE', #16452, #31403, #32120 ) ;
#11256 = FACE_OUTER_BOUND ( 'NONE', #33970, .T. ) ;
#11257 = DIRECTION ( 'NONE',  ( -1.000000000000000000, -0.000000000000000000, -0.000000000000000000 ) ) ;
#11258 = CARTESIAN_POINT ( 'NONE',  ( 10.00000000000000000, -41.76937507738745836, -62.50329211542482710 ) ) ;
#11259 = VERTEX_POINT ( 'NONE', #12950 ) ;
#11260 = CARTESIAN_POINT ( 'NONE',  ( 10.00000000000000000, 49.70050353004977239, -59.46389618801908483 ) ) ;
#11261 = DIRECTION ( 'NONE',  ( 0.000000000000000000, 0.000000000000000000, 1.000000000000000000 ) ) ;
#11262 = DIRECTION ( 'NONE',  ( -1.000000000000000000, -0.000000000000000000, -0.000000000000000000 ) ) ;
#11263 = CIRCLE ( 'NONE', #38622, 77.49899999999999523 ) ;
#11264 = ORIENTED_EDGE ( 'NONE', *, *, #44587, .F. ) ;
#11265 = VECTOR ( 'NONE', #17675, 1000.000000000000000 ) ;
#11266 = EDGE_CURVE ( 'NONE', #23089, #3690, #38838, .T. ) ;
#11267 = DIRECTION ( 'NONE',  ( -0.000000000000000000, -0.000000000000000000, 1.000000000000000000 ) ) ;
#11268 = CONICAL_SURFACE ( 'NONE', #38634, 12.85999999999999943, 0.7853981633974482790 ) ;
#11269 = CIRCLE ( 'NONE', #38635, 31.99999999999999645 ) ;
#11270 = CIRCLE ( 'NONE', #2648, 11.59999999999999964 ) ;
#11271 = EDGE_CURVE ( 'NONE', #42124, #43612, #27151, .T. ) ;
#11272 = DIRECTION ( 'NONE',  ( 0.000000000000000000, -0.5877852522924801315, 0.8090169943749421222 ) ) ;
#11273 = DIRECTION ( 'NONE',  ( 0.000000000000000000, 0.000000000000000000, -1.000000000000000000 ) ) ;
#11274 = EDGE_CURVE ( 'NONE', #24524, #13681, #42746, .T. ) ;
#11275 = ORIENTED_EDGE ( 'NONE', *, *, #22756, .F. ) ;
#11276 = CIRCLE ( 'NONE', #29227, 31.99999999999997868 ) ;
#11277 = AXIS2_PLACEMENT_3D ( 'NONE', #16496, #13308, #31441 ) ;
#11278 = VECTOR ( 'NONE', #9259, 1000.000000000000000 ) ;
#11279 = CARTESIAN_POINT ( 'NONE',  ( 6.000000000000000000, -74.18225833017864090, -34.94270380257717790 ) ) ;
#11280 = CIRCLE ( 'NONE', #31636, 12.50000000000000000 ) ;
#11281 = ORIENTED_EDGE ( 'NONE', *, *, #1829, .T. ) ;
#11282 = ORIENTED_EDGE ( 'NONE', *, *, #6934, .T. ) ;
#11283 = ORIENTED_EDGE ( 'NONE', *, *, #13389, .F. ) ;
#11284 = ORIENTED_EDGE ( 'NONE', *, *, #46359, .F. ) ;
#11285 = ORIENTED_EDGE ( 'NONE', *, *, #37957, .F. ) ;
#11286 = CARTESIAN_POINT ( 'NONE',  ( 11.99999999999999822, -75.11764819372145041, 29.05362095685286050 ) ) ;
#11287 = AXIS2_PLACEMENT_3D ( 'NONE', #43672, #41371, #14936 ) ;
#11288 = ADVANCED_FACE ( 'NONE', ( #30567 ), #11974, .F. ) ;
#11289 = EDGE_CURVE ( 'NONE', #41663, #21229, #30825, .T. ) ;
#11290 = CARTESIAN_POINT ( 'NONE',  ( 0.000000000000000000, 78.73519480814985627, -22.90783923731548910 ) ) ;
#11291 = ORIENTED_EDGE ( 'NONE', *, *, #14369, .T. ) ;
#11292 = VERTEX_POINT ( 'NONE', #34463 ) ;
#11293 = FACE_OUTER_BOUND ( 'NONE', #250, .T. ) ;
#11294 = ORIENTED_EDGE ( 'NONE', *, *, #29765, .T. ) ;
#11295 = AXIS2_PLACEMENT_3D ( 'NONE', #38401, #42314, #33809 ) ;
#11296 = CARTESIAN_POINT ( 'NONE',  ( 10.00000000000000000, -29.81001611431024756, 22.74946021919122785 ) ) ;
#11297 = CARTESIAN_POINT ( 'NONE',  ( 9.984461079971730157, -95.40710393340120277, -5.500000000000000000 ) ) ;
#11298 = ORIENTED_EDGE ( 'NONE', *, *, #30711, .F. ) ;
#11299 = EDGE_LOOP ( 'NONE', ( #41693, #29207, #10915, #39092 ) ) ;
#11300 = CARTESIAN_POINT ( 'NONE',  ( 0.000000000000000000, 5.835314593368772229, -22.81335362449846826 ) ) ;
#11301 = DIRECTION ( 'NONE',  ( 0.000000000000000000, 0.000000000000000000, 1.000000000000000000 ) ) ;
#11302 = VERTEX_POINT ( 'NONE', #935 ) ;
#11303 = ADVANCED_FACE ( 'NONE', ( #15883 ), #45747, .F. ) ;
#11304 = CARTESIAN_POINT ( 'NONE',  ( 0.000000000000000000, 36.72794159290334903, -65.59268652807170952 ) ) ;
#11305 = AXIS2_PLACEMENT_3D ( 'NONE', #20817, #38714, #43339 ) ;
#11306 = DIRECTION ( 'NONE',  ( -1.000000000000000000, 0.000000000000000000, -0.000000000000000000 ) ) ;
#11307 = ORIENTED_EDGE ( 'NONE', *, *, #39568, .T. ) ;
#11308 = DIRECTION ( 'NONE',  ( -0.000000000000000000, -0.000000000000000000, -1.000000000000000000 ) ) ;
#11309 = ORIENTED_EDGE ( 'NONE', *, *, #42116, .F. ) ;
#11310 = ORIENTED_EDGE ( 'NONE', *, *, #23270, .F. ) ;
#11311 = DIRECTION ( 'NONE',  ( 0.000000000000000000, 0.6691306063588675634, -0.7431448254773856954 ) ) ;
#11312 = AXIS2_PLACEMENT_3D ( 'NONE', #43956, #10682, #40307 ) ;
#11313 = DIRECTION ( 'NONE',  ( -0.7950889364178798102, 0.6064928550163511956, 0.000000000000000000 ) ) ;
#11314 = VERTEX_POINT ( 'NONE', #37068 ) ;
#11315 = AXIS2_PLACEMENT_3D ( 'NONE', #36301, #17699, #47784 ) ;
#11316 = LINE ( 'NONE', #18867, #37884 ) ;
#11317 = CARTESIAN_POINT ( 'NONE',  ( 19.29194287201271862, -133.5026271600380880, 5.500000000000000000 ) ) ;
#11318 = LINE ( 'NONE', #7632, #31564 ) ;
#11319 = AXIS2_PLACEMENT_3D ( 'NONE', #48303, #14781, #29696 ) ;
#11320 = CARTESIAN_POINT ( 'NONE',  ( 10.00000000000000000, -28.89263327155693517, -71.91182617369219088 ) ) ;
#11321 = DIRECTION ( 'NONE',  ( 0.000000000000000000, 0.000000000000000000, -1.000000000000000000 ) ) ;
#11322 = LINE ( 'NONE', #18644, #20818 ) ;
#11323 = CIRCLE ( 'NONE', #29265, 77.49900000000000944 ) ;
#11324 = VECTOR ( 'NONE', #21291, 1000.000000000000000 ) ;
#11325 = CARTESIAN_POINT ( 'NONE',  ( 0.000000000000000000, -0.8261519478436571973, 77.49459641780886443 ) ) ;
#11326 = CARTESIAN_POINT ( 'NONE',  ( 0.000000000000000000, 0.000000000000000000, 0.000000000000000000 ) ) ;
#11327 = CARTESIAN_POINT ( 'NONE',  ( -10.00000000000000000, 0.000000000000000000, 0.000000000000000000 ) ) ;
#11328 = CARTESIAN_POINT ( 'NONE',  ( 11.99999999999999822, 28.89263327155849126, -71.91182617369157981 ) ) ;
#11329 = AXIS2_PLACEMENT_3D ( 'NONE', #3621, #44987, #26389 ) ;
#11330 = CIRCLE ( 'NONE', #26161, 31.99999999999999289 ) ;
#11331 = DIRECTION ( 'NONE',  ( 0.000000000000000000, 0.9945218953682731788, 0.1045284632676559550 ) ) ;
#11332 = DIRECTION ( 'NONE',  ( 0.9580045777625458836, 0.2867529058022011412, -0.000000000000000000 ) ) ;
#11333 = CARTESIAN_POINT ( 'NONE',  ( 0.000000000000000000, -65.64334221924937651, 41.19522573413711797 ) ) ;
#11334 = CARTESIAN_POINT ( 'NONE',  ( 10.00000000000000000, 0.000000000000000000, 0.000000000000000000 ) ) ;
#11335 = AXIS2_PLACEMENT_3D ( 'NONE', #7507, #139, #396 ) ;
#11336 = ORIENTED_EDGE ( 'NONE', *, *, #21555, .T. ) ;
#11337 = EDGE_CURVE ( 'NONE', #14595, #28447, #43522, .T. ) ;
#11338 = CARTESIAN_POINT ( 'NONE',  ( 12.00000000000000000, 0.000000000000000000, 0.000000000000000000 ) ) ;
#11339 = ORIENTED_EDGE ( 'NONE', *, *, #30562, .F. ) ;
#11340 = FACE_OUTER_BOUND ( 'NONE', #10925, .T. ) ;
#11341 = EDGE_CURVE ( 'NONE', #5777, #44023, #37236, .T. ) ;
#11342 = DIRECTION ( 'NONE',  ( -0.9974137572422395737, -0.07187347816767440667, 0.000000000000000000 ) ) ;
#11343 = DIRECTION ( 'NONE',  ( -1.000000000000000000, 0.000000000000000000, 0.000000000000000000 ) ) ;
#11344 = EDGE_CURVE ( 'NONE', #13511, #26518, #13809, .T. ) ;
#11345 = ORIENTED_EDGE ( 'NONE', *, *, #21016, .F. ) ;
#11346 = VECTOR ( 'NONE', #10886, 999.9999999999998863 ) ;
#11347 = VECTOR ( 'NONE', #25071, 1000.000000000000000 ) ;
#11348 = ADVANCED_FACE ( 'NONE', ( #32261 ), #33162, .T. ) ;
#11349 = CARTESIAN_POINT ( 'NONE',  ( 0.000000000000000000, 0.000000000000000000, -40.00000000000000000 ) ) ;
#11350 = EDGE_LOOP ( 'NONE', ( #45531, #18002, #26411, #12846 ) ) ;
#11351 = ORIENTED_EDGE ( 'NONE', *, *, #10738, .F. ) ;
#11352 = EDGE_CURVE ( 'NONE', #13398, #773, #44420, .T. ) ;
#11353 = EDGE_CURVE ( 'NONE', #17893, #40687, #13661, .T. ) ;
#11354 = AXIS2_PLACEMENT_3D ( 'NONE', #11882, #45651, #34372 ) ;
#11355 = AXIS2_PLACEMENT_3D ( 'NONE', #41850, #26671, #30576 ) ;
#11356 = DIRECTION ( 'NONE',  ( -1.000000000000000000, -0.000000000000000000, 0.000000000000000000 ) ) ;
#11357 = EDGE_CURVE ( 'NONE', #37523, #20853, #14805, .T. ) ;
#11358 = DIRECTION ( 'NONE',  ( 0.000000000000000000, 0.000000000000000000, 1.000000000000000000 ) ) ;
#11360 = ORIENTED_EDGE ( 'NONE', *, *, #4927, .F. ) ;
#11359 = CARTESIAN_POINT ( 'NONE',  ( -3.000000000000000000, 26.50000000000000355, 1.500000000000000000 ) ) ;
#11361 = ORIENTED_EDGE ( 'NONE', *, *, #37085, .F. ) ;
#11362 = VECTOR ( 'NONE', #4553, 1000.000000000000000 ) ;
#11363 = AXIS2_PLACEMENT_3D ( 'NONE', #40189, #21579, #47993 ) ;
#11364 = DIRECTION ( 'NONE',  ( -1.000000000000000000, 0.000000000000000000, 0.000000000000000000 ) ) ;
#11365 = CARTESIAN_POINT ( 'NONE',  ( 0.000000000000000000, 74.65374052328660071, -8.840884882374309583 ) ) ;
#11366 = DIRECTION ( 'NONE',  ( 0.000000000000000000, 0.8910065241883688980, -0.4539904997395447506 ) ) ;
#11367 = ADVANCED_FACE ( 'NONE', ( #28105 ), #43277, .F. ) ;
#11368 = DIRECTION ( 'NONE',  ( 1.000000000000000000, 0.000000000000000000, 0.000000000000000000 ) ) ;
#11369 = ORIENTED_EDGE ( 'NONE', *, *, #17993, .T. ) ;
#11370 = CARTESIAN_POINT ( 'NONE',  ( 10.00000000000000000, 74.74816331893477184, -33.71516098798658589 ) ) ;
#11371 = ORIENTED_EDGE ( 'NONE', *, *, #43550, .F. ) ;
#11372 = ORIENTED_EDGE ( 'NONE', *, *, #19702, .F. ) ;
#11373 = DIRECTION ( 'NONE',  ( 0.000000000000000000, 0.000000000000000000, -1.000000000000000000 ) ) ;
#11374 = DIRECTION ( 'NONE',  ( 1.000000000000000000, 0.000000000000000000, 0.000000000000000000 ) ) ;
#11375 = AXIS2_PLACEMENT_3D ( 'NONE', #3163, #47486, #18094 ) ;
#11376 = CARTESIAN_POINT ( 'NONE',  ( 11.99999999999999822, 0.000000000000000000, 0.000000000000000000 ) ) ;
#11377 = CARTESIAN_POINT ( 'NONE',  ( 50.00005079999999680, 0.000000000000000000, 0.000000000000000000 ) ) ;
#11378 = ORIENTED_EDGE ( 'NONE', *, *, #7904, .F. ) ;
#11379 = CARTESIAN_POINT ( 'NONE',  ( 11.99999999999999822, 41.76106447765580043, -62.50884508063379741 ) ) ;
#11380 = DIRECTION ( 'NONE',  ( 0.000000000000000000, 0.000000000000000000, 1.000000000000000000 ) ) ;
#11381 = CARTESIAN_POINT ( 'NONE',  ( 10.00000000000000000, 10.41901085202078114, 40.68715046381932865 ) ) ;
#11382 = FACE_OUTER_BOUND ( 'NONE', #33663, .T. ) ;
#11383 = AXIS2_PLACEMENT_3D ( 'NONE', #43875, #7152, #40218 ) ;
#11384 = CARTESIAN_POINT ( 'NONE',  ( 15.00000000000000000, 24.81905959214275370, 9.408202855044498492 ) ) ;
#11385 = LINE ( 'NONE', #41240, #44136 ) ;
#11386 = CARTESIAN_POINT ( 'NONE',  ( 10.00000000000000000, 29.81001611431041098, -22.74946021919100403 ) ) ;
#11387 = CARTESIAN_POINT ( 'NONE',  ( 0.000000000000000000, -76.69515212746036070, 29.01471420065536932 ) ) ;
#11388 = FACE_OUTER_BOUND ( 'NONE', #32602, .T. ) ;
#11389 = DIRECTION ( 'NONE',  ( 0.000000000000000000, 0.07845909572783797692, 0.9969173337331285190 ) ) ;
#11390 = FACE_OUTER_BOUND ( 'NONE', #24022, .T. ) ;
#11391 = VERTEX_POINT ( 'NONE', #9977 ) ;
#11392 = CIRCLE ( 'NONE', #26228, 77.49899999999999523 ) ;
#11393 = CIRCLE ( 'NONE', #5133, 77.49900000000000944 ) ;
#11394 = DIRECTION ( 'NONE',  ( 1.000000000000000000, -0.000000000000000000, 0.000000000000000000 ) ) ;
#11395 = DIRECTION ( 'NONE',  ( -1.000000000000000000, -0.000000000000000000, -0.000000000000000000 ) ) ;
#11396 = DIRECTION ( 'NONE',  ( 0.000000000000000000, 0.000000000000000000, 1.000000000000000000 ) ) ;
#11397 = LINE ( 'NONE', #37078, #23851 ) ;
#11398 = EDGE_CURVE ( 'NONE', #15864, #27438, #24906, .T. ) ;
#11399 = VECTOR ( 'NONE', #9143, 1000.000000000000000 ) ;
#11400 = ADVANCED_FACE ( 'NONE', ( #25802 ), #6317, .T. ) ;
#11401 = LINE ( 'NONE', #18226, #14280 ) ;
#11402 = EDGE_CURVE ( 'NONE', #25709, #12123, #22402, .T. ) ;
#11403 = VECTOR ( 'NONE', #6118, 1000.000000000000000 ) ;
#11404 = ORIENTED_EDGE ( 'NONE', *, *, #9445, .T. ) ;
#11405 = VERTEX_POINT ( 'NONE', #24189 ) ;
#11406 = EDGE_CURVE ( 'NONE', #9950, #38308, #28654, .T. ) ;
#11407 = ORIENTED_EDGE ( 'NONE', *, *, #15479, .F. ) ;
#11408 = VECTOR ( 'NONE', #1361, 1000.000000000000000 ) ;
#11409 = DIRECTION ( 'NONE',  ( 0.000000000000000000, 0.000000000000000000, 1.000000000000000000 ) ) ;
#11410 = AXIS2_PLACEMENT_3D ( 'NONE', #40281, #47836, #43698 ) ;
#11411 = ORIENTED_EDGE ( 'NONE', *, *, #45700, .T. ) ;
#11412 = EDGE_CURVE ( 'NONE', #35598, #5335, #18216, .T. ) ;
#11413 = CIRCLE ( 'NONE', #3563, 82.00000000000000000 ) ;
#11414 = CARTESIAN_POINT ( 'NONE',  ( 0.000000000000000000, 0.000000000000000000, -1.199999999999999956 ) ) ;
#11415 = ADVANCED_FACE ( 'NONE', ( #13177 ), #43038, .F. ) ;
#11416 = DIRECTION ( 'NONE',  ( 0.000000000000000000, 0.1564344650402244019, 0.9876883405951387696 ) ) ;
#11417 = CYLINDRICAL_SURFACE ( 'NONE', #363, 77.49899999999999523 ) ;
#11418 = EDGE_LOOP ( 'NONE', ( #13863, #14830, #37695, #21344 ) ) ;
#11419 = CARTESIAN_POINT ( 'NONE',  ( -34.02017708624681092, -109.8571428571428470, 102.9091629284897493 ) ) ;
#11420 = ORIENTED_EDGE ( 'NONE', *, *, #19794, .F. ) ;
#11421 = VERTEX_POINT ( 'NONE', #5846 ) ;
#11422 = FACE_OUTER_BOUND ( 'NONE', #27253, .T. ) ;
#11423 = CARTESIAN_POINT ( 'NONE',  ( 6.000000000000000000, 81.34940948281337114, 10.30890764327411446 ) ) ;
#11424 = EDGE_CURVE ( 'NONE', #26639, #22815, #35710, .T. ) ;
#11425 = CARTESIAN_POINT ( 'NONE',  ( 10.00000000000000000, 0.000000000000000000, 0.000000000000000000 ) ) ;
#11426 = VECTOR ( 'NONE', #46263, 1000.000000000000000 ) ;
#11427 = ORIENTED_EDGE ( 'NONE', *, *, #28962, .T. ) ;
#11428 = EDGE_LOOP ( 'NONE', ( #9239, #46216, #20540, #46677 ) ) ;
#11429 = ORIENTED_EDGE ( 'NONE', *, *, #9037, .F. ) ;
#11430 = CYLINDRICAL_SURFACE ( 'NONE', #44283, 42.00000000000000000 ) ;
#11431 = ORIENTED_EDGE ( 'NONE', *, *, #32056, .F. ) ;
#11432 = DIRECTION ( 'NONE',  ( -1.000000000000000000, 0.000000000000000000, -0.000000000000000000 ) ) ;
#11433 = VECTOR ( 'NONE', #29903, 1000.000000000000000 ) ;
#11434 = DIRECTION ( 'NONE',  ( -1.000000000000000000, 0.000000000000000000, 0.000000000000000000 ) ) ;
#11435 = CARTESIAN_POINT ( 'NONE',  ( 0.000000000000000000, -71.21200624218768382, -40.65526001592689909 ) ) ;
#11436 = LINE ( 'NONE', #45419, #44066 ) ;
#11437 = DIRECTION ( 'NONE',  ( 1.000000000000000000, 0.000000000000000000, 0.000000000000000000 ) ) ;
#11438 = DIRECTION ( 'NONE',  ( 0.000000000000000000, -0.1045284632676570791, -0.9945218953682730678 ) ) ;
#11439 = DIRECTION ( 'NONE',  ( 0.000000000000000000, 0.000000000000000000, 1.000000000000000000 ) ) ;
#11440 = ORIENTED_EDGE ( 'NONE', *, *, #1721, .T. ) ;
#11441 = CARTESIAN_POINT ( 'NONE',  ( 10.00000000000000000, -74.65491531819124305, 8.830959090342128448 ) ) ;
#11442 = CARTESIAN_POINT ( 'NONE',  ( 16.30584220631899228, -140.9432449716519784, 5.500000000000000000 ) ) ;
#11443 = ORIENTED_EDGE ( 'NONE', *, *, #6306, .T. ) ;
#11444 = ADVANCED_FACE ( 'NONE', ( #35694 ), #2165, .T. ) ;
#11445 = DIRECTION ( 'NONE',  ( 0.9827303690289279636, 0.1850432970638682395, 0.000000000000000000 ) ) ;
#11446 = ORIENTED_EDGE ( 'NONE', *, *, #15428, .F. ) ;
#11447 = VECTOR ( 'NONE', #22145, 1000.000000000000114 ) ;
#11448 = CARTESIAN_POINT ( 'NONE',  ( 10.00000000000000000, -21.53537804866103045, 30.80686688397002371 ) ) ;
#11449 = CARTESIAN_POINT ( 'NONE',  ( 10.00000000000000000, 0.000000000000000000, 0.000000000000000000 ) ) ;
#11450 = CIRCLE ( 'NONE', #38798, 16.00000000000000000 ) ;
#11451 = LINE ( 'NONE', #3600, #1696 ) ;
#11452 = LINE ( 'NONE', #41537, #29141 ) ;
#11453 = FACE_OUTER_BOUND ( 'NONE', #16413, .T. ) ;
#11454 = CARTESIAN_POINT ( 'NONE',  ( 11.99999999999999822, 31.47745569255237896, -68.26794271651228030 ) ) ;
#11455 = CIRCLE ( 'NONE', #16133, 16.00000000000000355 ) ;
#11456 = EDGE_LOOP ( 'NONE', ( #27915, #38120, #48078, #902 ) ) ;
#11457 = DIRECTION ( 'NONE',  ( 0.000000000000000000, 0.000000000000000000, 1.000000000000000000 ) ) ;
#11458 = PLANE ( 'NONE',  #5800 ) ;
#11459 = EDGE_CURVE ( 'NONE', #38425, #48416, #23346, .T. ) ;
#11460 = EDGE_CURVE ( 'NONE', #9341, #23667, #20858, .T. ) ;
#11461 = DIRECTION ( 'NONE',  ( -1.000000000000000000, -0.000000000000000000, 0.000000000000000000 ) ) ;
#11462 = CARTESIAN_POINT ( 'NONE',  ( -3.759344165985237129, 0.000000000000000000, 0.000000000000000000 ) ) ;
#11463 = ADVANCED_FACE ( 'NONE', ( #30457 ), #12112, .T. ) ;
#11464 = ORIENTED_EDGE ( 'NONE', *, *, #29500, .T. ) ;
#11465 = ADVANCED_FACE ( 'NONE', ( #97 ), #34346, .T. ) ;
#11466 = ORIENTED_EDGE ( 'NONE', *, *, #41288, .T. ) ;
#11467 = AXIS2_PLACEMENT_3D ( 'NONE', #36698, #40394, #25675 ) ;
#11468 = DIRECTION ( 'NONE',  ( -1.000000000000000000, -0.000000000000000000, -0.000000000000000000 ) ) ;
#11469 = DIRECTION ( 'NONE',  ( 0.000000000000000000, 1.000000000000000000, 1.301042606982602757E-15 ) ) ;
#11470 = ORIENTED_EDGE ( 'NONE', *, *, #17227, .F. ) ;
#11471 = VECTOR ( 'NONE', #15525, 1000.000000000000114 ) ;
#11472 = CARTESIAN_POINT ( 'NONE',  ( 11.99999999999999822, 0.000000000000000000, 0.000000000000000000 ) ) ;
#11473 = ORIENTED_EDGE ( 'NONE', *, *, #5124, .T. ) ;
#11474 = VERTEX_POINT ( 'NONE', #33632 ) ;
#11475 = AXIS2_PLACEMENT_3D ( 'NONE', #32972, #22460, #48387 ) ;
#11476 = CARTESIAN_POINT ( 'NONE',  ( 10.00000000000000000, 0.000000000000000000, 0.000000000000000000 ) ) ;
#11477 = CARTESIAN_POINT ( 'NONE',  ( -11.68233973192911535, 2.127397731264211754E-15, 17.37152077436032371 ) ) ;
#11478 = CIRCLE ( 'NONE', #36479, 16.00000000000000000 ) ;
#11479 = DIRECTION ( 'NONE',  ( -1.000000000000000000, 0.000000000000000000, 0.000000000000000000 ) ) ;
#11480 = ORIENTED_EDGE ( 'NONE', *, *, #22995, .T. ) ;
#11481 = CARTESIAN_POINT ( 'NONE',  ( 0.000000000000000000, 0.000000000000000000, 0.000000000000000000 ) ) ;
#11482 = VERTEX_POINT ( 'NONE', #41242 ) ;
#11483 = DIRECTION ( 'NONE',  ( 0.000000000000000000, 0.000000000000000000, 1.000000000000000000 ) ) ;
#11484 = DIRECTION ( 'NONE',  ( -1.000000000000000000, -0.000000000000000000, -0.000000000000000000 ) ) ;
#11485 = DIRECTION ( 'NONE',  ( 0.000000000000000000, 0.000000000000000000, 1.000000000000000000 ) ) ;
#11486 = ORIENTED_EDGE ( 'NONE', *, *, #43826, .F. ) ;
#11487 = EDGE_LOOP ( 'NONE', ( #9784, #35158, #16389, #1221 ) ) ;
#11488 = CIRCLE ( 'NONE', #13826, 31.99999999999998579 ) ;
#11489 = CARTESIAN_POINT ( 'NONE',  ( 10.00000000000000000, -29.81001611430991360, -22.74946021919165418 ) ) ;
#11490 = VECTOR ( 'NONE', #40546, 1000.000000000000114 ) ;
#11491 = ORIENTED_EDGE ( 'NONE', *, *, #16751, .F. ) ;
#11492 = ORIENTED_EDGE ( 'NONE', *, *, #24273, .F. ) ;
#11493 = DIRECTION ( 'NONE',  ( 0.000000000000000000, 0.9876883405951372152, 0.1564344650402347547 ) ) ;
#11494 = ORIENTED_EDGE ( 'NONE', *, *, #32329, .T. ) ;
#11495 = DIRECTION ( 'NONE',  ( 0.000000000000000000, 0.000000000000000000, 1.000000000000000000 ) ) ;
#11496 = CARTESIAN_POINT ( 'NONE',  ( 10.00000000000000000, 26.08949754953024325, 27.05870788708241648 ) ) ;
#11497 = VECTOR ( 'NONE', #5852, 999.9999999999998863 ) ;
#11498 = DIRECTION ( 'NONE',  ( -1.000000000000000000, 0.000000000000000000, -0.000000000000000000 ) ) ;
#11499 = DIRECTION ( 'NONE',  ( 1.000000000000000000, 0.000000000000000000, 0.000000000000000000 ) ) ;
#11500 = CARTESIAN_POINT ( 'NONE',  ( 11.99999999999999822, -50.95692526931287603, -58.39081064771804819 ) ) ;
#11501 = DIRECTION ( 'NONE',  ( 0.000000000000000000, 0.7071067811865439090, 0.7071067811865512365 ) ) ;
#11502 = CARTESIAN_POINT ( 'NONE',  ( 0.000000000000000000, -72.35432306680498016, 20.40083707022857951 ) ) ;
#11503 = AXIS2_PLACEMENT_3D ( 'NONE', #17196, #24562, #23839 ) ;
#11504 = CARTESIAN_POINT ( 'NONE',  ( 15.00000000000000000, 23.59884966291538078, 12.14883922797231008 ) ) ;
#11505 = DIRECTION ( 'NONE',  ( -1.000000000000000000, 0.000000000000000000, -0.000000000000000000 ) ) ;
#11506 = EDGE_CURVE ( 'NONE', #29530, #32691, #8179, .T. ) ;
#11507 = FACE_OUTER_BOUND ( 'NONE', #9570, .T. ) ;
#11508 = DIRECTION ( 'NONE',  ( 0.000000000000000000, 0.2334453638559058630, -0.9723699203976765570 ) ) ;
#11509 = EDGE_CURVE ( 'NONE', #12571, #2183, #37276, .T. ) ;
#11510 = CIRCLE ( 'NONE', #38866, 16.00000000000000000 ) ;
#11511 = CARTESIAN_POINT ( 'NONE',  ( -0.7195005275814509993, -118.6838241033926948, 2.500000000000000000 ) ) ;
#11512 = ORIENTED_EDGE ( 'NONE', *, *, #13477, .F. ) ;
#11513 = VECTOR ( 'NONE', #28774, 1000.000000000000114 ) ;
#11514 = UNCERTAINTY_MEASURE_WITH_UNIT (LENGTH_MEASURE( 1.000000000000000082E-05 ), #31811, 'distance_accuracy_value', 'NONE');
#11515 = CYLINDRICAL_SURFACE ( 'NONE', #34650, 31.99999999999998579 ) ;
#11516 = EDGE_CURVE ( 'NONE', #15480, #42450, #34158, .T. ) ;
#11517 = ADVANCED_FACE ( 'NONE', ( #7694 ), #22861, .T. ) ;
#11518 = CARTESIAN_POINT ( 'NONE',  ( 5.822613034544236399, -142.8165987265839760, 5.500000000000000000 ) ) ;
#11519 = CARTESIAN_POINT ( 'NONE',  ( 0.000000000000000000, 0.000000000000000000, 0.000000000000000000 ) ) ;
#11520 = VERTEX_POINT ( 'NONE', #4284 ) ;
#11521 = LINE ( 'NONE', #8322, #30481 ) ;
#11522 = VERTEX_POINT ( 'NONE', #34119 ) ;
#11523 = ORIENTED_EDGE ( 'NONE', *, *, #28596, .F. ) ;
#11524 = CIRCLE ( 'NONE', #17762, 82.00000000000000000 ) ;
#11525 = ORIENTED_EDGE ( 'NONE', *, *, #9895, .T. ) ;
#11526 = EDGE_LOOP ( 'NONE', ( #47076, #47499, #33440, #20776 ) ) ;
#11527 = VERTEX_POINT ( 'NONE', #45618 ) ;
#11528 = CARTESIAN_POINT ( 'NONE',  ( 15.00000000000000000, 18.84667830672579569, -18.68964196561269375 ) ) ;
#11529 = CARTESIAN_POINT ( 'NONE',  ( -3.000000000000000000, -18.13022148937263012, 15.02647892043544608 ) ) ;
#11530 = AXIS2_PLACEMENT_3D ( 'NONE', #7402, #30637, #25989 ) ;
#11531 = VERTEX_POINT ( 'NONE', #11387 ) ;
#11532 = ORIENTED_EDGE ( 'NONE', *, *, #43005, .T. ) ;
#11533 = FACE_OUTER_BOUND ( 'NONE', #40103, .T. ) ;
#11534 = EDGE_LOOP ( 'NONE', ( #39173, #26273, #685, #14694 ) ) ;
#11535 = CARTESIAN_POINT ( 'NONE',  ( -10.00000000000000000, 0.000000000000000000, 0.000000000000000000 ) ) ;
#11536 = CARTESIAN_POINT ( 'NONE',  ( 22.08297821871651934, -111.8242998470044540, -5.500000000000000000 ) ) ;
#11537 = ORIENTED_EDGE ( 'NONE', *, *, #36902, .F. ) ;
#11538 = DIRECTION ( 'NONE',  ( 0.000000000000000000, 0.000000000000000000, 1.000000000000000000 ) ) ;
#11539 = LINE ( 'NONE', #26463, #39614 ) ;
#11540 = ORIENTED_EDGE ( 'NONE', *, *, #6528, .F. ) ;
#11541 = AXIS2_PLACEMENT_3D ( 'NONE', #30702, #30962, #13735 ) ;
#11542 = CARTESIAN_POINT ( 'NONE',  ( 10.00000000000000000, 2.663952781846733675, -41.91543099594814947 ) ) ;
#11543 = EDGE_CURVE ( 'NONE', #10449, #26599, #38085, .T. ) ;
#11544 = DIRECTION ( 'NONE',  ( 0.000000000000000000, -0.9510565162951536422, -0.3090169943749471182 ) ) ;
#11545 = EDGE_LOOP ( 'NONE', ( #19754, #8506, #31032, #2528 ) ) ;
#11546 = CARTESIAN_POINT ( 'NONE',  ( 0.000000000000000000, 0.000000000000000000, 0.000000000000000000 ) ) ;
#11547 = ORIENTED_EDGE ( 'NONE', *, *, #27524, .F. ) ;
#11548 = ORIENTED_EDGE ( 'NONE', *, *, #45217, .T. ) ;
#11549 = DIRECTION ( 'NONE',  ( -0.3311129884571281101, -0.9435911131814402886, 0.000000000000000000 ) ) ;
#11550 = CYLINDRICAL_SURFACE ( 'NONE', #27859, 32.00000000000000000 ) ;
#11551 = ORIENTED_EDGE ( 'NONE', *, *, #41609, .T. ) ;
#11552 = EDGE_CURVE ( 'NONE', #34978, #40483, #1334, .T. ) ;
#11553 = DIRECTION ( 'NONE',  ( -1.000000000000000000, 0.000000000000000000, 0.000000000000000000 ) ) ;
#11554 = DIRECTION ( 'NONE',  ( 0.000000000000000000, -0.1564344650402380854, 0.9876883405951365491 ) ) ;
#11555 = CARTESIAN_POINT ( 'NONE',  ( 0.000000000000000000, 76.41127070299290835, -12.93880638057234123 ) ) ;
#11556 = EDGE_CURVE ( 'NONE', #21364, #37807, #16978, .T. ) ;
#11557 = CARTESIAN_POINT ( 'NONE',  ( 0.000000000000000000, -120.0000000000000000, 40.00000000000000711 ) ) ;
#11558 = CARTESIAN_POINT ( 'NONE',  ( 0.000000000000000000, 27.13269053701132094, -25.88420570971372570 ) ) ;
#11559 = CARTESIAN_POINT ( 'NONE',  ( -3.000000000000000000, 16.61724383029390140, -20.69703378468903665 ) ) ;
#11560 = AXIS2_PLACEMENT_3D ( 'NONE', #31908, #43146, #35560 ) ;
#11561 = ORIENTED_EDGE ( 'NONE', *, *, #26666, .F. ) ;
#11562 = DIRECTION ( 'NONE',  ( 0.000000000000000000, 0.8090169943749447867, 0.5877852522924769119 ) ) ;
#11563 = CARTESIAN_POINT ( 'NONE',  ( 0.000000000000000000, 0.000000000000000000, 0.000000000000000000 ) ) ;
#11564 = CARTESIAN_POINT ( 'NONE',  ( 0.000000000000000000, -6.736453364083817341, 36.88895765772630142 ) ) ;
#11565 = FACE_OUTER_BOUND ( 'NONE', #43369, .T. ) ;
#11566 = VECTOR ( 'NONE', #16206, 1000.000000000000000 ) ;
#11567 = CARTESIAN_POINT ( 'NONE',  ( -3.000000000000000000, -25.60904388321916159, -6.976881207771517879 ) ) ;
#11568 = CYLINDRICAL_SURFACE ( 'NONE', #24585, 82.00000000000000000 ) ;
#11569 = CARTESIAN_POINT ( 'NONE',  ( 11.99999999999999822, -26.01480285779885904, 70.53064760720306481 ) ) ;
#11570 = EDGE_CURVE ( 'NONE', #42331, #23892, #39639, .T. ) ;
#11571 = DIRECTION ( 'NONE',  ( -1.000000000000000000, 0.000000000000000000, 0.000000000000000000 ) ) ;
#11572 = ADVANCED_FACE ( 'NONE', ( #26305 ), #4748, .T. ) ;
#11573 = EDGE_CURVE ( 'NONE', #46514, #22743, #11616, .T. ) ;
#11574 = ORIENTED_EDGE ( 'NONE', *, *, #33079, .F. ) ;
#11575 = FACE_BOUND ( 'NONE', #9351, .T. ) ;
#11576 = EDGE_LOOP ( 'NONE', ( #22966, #11643, #43417, #48003 ) ) ;
#11577 = CARTESIAN_POINT ( 'NONE',  ( 15.00000000000000000, -0.9646360437375368635, -23.52805723605589705 ) ) ;
#11578 = DIRECTION ( 'NONE',  ( -1.000000000000000000, 0.000000000000000000, -0.000000000000000000 ) ) ;
#11579 = VERTEX_POINT ( 'NONE', #7461 ) ;
#11580 = VECTOR ( 'NONE', #42086, 1000.000000000000000 ) ;
#11581 = DIRECTION ( 'NONE',  ( 1.000000000000000000, 0.000000000000000000, 0.000000000000000000 ) ) ;
#11582 = VERTEX_POINT ( 'NONE', #30956 ) ;
#11583 = CIRCLE ( 'NONE', #7563, 31.99999999999998934 ) ;
#11584 = CARTESIAN_POINT ( 'NONE',  ( 0.000000000000000000, 41.81611651403868990, -3.925862922255709542 ) ) ;
#11585 = DIRECTION ( 'NONE',  ( -1.000000000000000000, 0.000000000000000000, -0.000000000000000000 ) ) ;
#11587 = ORIENTED_EDGE ( 'NONE', *, *, #18908, .F. ) ;
#11586 = LINE ( 'NONE', #26515, #6700 ) ;
#11588 = ORIENTED_EDGE ( 'NONE', *, *, #28674, .T. ) ;
#11589 = VECTOR ( 'NONE', #2691, 1000.000000000000000 ) ;
#11590 = VECTOR ( 'NONE', #48123, 1000.000000000000114 ) ;
#11591 = CYLINDRICAL_SURFACE ( 'NONE', #3470, 82.00000000000000000 ) ;
#11592 = DIRECTION ( 'NONE',  ( 0.000000000000000000, 0.000000000000000000, -1.000000000000000000 ) ) ;
#11593 = EDGE_CURVE ( 'NONE', #15673, #31729, #41475, .T. ) ;
#11594 = FACE_OUTER_BOUND ( 'NONE', #1928, .T. ) ;
#11595 = DIRECTION ( 'NONE',  ( 0.000000000000000000, 0.000000000000000000, 1.000000000000000000 ) ) ;
#11596 = ADVANCED_FACE ( 'NONE', ( #22393 ), #37318, .T. ) ;
#11597 = ORIENTED_EDGE ( 'NONE', *, *, #11602, .T. ) ;
#11598 = DIRECTION ( 'NONE',  ( -1.000000000000000000, -0.000000000000000000, 0.000000000000000000 ) ) ;
#11599 = VERTEX_POINT ( 'NONE', #39010 ) ;
#11600 = ORIENTED_EDGE ( 'NONE', *, *, #28083, .T. ) ;
#11601 = LINE ( 'NONE', #21878, #10591 ) ;
#11602 = EDGE_CURVE ( 'NONE', #5896, #32654, #16971, .T. ) ;
#11603 = DIRECTION ( 'NONE',  ( -1.000000000000000000, -0.000000000000000000, 0.000000000000000000 ) ) ;
#11604 = CARTESIAN_POINT ( 'NONE',  ( 10.00000000000000000, 0.000000000000000000, 0.000000000000000000 ) ) ;
#11605 = CARTESIAN_POINT ( 'NONE',  ( 10.00000000000000000, 26.79245525562714647, 32.34446384429980981 ) ) ;
#11606 = VERTEX_POINT ( 'NONE', #24082 ) ;
#11607 = FACE_OUTER_BOUND ( 'NONE', #781, .T. ) ;
#11608 = EDGE_CURVE ( 'NONE', #4566, #42537, #48239, .T. ) ;
#11609 = CYLINDRICAL_SURFACE ( 'NONE', #37757, 31.99999999999998579 ) ;
#11610 = CARTESIAN_POINT ( 'NONE',  ( -20.30386590532152979, -102.9045904027214959, -5.500000000000000000 ) ) ;
#11611 = VECTOR ( 'NONE', #30271, 1000.000000000000000 ) ;
#11612 = DIRECTION ( 'NONE',  ( -1.000000000000000000, 0.000000000000000000, 0.000000000000000000 ) ) ;
#11613 = CARTESIAN_POINT ( 'NONE',  ( -20.30386590532152979, -102.9045904027214959, 5.500000000000000000 ) ) ;
#11614 = LINE ( 'NONE', #19654, #15295 ) ;
#11615 = DIRECTION ( 'NONE',  ( 0.000000000000000000, -0.7071067811865537900, 0.7071067811865413555 ) ) ;
#11616 = LINE ( 'NONE', #16014, #23232 ) ;
#11617 = EDGE_CURVE ( 'NONE', #39337, #31941, #30266, .T. ) ;
#11618 = CYLINDRICAL_SURFACE ( 'NONE', #15802, 31.99999999999998579 ) ;
#11619 = DIRECTION ( 'NONE',  ( 0.000000000000000000, 0.8910065241883690090, -0.4539904997395446395 ) ) ;
#11620 = EDGE_CURVE ( 'NONE', #29705, #22027, #23581, .T. ) ;
#11621 = EDGE_CURVE ( 'NONE', #2795, #40846, #28227, .T. ) ;
#11622 = CARTESIAN_POINT ( 'NONE',  ( 11.99999999999999822, 0.000000000000000000, 0.000000000000000000 ) ) ;
#11623 = LINE ( 'NONE', #41005, #25601 ) ;
#11624 = CARTESIAN_POINT ( 'NONE',  ( 0.000000000000000000, 0.000000000000000000, 0.000000000000000000 ) ) ;
#11625 = CARTESIAN_POINT ( 'NONE',  ( 10.00000000000000000, 75.11725578898467859, 2.956366410620910656 ) ) ;
#11626 = ORIENTED_EDGE ( 'NONE', *, *, #18107, .F. ) ;
#11627 = VECTOR ( 'NONE', #32487, 1000.000000000000000 ) ;
#11628 = AXIS2_PLACEMENT_3D ( 'NONE', #20028, #46718, #43034 ) ;
#11629 = AXIS2_PLACEMENT_3D ( 'NONE', #36085, #43190, #47570 ) ;
#11630 = CARTESIAN_POINT ( 'NONE',  ( 5.000000000000000000, 26.79245525562762253, -32.34446384429941901 ) ) ;
#11631 = ORIENTED_EDGE ( 'NONE', *, *, #13550, .T. ) ;
#11632 = EDGE_CURVE ( 'NONE', #23778, #45628, #6816, .T. ) ;
#11633 = EDGE_LOOP ( 'NONE', ( #135, #44409, #24395, #14497 ) ) ;
#11634 = LINE ( 'NONE', #29745, #17160 ) ;
#11635 = ORIENTED_EDGE ( 'NONE', *, *, #23599, .F. ) ;
#11636 = AXIS2_PLACEMENT_3D ( 'NONE', #13959, #6619, #3667 ) ;
#11637 = LINE ( 'NONE', #1093, #36311 ) ;
#11638 = DIRECTION ( 'NONE',  ( 0.000000000000000000, 0.9723699203976773342, -0.2334453638559023381 ) ) ;
#11640 = ORIENTED_EDGE ( 'NONE', *, *, #17521, .F. ) ;
#11639 = CYLINDRICAL_SURFACE ( 'NONE', #24584, 77.49899999999999523 ) ;
#11641 = EDGE_LOOP ( 'NONE', ( #47262, #238, #24713, #8236 ) ) ;
#11642 = CARTESIAN_POINT ( 'NONE',  ( 0.000000000000000000, 0.000000000000000000, 0.000000000000000000 ) ) ;
#11643 = ORIENTED_EDGE ( 'NONE', *, *, #14094, .F. ) ;
#11644 = ORIENTED_EDGE ( 'NONE', *, *, #34412, .T. ) ;
#11645 = DIRECTION ( 'NONE',  ( -1.000000000000000000, -0.000000000000000000, -0.000000000000000000 ) ) ;
#11646 = CARTESIAN_POINT ( 'NONE',  ( -7.001685179585692254, -14.98378029539707512, -1.199999999999999956 ) ) ;
#11647 = CARTESIAN_POINT ( 'NONE',  ( 10.00000000000000000, 74.74816331893428867, 33.71516098798765881 ) ) ;
#11648 = ORIENTED_EDGE ( 'NONE', *, *, #22346, .F. ) ;
#11649 = EDGE_LOOP ( 'NONE', ( #9254, #42339, #29232, #7727 ) ) ;
#11650 = ORIENTED_EDGE ( 'NONE', *, *, #45402, .T. ) ;
#11651 = AXIS2_PLACEMENT_3D ( 'NONE', #7774, #4116, #27121 ) ;
#11652 = CARTESIAN_POINT ( 'NONE',  ( 11.99999999999999822, 67.80270845531956070, -46.11716303203111522 ) ) ;
#11653 = ORIENTED_EDGE ( 'NONE', *, *, #30664, .T. ) ;
#11654 = LINE ( 'NONE', #21936, #47274 ) ;
#11656 = ADVANCED_FACE ( 'NONE', ( #46114 ), #35326, .T. ) ;
#11655 = CIRCLE ( 'NONE', #39020, 0.5000000000000004441 ) ;
#11657 = FACE_OUTER_BOUND ( 'NONE', #36851, .T. ) ;
#11659 = CARTESIAN_POINT ( 'NONE',  ( 9.984461079971730157, -95.40710393340120277, 5.500000000000000000 ) ) ;
#11658 = AXIS2_PLACEMENT_3D ( 'NONE', #650, #7752, #18753 ) ;
#11660 = CARTESIAN_POINT ( 'NONE',  ( 10.00000000000000000, 33.17418723428333749, -17.67226234102790272 ) ) ;
#11661 = CYLINDRICAL_SURFACE ( 'NONE', #46243, 82.00000000000000000 ) ;
#11662 = DIRECTION ( 'NONE',  ( -0.000000000000000000, -0.000000000000000000, -1.000000000000000000 ) ) ;
#11663 = AXIS2_PLACEMENT_3D ( 'NONE', #10137, #36562, #13828 ) ;
#11664 = EDGE_CURVE ( 'NONE', #21034, #8377, #45880, .T. ) ;
#11665 = DIRECTION ( 'NONE',  ( -1.000000000000000000, 0.000000000000000000, -0.000000000000000000 ) ) ;
#11666 = CARTESIAN_POINT ( 'NONE',  ( 5.000000000000002665, 81.90746397400393164, -3.894527615416986333 ) ) ;
#11667 = LINE ( 'NONE', #29540, #44129 ) ;
#11668 = ORIENTED_EDGE ( 'NONE', *, *, #31214, .T. ) ;
#11669 = LINE ( 'NONE', #41769, #40757 ) ;
#11670 = ORIENTED_EDGE ( 'NONE', *, *, #20889, .F. ) ;
#11671 = VERTEX_POINT ( 'NONE', #2276 ) ;
#11672 = EDGE_CURVE ( 'NONE', #41802, #45751, #8646, .T. ) ;
#11673 = DIRECTION ( 'NONE',  ( 0.000000000000000000, 0.8910065241883656784, 0.4539904997395510788 ) ) ;
#11674 = DIRECTION ( 'NONE',  ( -1.000000000000000000, 0.000000000000000000, -0.000000000000000000 ) ) ;
#11675 = CARTESIAN_POINT ( 'NONE',  ( 8.452893869119503023, -12.51233732111638375, 0.000000000000000000 ) ) ;
#11676 = PLANE ( 'NONE',  #7276 ) ;
#11677 = ADVANCED_FACE ( 'NONE', ( #31195 ), #9376, .T. ) ;
#11678 = DIRECTION ( 'NONE',  ( 0.1850432970638682395, -0.9827303690289279636, 0.000000000000000000 ) ) ;
#11679 = STYLED_ITEM ( 'NONE', ( #21237 ), #21055 ) ;
#11680 = DIRECTION ( 'NONE',  ( -1.000000000000000000, 0.000000000000000000, 0.000000000000000000 ) ) ;
#11681 = ORIENTED_EDGE ( 'NONE', *, *, #5598, .T. ) ;
#11682 = FACE_OUTER_BOUND ( 'NONE', #23874, .T. ) ;
#11683 = DIRECTION ( 'NONE',  ( -1.000000000000000000, 0.000000000000000000, -0.000000000000000000 ) ) ;
#11684 = EDGE_CURVE ( 'NONE', #40419, #13689, #28002, .T. ) ;
#11685 = DIRECTION ( 'NONE',  ( 0.000000000000000000, -0.2079116908177641998, -0.9781476007338046896 ) ) ;
#11686 = ORIENTED_EDGE ( 'NONE', *, *, #47022, .F. ) ;
#11687 = ADVANCED_FACE ( 'NONE', ( #43163 ), #12349, .T. ) ;
#11688 = CIRCLE ( 'NONE', #1523, 31.99999999999999289 ) ;
#11689 = AXIS2_PLACEMENT_3D ( 'NONE', #26796, #45392, #44438 ) ;
#11690 = ORIENTED_EDGE ( 'NONE', *, *, #11672, .T. ) ;
#11691 = CARTESIAN_POINT ( 'NONE',  ( -89.17737905728745318, -39.70432723693717492, 5.500000000000000000 ) ) ;
#11692 = FACE_OUTER_BOUND ( 'NONE', #46123, .T. ) ;
#11693 = VERTEX_POINT ( 'NONE', #42435 ) ;
#11694 = EDGE_CURVE ( 'NONE', #31325, #2585, #24314, .T. ) ;
#11695 = VECTOR ( 'NONE', #3266, 1000.000000000000000 ) ;
#11696 = DIRECTION ( 'NONE',  ( 0.000000000000000000, 0.000000000000000000, 1.000000000000000000 ) ) ;
#11697 = EDGE_LOOP ( 'NONE', ( #4468, #46750, #48230, #35173 ) ) ;
#11698 = ORIENTED_EDGE ( 'NONE', *, *, #7990, .T. ) ;
#11699 = PRODUCT_DEFINITION_SHAPE ( 'NONE', 'NONE',  #48453 ) ;
#11700 = DIRECTION ( 'NONE',  ( 0.000000000000000000, 0.000000000000000000, 1.000000000000000000 ) ) ;
#11702 = ORIENTED_EDGE ( 'NONE', *, *, #47263, .T. ) ;
#11701 = CARTESIAN_POINT ( 'NONE',  ( 10.00000000000000000, -30.84782396557233142, 21.32104025579104345 ) ) ;
#11703 = DIRECTION ( 'NONE',  ( 0.3311129884571280546, 0.9435911131814402886, 0.000000000000000000 ) ) ;
#11704 = ORIENTED_EDGE ( 'NONE', *, *, #1558, .F. ) ;
#11705 = ORIENTED_EDGE ( 'NONE', *, *, #35350, .F. ) ;
#11706 = CARTESIAN_POINT ( 'NONE',  ( 15.00000000000000000, 22.07842321921480888, -8.187992925817425771 ) ) ;
#11707 = ORIENTED_EDGE ( 'NONE', *, *, #17551, .F. ) ;
#11708 = ORIENTED_EDGE ( 'NONE', *, *, #14658, .T. ) ;
#11709 = ADVANCED_FACE ( 'NONE', ( #5718 ), #4991, .F. ) ;
#11710 = DIRECTION ( 'NONE',  ( -1.000000000000000000, 0.000000000000000000, 0.000000000000000000 ) ) ;
#11711 = ADVANCED_FACE ( 'NONE', ( #12824 ), #39501, .T. ) ;
#11712 = FACE_OUTER_BOUND ( 'NONE', #15153, .T. ) ;
#11713 = DIRECTION ( 'NONE',  ( 0.000000000000000000, -0.9969173337331270757, -0.07845909572785580988 ) ) ;
#11714 = VERTEX_POINT ( 'NONE', #19908 ) ;
#11715 = EDGE_CURVE ( 'NONE', #6597, #19561, #38526, .T. ) ;
#11716 = VERTEX_POINT ( 'NONE', #44362 ) ;
#11717 = DIRECTION ( 'NONE',  ( 0.000000000000000000, 0.8910065241883688980, -0.4539904997395445840 ) ) ;
#11718 = EDGE_CURVE ( 'NONE', #39725, #34042, #40458, .T. ) ;
#11719 = AXIS2_PLACEMENT_3D ( 'NONE', #48118, #10916, #44446 ) ;
#11720 = DIRECTION ( 'NONE',  ( 0.08130631524009970801, -0.9966891607226786576, 0.000000000000000000 ) ) ;
#11721 = ORIENTED_EDGE ( 'NONE', *, *, #13450, .T. ) ;
#11722 = VECTOR ( 'NONE', #25284, 1000.000000000000000 ) ;
#11723 = ORIENTED_EDGE ( 'NONE', *, *, #10219, .F. ) ;
#11724 = EDGE_CURVE ( 'NONE', #11880, #20505, #34929, .T. ) ;
#11725 = CARTESIAN_POINT ( 'NONE',  ( 10.00000000000000000, 14.67089635893713684, 73.72996012237443608 ) ) ;
#11726 = ORIENTED_EDGE ( 'NONE', *, *, #21495, .T. ) ;
#11727 = CARTESIAN_POINT ( 'NONE',  ( 10.00000000000000000, -33.17418723428319538, 17.67226234102814431 ) ) ;
#11728 = CIRCLE ( 'NONE', #27383, 82.00000000000000000 ) ;
#11729 = CYLINDRICAL_SURFACE ( 'NONE', #39433, 42.00000000000000000 ) ;
#11730 = CARTESIAN_POINT ( 'NONE',  ( 6.000000000000000000, -80.28980883073747066, -16.65972982745017461 ) ) ;
#11731 = DIRECTION ( 'NONE',  ( -1.000000000000000000, 0.000000000000000000, 0.000000000000000000 ) ) ;
#11732 = VERTEX_POINT ( 'NONE', #48025 ) ;
#11733 = DIRECTION ( 'NONE',  ( 0.000000000000000000, 0.5877852522924685852, 0.8090169943749508930 ) ) ;
#11734 = CARTESIAN_POINT ( 'NONE',  ( 10.00000000000000000, -35.53030884539077050, -12.26510123303296851 ) ) ;
#11735 = CIRCLE ( 'NONE', #32806, 31.99999999999998934 ) ;
#11736 = DIRECTION ( 'NONE',  ( 0.000000000000000000, 0.4539904997395413089, 0.8910065241883705633 ) ) ;
#11737 = CARTESIAN_POINT ( 'NONE',  ( 11.99999999999999822, -34.94270380257692921, 74.18225833017875459 ) ) ;
#11738 = DIRECTION ( 'NONE',  ( -1.000000000000000000, 0.000000000000000000, -0.000000000000000000 ) ) ;
#11739 = LINE ( 'NONE', #23465, #40929 ) ;
#11740 = DIRECTION ( 'NONE',  ( 0.2867529058022035837, -0.9580045777625452175, 0.000000000000000000 ) ) ;
#11741 = DIRECTION ( 'NONE',  ( -1.000000000000000000, -0.000000000000000000, 0.000000000000000000 ) ) ;
#11742 = VERTEX_POINT ( 'NONE', #40220 ) ;
#11743 = EDGE_CURVE ( 'NONE', #33332, #9321, #13077, .T. ) ;
#11744 = DIRECTION ( 'NONE',  ( 0.000000000000000000, 0.000000000000000000, 1.000000000000000000 ) ) ;
#11745 = CARTESIAN_POINT ( 'NONE',  ( 11.99999999999999822, 28.89263327155746097, 71.91182617369197771 ) ) ;
#11746 = EDGE_CURVE ( 'NONE', #31534, #20915, #8381, .T. ) ;
#11747 = CARTESIAN_POINT ( 'NONE',  ( 10.00000000000000000, 68.27212725128275395, -31.46837873495001503 ) ) ;
#11748 = VERTEX_POINT ( 'NONE', #25744 ) ;
#11749 = VERTEX_POINT ( 'NONE', #21835 ) ;
#11750 = AXIS2_PLACEMENT_3D ( 'NONE', #5748, #24339, #43188 ) ;
#11751 = EDGE_CURVE ( 'NONE', #32221, #37634, #47321, .T. ) ;
#11752 = AXIS2_PLACEMENT_3D ( 'NONE', #7432, #18673, #11358 ) ;
#11753 = DIRECTION ( 'NONE',  ( 0.000000000000000000, 0.8660254037844432595, -0.4999999999999919509 ) ) ;
#11754 = AXIS2_PLACEMENT_3D ( 'NONE', #35370, #46648, #13111 ) ;
#11755 = CIRCLE ( 'NONE', #16442, 12.50000000000000000 ) ;
#11756 = ORIENTED_EDGE ( 'NONE', *, *, #5220, .F. ) ;
#11757 = ORIENTED_EDGE ( 'NONE', *, *, #10236, .T. ) ;
#11758 = ORIENTED_EDGE ( 'NONE', *, *, #14094, .T. ) ;
#11759 = ORIENTED_EDGE ( 'NONE', *, *, #24048, .F. ) ;
#11760 = ORIENTED_EDGE ( 'NONE', *, *, #6246, .T. ) ;
#11761 = AXIS2_PLACEMENT_3D ( 'NONE', #21164, #35857, #6021 ) ;
#11762 = DIRECTION ( 'NONE',  ( 0.000000000000000000, 0.8910065241883688980, -0.4539904997395446951 ) ) ;
#11763 = CIRCLE ( 'NONE', #36772, 31.99999999999999289 ) ;
#11764 = ORIENTED_EDGE ( 'NONE', *, *, #47009, .T. ) ;
#11765 = ORIENTED_EDGE ( 'NONE', *, *, #14278, .T. ) ;
#11766 = ADVANCED_FACE ( 'NONE', ( #2756 ), #36760, .T. ) ;
#11767 = DIRECTION ( 'NONE',  ( 0.000000000000000000, 0.000000000000000000, 1.000000000000000000 ) ) ;
#11768 = ORIENTED_EDGE ( 'NONE', *, *, #6511, .T. ) ;
#11769 = DIRECTION ( 'NONE',  ( -1.000000000000000000, 0.000000000000000000, 0.000000000000000000 ) ) ;
#11770 = EDGE_CURVE ( 'NONE', #39596, #42540, #9868, .T. ) ;
#11771 = DIRECTION ( 'NONE',  ( -1.000000000000000000, 0.000000000000000000, 0.000000000000000000 ) ) ;
#11772 = DIRECTION ( 'NONE',  ( -1.000000000000000000, 0.000000000000000000, -0.000000000000000000 ) ) ;
#11773 = ORIENTED_EDGE ( 'NONE', *, *, #8442, .T. ) ;
#11775 = ORIENTED_EDGE ( 'NONE', *, *, #927, .T. ) ;
#11774 = DIRECTION ( 'NONE',  ( -1.000000000000000000, 0.000000000000000000, -0.000000000000000000 ) ) ;
#11776 = DIRECTION ( 'NONE',  ( 0.000000000000000000, 0.9238795325112851842, 0.3826834323650938341 ) ) ;
#11777 = VERTEX_POINT ( 'NONE', #43412 ) ;
#11778 = DIRECTION ( 'NONE',  ( -1.000000000000000000, -0.000000000000000000, 0.000000000000000000 ) ) ;
#11779 = VERTEX_POINT ( 'NONE', #37003 ) ;
#11780 = EDGE_CURVE ( 'NONE', #15249, #15994, #35736, .T. ) ;
#11781 = DIRECTION ( 'NONE',  ( -1.000000000000000000, 0.000000000000000000, 0.000000000000000000 ) ) ;
#11782 = DIRECTION ( 'NONE',  ( 0.000000000000000000, 0.000000000000000000, 1.000000000000000000 ) ) ;
#11783 = ORIENTED_EDGE ( 'NONE', *, *, #12897, .T. ) ;
#11784 = DIRECTION ( 'NONE',  ( -1.000000000000000000, -0.000000000000000000, -0.000000000000000000 ) ) ;
#11785 = EDGE_CURVE ( 'NONE', #18781, #1295, #25254, .T. ) ;
#11786 = CARTESIAN_POINT ( 'NONE',  ( 0.000000000000000000, -35.95386929396264009, 10.96151621346475658 ) ) ;
#11787 = CARTESIAN_POINT ( 'NONE',  ( 11.99999999999999822, -46.53671651293907274, -59.03961581697448935 ) ) ;
#11788 = CARTESIAN_POINT ( 'NONE',  ( 5.000000000000002665, -10.30890764327441822, 81.34940948281332851 ) ) ;
#11789 = CYLINDRICAL_SURFACE ( 'NONE', #32909, 82.00000000000000000 ) ;
#11791 = AXIS2_PLACEMENT_3D ( 'NONE', #24077, #19904, #20382 ) ;
#11790 = DIRECTION ( 'NONE',  ( -1.000000000000000000, -0.000000000000000000, 0.000000000000000000 ) ) ;
#11792 = ORIENTED_EDGE ( 'NONE', *, *, #26851, .T. ) ;
#11793 = AXIS2_PLACEMENT_3D ( 'NONE', #21695, #44451, #17535 ) ;
#11794 = CARTESIAN_POINT ( 'NONE',  ( 10.00000000000000000, 64.81221759200417409, -50.23322058963275794 ) ) ;
#11795 = DIRECTION ( 'NONE',  ( 1.000000000000000000, -0.000000000000000000, -0.000000000000000000 ) ) ;
#11796 = DIRECTION ( 'NONE',  ( 0.000000000000000000, 0.000000000000000000, 1.000000000000000000 ) ) ;
#11797 = CIRCLE ( 'NONE', #17261, 82.00000000000000000 ) ;
#11798 = AXIS2_PLACEMENT_3D ( 'NONE', #18787, #18314, #25895 ) ;
#11799 = CARTESIAN_POINT ( 'NONE',  ( -10.94538922500103162, 1.915100337961297692E-15, -13.90444123027096879 ) ) ;
#11800 = DIRECTION ( 'NONE',  ( 0.000000000000000000, 0.000000000000000000, 1.000000000000000000 ) ) ;
#11801 = DIRECTION ( 'NONE',  ( 0.000000000000000000, -0.9510565162951543083, 0.3090169943749449533 ) ) ;
#11802 = CYLINDRICAL_SURFACE ( 'NONE', #4583, 42.00000000000000000 ) ;
#11803 = VECTOR ( 'NONE', #44079, 1000.000000000000000 ) ;
#11804 = EDGE_CURVE ( 'NONE', #37445, #2183, #17917, .T. ) ;
#11805 = AXIS2_PLACEMENT_3D ( 'NONE', #9795, #31859, #21280 ) ;
#11806 = VERTEX_POINT ( 'NONE', #6205 ) ;
#11807 = FACE_OUTER_BOUND ( 'NONE', #13707, .T. ) ;
#11808 = VERTEX_POINT ( 'NONE', #21610 ) ;
#11809 = LINE ( 'NONE', #299, #24454 ) ;
#11810 = APPLICATION_PROTOCOL_DEFINITION ( 'draft international standard', 'automotive_design', 1998, #22579 ) ;
#11811 = CARTESIAN_POINT ( 'NONE',  ( 15.00000000000000000, 26.49999999999999645, 1.499999999999995781 ) ) ;
#11812 = ORIENTED_EDGE ( 'NONE', *, *, #44773, .F. ) ;
#11813 = EDGE_CURVE ( 'NONE', #22090, #18915, #47771, .T. ) ;
#11814 = DIRECTION ( 'NONE',  ( 1.000000000000000000, -0.000000000000000000, -0.000000000000000000 ) ) ;
#11815 = ORIENTED_EDGE ( 'NONE', *, *, #4458, .T. ) ;
#11816 = AXIS2_PLACEMENT_3D ( 'NONE', #37492, #276, #44113 ) ;
#11817 = CARTESIAN_POINT ( 'NONE',  ( 26.09152095774781799, -124.8716048804687375, 5.500000000000000000 ) ) ;
#11818 = ORIENTED_EDGE ( 'NONE', *, *, #29087, .F. ) ;
#11819 = AXIS2_PLACEMENT_3D ( 'NONE', #30738, #33906, #38083 ) ;
#11820 = DIRECTION ( 'NONE',  ( 0.000000000000000000, 1.000000000000000000, 0.000000000000000000 ) ) ;
#11822 = ORIENTED_EDGE ( 'NONE', *, *, #26016, .F. ) ;
#11821 = DIRECTION ( 'NONE',  ( 0.000000000000000000, 0.000000000000000000, 1.000000000000000000 ) ) ;
#11823 = CIRCLE ( 'NONE', #18829, 31.99999999999998934 ) ;
#11824 = ORIENTED_EDGE ( 'NONE', *, *, #48016, .F. ) ;
#11825 = ORIENTED_EDGE ( 'NONE', *, *, #33312, .F. ) ;
#11826 = ADVANCED_FACE ( 'NONE', ( #6684 ), #14259, .T. ) ;
#11827 = ORIENTED_EDGE ( 'NONE', *, *, #12906, .F. ) ;
#11828 = EDGE_CURVE ( 'NONE', #48063, #27309, #38860, .T. ) ;
#11829 = ADVANCED_FACE ( 'NONE', ( #10106 ), #17693, .T. ) ;
#11830 = DIRECTION ( 'NONE',  ( 0.000000000000000000, 0.000000000000000000, 1.000000000000000000 ) ) ;
#11831 = CARTESIAN_POINT ( 'NONE',  ( 10.00000000000000000, 10.41901085202135668, -40.68715046381917944 ) ) ;
#11832 = AXIS2_PLACEMENT_3D ( 'NONE', #33507, #14682, #22505 ) ;
#11833 = DIRECTION ( 'NONE',  ( 0.000000000000000000, 0.000000000000000000, 1.000000000000000000 ) ) ;
#11834 = DIRECTION ( 'NONE',  ( -1.000000000000000000, -0.000000000000000000, 0.000000000000000000 ) ) ;
#11835 = VERTEX_POINT ( 'NONE', #28935 ) ;
#11836 = DIRECTION ( 'NONE',  ( 0.000000000000000000, 0.000000000000000000, 1.000000000000000000 ) ) ;
#11837 = ORIENTED_EDGE ( 'NONE', *, *, #42954, .F. ) ;
#11838 = ORIENTED_EDGE ( 'NONE', *, *, #32619, .F. ) ;
#11839 = EDGE_CURVE ( 'NONE', #42002, #10117, #5280, .T. ) ;
#11840 = CARTESIAN_POINT ( 'NONE',  ( -3.000000000000000000, 14.60985201121704513, 18.46759930825707841 ) ) ;
#11841 = LINE ( 'NONE', #8407, #34000 ) ;
#11842 = EDGE_CURVE ( 'NONE', #24088, #30166, #19336, .T. ) ;
#11843 = DIRECTION ( 'NONE',  ( 0.000000000000000000, 0.000000000000000000, 1.000000000000000000 ) ) ;
#11844 = DIRECTION ( 'NONE',  ( 0.000000000000000000, 0.000000000000000000, 1.000000000000000000 ) ) ;
#11845 = ORIENTED_EDGE ( 'NONE', *, *, #3025, .F. ) ;
#11846 = DIRECTION ( 'NONE',  ( -1.000000000000000000, 0.000000000000000000, 0.000000000000000000 ) ) ;
#11847 = CARTESIAN_POINT ( 'NONE',  ( 11.99999999999999822, -59.03342792756297541, 46.54456581323783126 ) ) ;
#11848 = FACE_BOUND ( 'NONE', #16152, .T. ) ;
#11849 = CARTESIAN_POINT ( 'NONE',  ( 0.000000000000000000, -81.96053171279901051, -2.543863470249246195 ) ) ;
#11850 = VECTOR ( 'NONE', #28600, 1000.000000000000000 ) ;
#11851 = CARTESIAN_POINT ( 'NONE',  ( 0.000000000000000000, -70.53064760720297954, -26.01480285779911839 ) ) ;
#11852 = DIRECTION ( 'NONE',  ( -1.000000000000000000, -0.000000000000000000, 0.000000000000000000 ) ) ;
#11853 = DIRECTION ( 'NONE',  ( 0.000000000000000000, 0.000000000000000000, 1.000000000000000000 ) ) ;
#11854 = CARTESIAN_POINT ( 'NONE',  ( 0.000000000000000000, -3.948201729842038432, -23.21447184625298021 ) ) ;
#11855 = ADVANCED_FACE ( 'NONE', ( #36 ), #14993, .T. ) ;
#11856 = DIRECTION ( 'NONE',  ( 0.000000000000000000, 0.1564344650402312020, -0.9876883405951376593 ) ) ;
#11857 = DIRECTION ( 'NONE',  ( 0.000000000000000000, -0.1564344650402170744, -0.9876883405951398798 ) ) ;
#11858 = DIRECTION ( 'NONE',  ( -1.000000000000000000, 0.000000000000000000, 0.000000000000000000 ) ) ;
#11859 = VECTOR ( 'NONE', #45685, 1000.000000000000000 ) ;
#11860 = DIRECTION ( 'NONE',  ( 0.000000000000000000, 0.000000000000000000, 1.000000000000000000 ) ) ;
#11861 = CARTESIAN_POINT ( 'NONE',  ( -2.977765906491215642, 0.000000000000000000, 0.000000000000000000 ) ) ;
#11862 = AXIS2_PLACEMENT_3D ( 'NONE', #44878, #15742, #18680 ) ;
#11863 = DIRECTION ( 'NONE',  ( 0.000000000000000000, 0.9510565162951544194, -0.3090169943749446757 ) ) ;
#11864 = ORIENTED_EDGE ( 'NONE', *, *, #36579, .T. ) ;
#11865 = VECTOR ( 'NONE', #46323, 1000.000000000000000 ) ;
#11866 = AXIS2_PLACEMENT_3D ( 'NONE', #36810, #3274, #10149 ) ;
#11867 = AXIS2_PLACEMENT_3D ( 'NONE', #31927, #16493, #42434 ) ;
#11868 = DIRECTION ( 'NONE',  ( -1.000000000000000000, 0.000000000000000000, 0.000000000000000000 ) ) ;
#11869 = CIRCLE ( 'NONE', #27492, 37.49900000000000233 ) ;
#11870 = ORIENTED_EDGE ( 'NONE', *, *, #15708, .T. ) ;
#11871 = EDGE_CURVE ( 'NONE', #962, #12545, #44838, .T. ) ;
#11872 = ORIENTED_EDGE ( 'NONE', *, *, #41610, .F. ) ;
#11873 = EDGE_CURVE ( 'NONE', #42556, #28383, #4512, .T. ) ;
#11874 = ORIENTED_EDGE ( 'NONE', *, *, #45631, .T. ) ;
#11875 = ORIENTED_EDGE ( 'NONE', *, *, #20289, .T. ) ;
#11876 = FACE_OUTER_BOUND ( 'NONE', #34510, .T. ) ;
#11877 = VERTEX_POINT ( 'NONE', #26726 ) ;
#11878 = EDGE_CURVE ( 'NONE', #9789, #25227, #1364, .T. ) ;
#11879 = CARTESIAN_POINT ( 'NONE',  ( 0.000000000000000000, 0.000000000000000000, 0.000000000000000000 ) ) ;
#11880 = VERTEX_POINT ( 'NONE', #14749 ) ;
#11881 = LINE ( 'NONE', #26805, #31229 ) ;
#11882 = CARTESIAN_POINT ( 'NONE',  ( 0.000000000000000000, 0.000000000000000000, 0.000000000000000000 ) ) ;
#11883 = ORIENTED_EDGE ( 'NONE', *, *, #13319, .F. ) ;
#11884 = DIRECTION ( 'NONE',  ( 0.000000000000000000, -0.7071067811865389130, -0.7071067811865562325 ) ) ;
#11885 = VERTEX_POINT ( 'NONE', #23293 ) ;
#11886 = ORIENTED_EDGE ( 'NONE', *, *, #40599, .T. ) ;
#11887 = EDGE_CURVE ( 'NONE', #48421, #41493, #23051, .T. ) ;
#11888 = EDGE_CURVE ( 'NONE', #18503, #22588, #10757, .T. ) ;
#11889 = CARTESIAN_POINT ( 'NONE',  ( 10.00000000000000000, -4.992566952385247170, 37.16516213103275845 ) ) ;
#11890 = DIRECTION ( 'NONE',  ( -1.000000000000000000, -0.000000000000000000, 0.000000000000000000 ) ) ;
#11891 = AXIS2_PLACEMENT_3D ( 'NONE', #32672, #36351, #13595 ) ;
#11892 = ORIENTED_EDGE ( 'NONE', *, *, #562, .F. ) ;
#11893 = ORIENTED_EDGE ( 'NONE', *, *, #21558, .F. ) ;
#11894 = ORIENTED_EDGE ( 'NONE', *, *, #9995, .T. ) ;
#11895 = DIRECTION ( 'NONE',  ( -1.000000000000000000, 0.000000000000000000, 0.000000000000000000 ) ) ;
#11896 = ORIENTED_EDGE ( 'NONE', *, *, #44815, .F. ) ;
#11897 = CIRCLE ( 'NONE', #944, 16.00000000000000000 ) ;
#11898 = CARTESIAN_POINT ( 'NONE',  ( 11.99999999999999822, 26.01480285779837232, 70.53064760720326376 ) ) ;
#11899 = CARTESIAN_POINT ( 'NONE',  ( 0.000000000000000000, 0.000000000000000000, 0.000000000000000000 ) ) ;
#11900 = CARTESIAN_POINT ( 'NONE',  ( 0.000000000000000000, 18.89407956138362010, -75.16055320797013906 ) ) ;
#11901 = DIRECTION ( 'NONE',  ( -1.000000000000000000, 0.000000000000000000, 0.000000000000000000 ) ) ;
#11902 = CARTESIAN_POINT ( 'NONE',  ( 10.00000000000000000, 0.000000000000000000, 0.000000000000000000 ) ) ;
#11903 = DIRECTION ( 'NONE',  ( 0.000000000000000000, 0.000000000000000000, 1.000000000000000000 ) ) ;
#11904 = AXIS2_PLACEMENT_3D ( 'NONE', #31245, #17017, #32442 ) ;
#11905 = DIRECTION ( 'NONE',  ( -1.000000000000000000, 0.000000000000000000, 0.000000000000000000 ) ) ;
#11906 = FACE_OUTER_BOUND ( 'NONE', #40837, .T. ) ;
#11908 = EDGE_CURVE ( 'NONE', #23982, #6451, #18876, .T. ) ;
#11907 = CARTESIAN_POINT ( 'NONE',  ( 10.00000000000000000, 11.30684508768339569, 76.66974797899841576 ) ) ;
#11909 = EDGE_LOOP ( 'NONE', ( #12309, #44039, #9170, #14727 ) ) ;
#11910 = DIRECTION ( 'NONE',  ( 0.000000000000000000, 0.000000000000000000, 1.000000000000000000 ) ) ;
#11911 = CARTESIAN_POINT ( 'NONE',  ( 0.000000000000000000, 41.76106447765580043, -62.50884508063379741 ) ) ;
#11912 = ORIENTED_EDGE ( 'NONE', *, *, #21857, .F. ) ;
#11913 = DIRECTION ( 'NONE',  ( 0.9730327541852497042, -0.2306669878475622604, 0.000000000000000000 ) ) ;
#11914 = AXIS2_PLACEMENT_3D ( 'NONE', #29010, #7706, #22631 ) ;
#11915 = CARTESIAN_POINT ( 'NONE',  ( 10.00000000000000000, 37.58145647212453611, 0.6853352020791767529 ) ) ;
#11916 = CARTESIAN_POINT ( 'NONE',  ( 0.000000000000000000, -40.98264845739743123, -9.188173127307734944 ) ) ;
#11917 = LINE ( 'NONE', #1622, #47933 ) ;
#11918 = AXIS2_PLACEMENT_3D ( 'NONE', #46230, #43284, #39625 ) ;
#11919 = CARTESIAN_POINT ( 'NONE',  ( 0.000000000000000000, 65.59268652807263322, -36.72794159290169347 ) ) ;
#11920 = CARTESIAN_POINT ( 'NONE',  ( -23.30023580412278505, -123.4057321492263384, 5.500000000000000000 ) ) ;
#11921 = ORIENTED_EDGE ( 'NONE', *, *, #10370, .T. ) ;
#11922 = DIRECTION ( 'NONE',  ( -1.000000000000000000, 0.000000000000000000, 0.000000000000000000 ) ) ;
#11923 = CARTESIAN_POINT ( 'NONE',  ( 0.000000000000000000, -36.13751322684404244, -21.40280677340410165 ) ) ;
#11924 = VECTOR ( 'NONE', #45018, 1000.000000000000000 ) ;
#11925 = ORIENTED_EDGE ( 'NONE', *, *, #893, .F. ) ;
#11926 = SURFACE_STYLE_USAGE ( .BOTH. , #26380 ) ;
#11927 = DIRECTION ( 'NONE',  ( -1.000000000000000000, -0.000000000000000000, 0.000000000000000000 ) ) ;
#11928 = EDGE_LOOP ( 'NONE', ( #41881, #8130, #25838, #10242 ) ) ;
#11929 = EDGE_CURVE ( 'NONE', #20488, #14224, #39671, .T. ) ;
#11930 = AXIS2_PLACEMENT_3D ( 'NONE', #31689, #27037, #16740 ) ;
#11931 = VECTOR ( 'NONE', #11311, 1000.000000000000114 ) ;
#11932 = EDGE_CURVE ( 'NONE', #23907, #14963, #33578, .T. ) ;
#11933 = VERTEX_POINT ( 'NONE', #11564 ) ;
#11934 = EDGE_CURVE ( 'NONE', #20915, #36021, #41416, .T. ) ;
#11935 = ORIENTED_EDGE ( 'NONE', *, *, #36564, .T. ) ;
#11936 = DIRECTION ( 'NONE',  ( -1.000000000000000000, -0.000000000000000000, 0.000000000000000000 ) ) ;
#11937 = CARTESIAN_POINT ( 'NONE',  ( 0.000000000000000000, 0.000000000000000000, 125.0000000000000000 ) ) ;
#11938 = VERTEX_POINT ( 'NONE', #4462 ) ;
#11939 = EDGE_CURVE ( 'NONE', #14587, #43833, #43568, .T. ) ;
#11940 = AXIS2_PLACEMENT_3D ( 'NONE', #38520, #37549, #4279 ) ;
#11941 = VECTOR ( 'NONE', #17014, 1000.000000000000000 ) ;
#11942 = DIRECTION ( 'NONE',  ( 0.000000000000000000, 0.000000000000000000, 1.000000000000000000 ) ) ;
#11943 = VECTOR ( 'NONE', #14086, 1000.000000000000000 ) ;
#11944 = ORIENTED_EDGE ( 'NONE', *, *, #47314, .T. ) ;
#11945 = ORIENTED_EDGE ( 'NONE', *, *, #32980, .F. ) ;
#11946 = ADVANCED_FACE ( 'NONE', ( #37497 ), #762, .T. ) ;
#11947 = EDGE_CURVE ( 'NONE', #40215, #10055, #38119, .T. ) ;
#11948 = DIRECTION ( 'NONE',  ( -1.000000000000000000, -0.000000000000000000, -0.000000000000000000 ) ) ;
#11950 = ORIENTED_EDGE ( 'NONE', *, *, #38645, .F. ) ;
#11949 = LINE ( 'NONE', #4599, #28174 ) ;
#11951 = DIRECTION ( 'NONE',  ( -1.000000000000000000, 0.000000000000000000, 0.000000000000000000 ) ) ;
#11952 = ORIENTED_EDGE ( 'NONE', *, *, #21753, .F. ) ;
#11953 = LINE ( 'NONE', #42055, #32548 ) ;
#11954 = EDGE_CURVE ( 'NONE', #40825, #32445, #6842, .T. ) ;
#11955 = ORIENTED_EDGE ( 'NONE', *, *, #3191, .T. ) ;
#11956 = EDGE_LOOP ( 'NONE', ( #15607, #27327, #38008, #9466, #2950, #9343, #23736, #1903, #44795, #10582, #8551, #34313, #19596, #44265, #892, #9184 ) ) ;
#11957 = CYLINDRICAL_SURFACE ( 'NONE', #44713, 77.49899999999999523 ) ;
#11958 = LINE ( 'NONE', #26890, #27587 ) ;
#11959 = VECTOR ( 'NONE', #18891, 1000.000000000000114 ) ;
#11960 = PLANE ( 'NONE',  #15842 ) ;
#11961 = VERTEX_POINT ( 'NONE', #30169 ) ;
#11962 = ORIENTED_EDGE ( 'NONE', *, *, #17729, .F. ) ;
#11963 = VECTOR ( 'NONE', #35514, 1000.000000000000000 ) ;
#11964 = EDGE_CURVE ( 'NONE', #45199, #44962, #45091, .T. ) ;
#11965 = FACE_OUTER_BOUND ( 'NONE', #20160, .T. ) ;
#11966 = AXIS2_PLACEMENT_3D ( 'NONE', #13465, #5897, #27939 ) ;
#11967 = ORIENTED_EDGE ( 'NONE', *, *, #5377, .T. ) ;
#11968 = DIRECTION ( 'NONE',  ( -1.000000000000000000, 0.000000000000000000, -0.000000000000000000 ) ) ;
#11969 = ORIENTED_EDGE ( 'NONE', *, *, #3609, .F. ) ;
#11970 = AXIS2_PLACEMENT_3D ( 'NONE', #42238, #34636, #1118 ) ;
#11971 = CARTESIAN_POINT ( 'NONE',  ( 0.000000000000000000, -67.80270845531921964, 46.11716303203162681 ) ) ;
#11972 = DIRECTION ( 'NONE',  ( 0.000000000000000000, 0.000000000000000000, 1.000000000000000000 ) ) ;
#11973 = CIRCLE ( 'NONE', #8803, 77.49900000000000944 ) ;
#11974 = PLANE ( 'NONE',  #21630 ) ;
#11975 = DIRECTION ( 'NONE',  ( -1.000000000000000000, -0.000000000000000000, -0.000000000000000000 ) ) ;
#11976 = CARTESIAN_POINT ( 'NONE',  ( 10.00000000000000000, -35.38097989696520074, 12.42422080174625520 ) ) ;
#11977 = DIRECTION ( 'NONE',  ( -1.000000000000000000, 0.000000000000000000, 0.000000000000000000 ) ) ;
#11978 = AXIS2_PLACEMENT_3D ( 'NONE', #1198, #38400, #23704 ) ;
#11979 = DIRECTION ( 'NONE',  ( 0.000000000000000000, -0.8660254037844432595, -0.4999999999999919509 ) ) ;
#11980 = AXIS2_PLACEMENT_3D ( 'NONE', #20883, #28217, #13294 ) ;
#11981 = CARTESIAN_POINT ( 'NONE',  ( 10.00000000000000000, 5.256550761632864166, 77.32052557432842832 ) ) ;
#11982 = DIRECTION ( 'NONE',  ( -1.000000000000000000, -0.000000000000000000, 0.000000000000000000 ) ) ;
#11983 = ORIENTED_EDGE ( 'NONE', *, *, #15154, .F. ) ;
#11984 = VECTOR ( 'NONE', #38792, 1000.000000000000000 ) ;
#11985 = CARTESIAN_POINT ( 'NONE',  ( 10.00000000000000000, -30.00120703465189465, -22.64427369931201639 ) ) ;
#11986 = CARTESIAN_POINT ( 'NONE',  ( -24.94940289813038703, -237.3777120880567963, -5.500000000000000000 ) ) ;
#11987 = CARTESIAN_POINT ( 'NONE',  ( 5.000000000000000000, 15.48615015657637706, -39.04073710021327770 ) ) ;
#11988 = VERTEX_POINT ( 'NONE', #12047 ) ;
#11989 = UNCERTAINTY_MEASURE_WITH_UNIT (LENGTH_MEASURE( 1.000000000000000082E-05 ), #4101, 'distance_accuracy_value', 'NONE');
#11990 = DIRECTION ( 'NONE',  ( 0.000000000000000000, 0.9135454576426063067, -0.4067366430757881068 ) ) ;
#11991 = ADVANCED_FACE ( 'NONE', ( #540 ), #15471, .F. ) ;
#11992 = DIRECTION ( 'NONE',  ( -1.000000000000000000, -0.000000000000000000, -0.000000000000000000 ) ) ;
#11993 = AXIS2_PLACEMENT_3D ( 'NONE', #33525, #14698, #30356 ) ;
#11994 = DIRECTION ( 'NONE',  ( 0.000000000000000000, 0.000000000000000000, -1.000000000000000000 ) ) ;
#11995 = EDGE_CURVE ( 'NONE', #28510, #46631, #8364, .T. ) ;
#11996 = VERTEX_POINT ( 'NONE', #5415 ) ;
#11997 = EDGE_CURVE ( 'NONE', #5001, #4198, #24041, .T. ) ;
#11998 = CIRCLE ( 'NONE', #47921, 82.00000000000000000 ) ;
#12000 = ORIENTED_EDGE ( 'NONE', *, *, #2640, .F. ) ;
#11999 = EDGE_CURVE ( 'NONE', #48421, #29406, #35023, .T. ) ;
#12001 = EDGE_CURVE ( 'NONE', #11302, #46719, #38462, .T. ) ;
#12002 = CARTESIAN_POINT ( 'NONE',  ( 0.000000000000000000, 72.35160999960817207, 20.41045688087850607 ) ) ;
#12003 = VECTOR ( 'NONE', #43923, 1000.000000000000000 ) ;
#12004 = CIRCLE ( 'NONE', #18233, 82.00000000000000000 ) ;
#12006 = ORIENTED_EDGE ( 'NONE', *, *, #31522, .F. ) ;
#12005 = CIRCLE ( 'NONE', #40938, 16.00000000000000355 ) ;
#12007 = ORIENTED_EDGE ( 'NONE', *, *, #43005, .F. ) ;
#12008 = ORIENTED_EDGE ( 'NONE', *, *, #6951, .T. ) ;
#12009 = EDGE_LOOP ( 'NONE', ( #6571, #12741, #27802, #25695 ) ) ;
#12010 = AXIS2_PLACEMENT_3D ( 'NONE', #8961, #881, #35138 ) ;
#12011 = DIRECTION ( 'NONE',  ( 0.000000000000000000, 0.000000000000000000, 1.000000000000000000 ) ) ;
#12012 = ORIENTED_EDGE ( 'NONE', *, *, #13426, .T. ) ;
#12013 = AXIS2_PLACEMENT_3D ( 'NONE', #15528, #23115, #19420 ) ;
#12014 = VERTEX_POINT ( 'NONE', #20325 ) ;
#12015 = DIRECTION ( 'NONE',  ( -1.000000000000000000, 0.000000000000000000, 0.000000000000000000 ) ) ;
#12016 = ADVANCED_FACE ( 'NONE', ( #46540 ), #1744, .T. ) ;
#12017 = ORIENTED_EDGE ( 'NONE', *, *, #13926, .F. ) ;
#12018 = AXIS2_PLACEMENT_3D ( 'NONE', #39904, #32319, #28160 ) ;
#12019 = DIRECTION ( 'NONE',  ( 0.000000000000000000, 0.000000000000000000, -1.000000000000000000 ) ) ;
#12020 = VECTOR ( 'NONE', #3499, 1000.000000000000000 ) ;
#12021 = ORIENTED_EDGE ( 'NONE', *, *, #12830, .F. ) ;
#12022 = FACE_OUTER_BOUND ( 'NONE', #45789, .T. ) ;
#12023 = DIRECTION ( 'NONE',  ( 0.000000000000000000, 0.8090169943749445647, 0.5877852522924770229 ) ) ;
#12025 = EDGE_LOOP ( 'NONE', ( #5930, #35363, #45987, #1111 ) ) ;
#12024 = CIRCLE ( 'NONE', #4952, 30.50000000000000000 ) ;
#12026 = PLANE ( 'NONE',  #877 ) ;
#12027 = VERTEX_POINT ( 'NONE', #45818 ) ;
#12029 = ORIENTED_EDGE ( 'NONE', *, *, #40303, .T. ) ;
#12028 = DIRECTION ( 'NONE',  ( 1.000000000000000000, -0.000000000000000000, -0.000000000000000000 ) ) ;
#12030 = EDGE_CURVE ( 'NONE', #41330, #12321, #45145, .T. ) ;
#12031 = DIRECTION ( 'NONE',  ( 0.000000000000000000, 0.000000000000000000, 1.000000000000000000 ) ) ;
#12032 = ORIENTED_EDGE ( 'NONE', *, *, #36373, .T. ) ;
#12033 = CARTESIAN_POINT ( 'NONE',  ( 23.41451323550360186, -132.5004227906269989, -5.500000000000000000 ) ) ;
#12034 = ORIENTED_EDGE ( 'NONE', *, *, #6000, .T. ) ;
#12035 = VERTEX_POINT ( 'NONE', #19842 ) ;
#12036 = CARTESIAN_POINT ( 'NONE',  ( -7.572224309238338336, -145.4393675041377492, 5.500000000000000000 ) ) ;
#12037 = DIRECTION ( 'NONE',  ( 0.000000000000000000, 0.9135454576426055295, 0.4067366430757899387 ) ) ;
#12038 = DIRECTION ( 'NONE',  ( -1.000000000000000000, 0.000000000000000000, 0.000000000000000000 ) ) ;
#12039 = CARTESIAN_POINT ( 'NONE',  ( 11.99999999999999822, -75.11725578898470701, 2.956366410620372864 ) ) ;
#12040 = DIRECTION ( 'NONE',  ( -0.9038112904824853189, 0.4279312458752976833, 0.000000000000000000 ) ) ;
#12041 = FACE_OUTER_BOUND ( 'NONE', #46715, .T. ) ;
#12042 = CARTESIAN_POINT ( 'NONE',  ( 10.00000000000000000, 35.38097989696512968, 12.42422080174651100 ) ) ;
#12043 = DIRECTION ( 'NONE',  ( 0.000000000000000000, 0.000000000000000000, 1.000000000000000000 ) ) ;
#12044 = EDGE_CURVE ( 'NONE', #24231, #38560, #12292, .T. ) ;
#12045 = AXIS2_PLACEMENT_3D ( 'NONE', #13289, #1552, #9597 ) ;
#12046 = DIRECTION ( 'NONE',  ( 0.000000000000000000, 0.000000000000000000, 1.000000000000000000 ) ) ;
#12047 = CARTESIAN_POINT ( 'NONE',  ( 11.99999999999999822, -44.88180994100329713, -63.18004540533077318 ) ) ;
#12048 = DIRECTION ( 'NONE',  ( 0.000000000000000000, 0.000000000000000000, 1.000000000000000000 ) ) ;
#12049 = VERTEX_POINT ( 'NONE', #13014 ) ;
#12050 = AXIS2_PLACEMENT_3D ( 'NONE', #4619, #3654, #11495 ) ;
#12051 = CIRCLE ( 'NONE', #39393, 82.00000000000000000 ) ;
#12052 = VECTOR ( 'NONE', #13858, 1000.000000000000000 ) ;
#12053 = CARTESIAN_POINT ( 'NONE',  ( 0.000000000000000000, -0.8299999999999999600, 0.000000000000000000 ) ) ;
#12054 = CYLINDRICAL_SURFACE ( 'NONE', #36318, 82.00000000000000000 ) ;
#12055 =( NAMED_UNIT ( * ) SI_UNIT ( $, .STERADIAN. ) SOLID_ANGLE_UNIT ( ) );
#12056 = CARTESIAN_POINT ( 'NONE',  ( 11.99999999999999822, -81.34940948281344220, 10.30890764327355491 ) ) ;
#12057 = VERTEX_POINT ( 'NONE', #46058 ) ;
#12058 = EDGE_CURVE ( 'NONE', #19561, #19028, #34782, .T. ) ;
#12059 = ORIENTED_EDGE ( 'NONE', *, *, #11684, .T. ) ;
#12061 = FACE_BOUND ( 'NONE', #4445, .T. ) ;
#12060 = VECTOR ( 'NONE', #17090, 1000.000000000000114 ) ;
#12062 = CIRCLE ( 'NONE', #5014, 42.00000000000000000 ) ;
#12063 = ORIENTED_EDGE ( 'NONE', *, *, #13856, .F. ) ;
#12064 = AXIS2_PLACEMENT_3D ( 'NONE', #36927, #33993, #47951 ) ;
#12065 = EDGE_CURVE ( 'NONE', #14287, #46808, #34967, .T. ) ;
#12066 = LINE ( 'NONE', #1016, #40880 ) ;
#12067 = VECTOR ( 'NONE', #33528, 1000.000000000000000 ) ;
#12068 = CIRCLE ( 'NONE', #8009, 16.00000000000000000 ) ;
#12069 = APPLICATION_PROTOCOL_DEFINITION ( 'draft international standard', 'automotive_design', 1998, #12581 ) ;
#12070 = CARTESIAN_POINT ( 'NONE',  ( -3.000000000000000000, 26.50000000000000000, -1.500000000000001332 ) ) ;
#12071 = AXIS2_PLACEMENT_3D ( 'NONE', #31651, #24522, #35544 ) ;
#12072 = EDGE_LOOP ( 'NONE', ( #41112, #43962, #8231, #7445 ) ) ;
#12073 = EDGE_CURVE ( 'NONE', #35339, #32597, #20100, .T. ) ;
#12074 = EDGE_CURVE ( 'NONE', #16579, #7278, #23262, .T. ) ;
#12075 = CARTESIAN_POINT ( 'NONE',  ( 6.938893903907228378E-15, 0.000000000000000000, 0.000000000000000000 ) ) ;
#12076 = ORIENTED_EDGE ( 'NONE', *, *, #2373, .F. ) ;
#12077 = VECTOR ( 'NONE', #21765, 1000.000000000000000 ) ;
#12078 = DIRECTION ( 'NONE',  ( -0.7071067811865474617, 0.000000000000000000, 0.7071067811865474617 ) ) ;
#12079 = CARTESIAN_POINT ( 'NONE',  ( 10.00000000000000000, -12.42422080174663712, 35.38097989696507994 ) ) ;
#12080 = AXIS2_PLACEMENT_3D ( 'NONE', #8040, #22978, #45486 ) ;
#12082 = ORIENTED_EDGE ( 'NONE', *, *, #7528, .T. ) ;
#12081 = DIRECTION ( 'NONE',  ( 0.000000000000000000, -0.8526401643540970632, 0.5224985647159410274 ) ) ;
#12083 = AXIS2_PLACEMENT_3D ( 'NONE', #22348, #2514, #17446 ) ;
#12084 = ORIENTED_EDGE ( 'NONE', *, *, #17413, .T. ) ;
#12085 = CIRCLE ( 'NONE', #39440, 31.99999999999998579 ) ;
#12086 = DIRECTION ( 'NONE',  ( 0.000000000000000000, 0.000000000000000000, 1.000000000000000000 ) ) ;
#12087 = DIRECTION ( 'NONE',  ( 0.000000000000000000, 0.000000000000000000, 1.000000000000000000 ) ) ;
#12088 = CARTESIAN_POINT ( 'NONE',  ( 4.999999999999999112, -40.98264845739743123, -9.188173127307734944 ) ) ;
#12089 = DIRECTION ( 'NONE',  ( -1.000000000000000000, 0.000000000000000000, 0.000000000000000000 ) ) ;
#12090 = AXIS2_PLACEMENT_3D ( 'NONE', #47622, #3313, #14106 ) ;
#12091 = AXIS2_PLACEMENT_3D ( 'NONE', #4692, #15710, #45095 ) ;
#12092 = ORIENTED_EDGE ( 'NONE', *, *, #18944, .T. ) ;
#12093 = CARTESIAN_POINT ( 'NONE',  ( 0.000000000000000000, 0.000000000000000000, 0.000000000000000000 ) ) ;
#12094 = VERTEX_POINT ( 'NONE', #31378 ) ;
#12095 = VERTEX_POINT ( 'NONE', #42376 ) ;
#12096 = CIRCLE ( 'NONE', #37089, 77.49900000000000944 ) ;
#12097 = DIRECTION ( 'NONE',  ( -1.000000000000000000, 0.000000000000000000, 0.000000000000000000 ) ) ;
#12098 = AXIS2_PLACEMENT_3D ( 'NONE', #25641, #47445, #40583 ) ;
#12099 = DIRECTION ( 'NONE',  ( -1.000000000000000000, -0.000000000000000000, 0.000000000000000000 ) ) ;
#12100 = CARTESIAN_POINT ( 'NONE',  ( 23.49916127795269105, -121.5130826919798039, -2.500000000000000000 ) ) ;
#12101 = LINE ( 'NONE', #30216, #42260 ) ;
#12102 = ORIENTED_EDGE ( 'NONE', *, *, #11357, .F. ) ;
#12103 = CARTESIAN_POINT ( 'NONE',  ( 23.30762065077924916, -123.0008031590507329, 2.500000000000000000 ) ) ;
#12104 = AXIS2_PLACEMENT_3D ( 'NONE', #34242, #27643, #15899 ) ;
#12105 = DIRECTION ( 'NONE',  ( 1.000000000000000000, 0.000000000000000000, 0.000000000000000000 ) ) ;
#12106 = DIRECTION ( 'NONE',  ( -1.000000000000000000, -0.000000000000000000, -0.000000000000000000 ) ) ;
#12107 = FACE_OUTER_BOUND ( 'NONE', #23588, .T. ) ;
#12108 = CARTESIAN_POINT ( 'NONE',  ( -11.99999999999999645, 0.000000000000000000, 0.000000000000000000 ) ) ;
#12109 = EDGE_CURVE ( 'NONE', #38735, #47410, #24248, .T. ) ;
#12110 = DIRECTION ( 'NONE',  ( 0.000000000000000000, 1.000000000000000000, 1.301042606982602757E-15 ) ) ;
#12111 = CARTESIAN_POINT ( 'NONE',  ( 23.49916127795269460, -121.5130826919798039, 5.500000000000000000 ) ) ;
#12112 = CYLINDRICAL_SURFACE ( 'NONE', #20824, 16.00000000000000000 ) ;
#12113 = DIRECTION ( 'NONE',  ( 1.000000000000000000, -0.000000000000000000, -0.000000000000000000 ) ) ;
#12114 = DIRECTION ( 'NONE',  ( 1.000000000000000000, -0.000000000000000000, -0.000000000000000000 ) ) ;
#12115 = ORIENTED_EDGE ( 'NONE', *, *, #22979, .T. ) ;
#12116 = DIRECTION ( 'NONE',  ( -1.000000000000000000, -0.000000000000000000, -0.000000000000000000 ) ) ;
#12117 = EDGE_LOOP ( 'NONE', ( #30264, #30142, #27790, #46096 ) ) ;
#12118 = EDGE_CURVE ( 'NONE', #38854, #5281, #38723, .T. ) ;
#12119 = CIRCLE ( 'NONE', #26957, 77.49900000000002365 ) ;
#12120 = FACE_OUTER_BOUND ( 'NONE', #40247, .T. ) ;
#12121 = LINE ( 'NONE', #830, #33957 ) ;
#12122 = ORIENTED_EDGE ( 'NONE', *, *, #3914, .F. ) ;
#12123 = VERTEX_POINT ( 'NONE', #24024 ) ;
#12124 = EDGE_CURVE ( 'NONE', #47625, #19393, #38958, .T. ) ;
#12125 = AXIS2_PLACEMENT_3D ( 'NONE', #28129, #14344, #47619 ) ;
#12126 = AXIS2_PLACEMENT_3D ( 'NONE', #18657, #34070, #15481 ) ;
#12127 = EDGE_CURVE ( 'NONE', #32836, #43777, #4687, .T. ) ;
#12128 = CARTESIAN_POINT ( 'NONE',  ( -2.981742216678212820, 0.000000000000000000, -15.39727592608509177 ) ) ;
#12129 = ORIENTED_EDGE ( 'NONE', *, *, #20536, .T. ) ;
#12130 = CIRCLE ( 'NONE', #31664, 31.99999999999998934 ) ;
#12131 = EDGE_CURVE ( 'NONE', #10568, #28195, #6092, .T. ) ;
#12132 = VERTEX_POINT ( 'NONE', #37625 ) ;
#12133 = ORIENTED_EDGE ( 'NONE', *, *, #31085, .T. ) ;
#12134 = VECTOR ( 'NONE', #27682, 1000.000000000000000 ) ;
#12136 = EDGE_CURVE ( 'NONE', #16743, #31838, #4098, .T. ) ;
#12135 = ORIENTED_EDGE ( 'NONE', *, *, #1501, .F. ) ;
#12137 = CARTESIAN_POINT ( 'NONE',  ( 11.99999999999999822, -56.15606465354916566, -59.75363087400133111 ) ) ;
#12138 = ORIENTED_EDGE ( 'NONE', *, *, #30862, .F. ) ;
#12139 = AXIS2_PLACEMENT_3D ( 'NONE', #39293, #15819, #30752 ) ;
#12140 = CARTESIAN_POINT ( 'NONE',  ( 10.00000000000000000, 59.75363087400152295, -56.15606465354897381 ) ) ;
#12141 = DIRECTION ( 'NONE',  ( -1.000000000000000000, 0.000000000000000000, -0.000000000000000000 ) ) ;
#12142 = LINE ( 'NONE', #4054, #7398 ) ;
#12143 = EDGE_CURVE ( 'NONE', #39399, #6463, #38901, .T. ) ;
#12144 = ORIENTED_EDGE ( 'NONE', *, *, #12620, .F. ) ;
#12145 = CARTESIAN_POINT ( 'NONE',  ( 0.000000000000000000, -120.0000000000000000, -40.00000000000000711 ) ) ;
#12146 = AXIS2_PLACEMENT_3D ( 'NONE', #28402, #29372, #2448 ) ;
#12147 = ORIENTED_EDGE ( 'NONE', *, *, #10129, .F. ) ;
#12148 = ORIENTED_EDGE ( 'NONE', *, *, #43818, .F. ) ;
#12149 = CARTESIAN_POINT ( 'NONE',  ( 0.000000000000000000, 33.00180498840072829, -17.80606268964504935 ) ) ;
#12150 = CARTESIAN_POINT ( 'NONE',  ( 0.000000000000000000, 59.75363087400153006, -56.15606465354896670 ) ) ;
#12151 = AXIS2_PLACEMENT_3D ( 'NONE', #1065, #11852, #27512 ) ;
#12152 = VERTEX_POINT ( 'NONE', #11923 ) ;
#12153 = ORIENTED_EDGE ( 'NONE', *, *, #9889, .T. ) ;
#12154 = FACE_OUTER_BOUND ( 'NONE', #27805, .T. ) ;
#12155 = VERTEX_POINT ( 'NONE', #42032 ) ;
#12156 = CIRCLE ( 'NONE', #1986, 77.49900000000000944 ) ;
#12157 = DIRECTION ( 'NONE',  ( -1.000000000000000000, 0.000000000000000000, 0.000000000000000000 ) ) ;
#12158 = DIRECTION ( 'NONE',  ( 1.000000000000000000, 0.000000000000000000, -0.000000000000000000 ) ) ;
#12159 = DIRECTION ( 'NONE',  ( -1.000000000000000000, 0.000000000000000000, 0.000000000000000000 ) ) ;
#12160 = CARTESIAN_POINT ( 'NONE',  ( 10.00000000000000000, -55.38113227695820484, 54.21277698773656084 ) ) ;
#12161 = CYLINDRICAL_SURFACE ( 'NONE', #44667, 77.49899999999999523 ) ;
#12162 = CARTESIAN_POINT ( 'NONE',  ( 0.000000000000000000, 0.000000000000000000, 42.00000000000001421 ) ) ;
#12163 = CYLINDRICAL_SURFACE ( 'NONE', #8135, 82.00000000000000000 ) ;
#12164 = DIRECTION ( 'NONE',  ( 0.000000000000000000, -0.7071067811865535679, 0.7071067811865414665 ) ) ;
#12165 = CYLINDRICAL_SURFACE ( 'NONE', #18900, 77.49899999999999523 ) ;
#12166 = CARTESIAN_POINT ( 'NONE',  ( 11.99999999999999822, -55.20638768913724448, -51.02545421589383068 ) ) ;
#12167 = ADVANCED_FACE ( 'NONE', ( #27573 ), #45218, .T. ) ;
#12168 = VECTOR ( 'NONE', #7899, 1000.000000000000000 ) ;
#12169 = AXIS2_PLACEMENT_3D ( 'NONE', #29156, #36268, #44095 ) ;
#12170 = EDGE_LOOP ( 'NONE', ( #30878, #19740, #36368, #19723 ) ) ;
#12171 = ORIENTED_EDGE ( 'NONE', *, *, #3424, .F. ) ;
#12172 = CARTESIAN_POINT ( 'NONE',  ( 0.000000000000000000, 39.47590169984945163, -71.87247863392373404 ) ) ;
#12173 = EDGE_CURVE ( 'NONE', #26066, #29937, #20119, .T. ) ;
#12174 = AXIS2_PLACEMENT_3D ( 'NONE', #29104, #25430, #33014 ) ;
#12175 = DIRECTION ( 'NONE',  ( 0.000000000000000000, 0.000000000000000000, 1.000000000000000000 ) ) ;
#12176 = FACE_OUTER_BOUND ( 'NONE', #5380, .T. ) ;
#12177 = LINE ( 'NONE', #1387, #15916 ) ;
#12178 = EDGE_CURVE ( 'NONE', #6290, #15060, #22472, .T. ) ;
#12179 = SURFACE_STYLE_FILL_AREA ( #31021 ) ;
#12180 = FACE_OUTER_BOUND ( 'NONE', #33719, .T. ) ;
#12181 = DIRECTION ( 'NONE',  ( 9.814797785686868941E-17, -1.000000000000000000, 0.000000000000000000 ) ) ;
#12182 = DIRECTION ( 'NONE',  ( -1.000000000000000000, 0.000000000000000000, -0.000000000000000000 ) ) ;
#12183 = VECTOR ( 'NONE', #32735, 1000.000000000000000 ) ;
#12184 = EDGE_CURVE ( 'NONE', #15589, #994, #34913, .T. ) ;
#12185 = LINE ( 'NONE', #27110, #47878 ) ;
#12186 = EDGE_CURVE ( 'NONE', #33852, #22252, #16089, .T. ) ;
#12187 = EDGE_CURVE ( 'NONE', #46736, #44017, #23180, .T. ) ;
#12188 = VERTEX_POINT ( 'NONE', #27336 ) ;
#12189 = ORIENTED_EDGE ( 'NONE', *, *, #13061, .T. ) ;
#12190 = LINE ( 'NONE', #38362, #10890 ) ;
#12191 = ORIENTED_EDGE ( 'NONE', *, *, #34361, .T. ) ;
#12192 = PRODUCT_DEFINITION ( 'UNKNOWN', '', #20188, #37447 ) ;
#12193 = ORIENTED_EDGE ( 'NONE', *, *, #38189, .F. ) ;
#12194 = CIRCLE ( 'NONE', #9829, 37.49900000000000233 ) ;
#12195 = CARTESIAN_POINT ( 'NONE',  ( 0.000000000000000000, 18.84667830672605859, -18.68964196561243796 ) ) ;
#12196 = ORIENTED_EDGE ( 'NONE', *, *, #4775, .T. ) ;
#12197 = CIRCLE ( 'NONE', #41899, 42.00000000000000000 ) ;
#12198 = AXIS2_PLACEMENT_3D ( 'NONE', #44887, #11116, #11373 ) ;
#12199 = DIRECTION ( 'NONE',  ( 0.000000000000000000, -0.8090169943749531134, 0.5877852522924653655 ) ) ;
#12201 = ORIENTED_EDGE ( 'NONE', *, *, #42968, .T. ) ;
#12200 = DIRECTION ( 'NONE',  ( 1.000000000000000000, 0.000000000000000000, -0.000000000000000000 ) ) ;
#12202 = CARTESIAN_POINT ( 'NONE',  ( -21.33958957442910886, -129.9559990355020034, 5.500000000000000000 ) ) ;
#12203 = VERTEX_POINT ( 'NONE', #15834 ) ;
#12204 = ORIENTED_EDGE ( 'NONE', *, *, #23063, .F. ) ;
#12205 = FACE_OUTER_BOUND ( 'NONE', #40763, .T. ) ;
#12206 = VERTEX_POINT ( 'NONE', #42257 ) ;
#12207 = ORIENTED_EDGE ( 'NONE', *, *, #33958, .F. ) ;
#12208 = CARTESIAN_POINT ( 'NONE',  ( 12.00000000000000000, 14.60985201121729737, 18.46759930825687235 ) ) ;
#12209 = CYLINDRICAL_SURFACE ( 'NONE', #3789, 31.99999999999998579 ) ;
#12210 = ORIENTED_EDGE ( 'NONE', *, *, #31893, .T. ) ;
#12211 = AXIS2_PLACEMENT_3D ( 'NONE', #42631, #46059, #30894 ) ;
#12212 = CARTESIAN_POINT ( 'NONE',  ( 11.99999999999999822, -46.54456581323847786, 59.03342792756247093 ) ) ;
#12213 = LINE ( 'NONE', #31793, #25210 ) ;
#12214 = AXIS2_PLACEMENT_3D ( 'NONE', #11622, #11858, #26549 ) ;
#12215 = ORIENTED_EDGE ( 'NONE', *, *, #40153, .F. ) ;
#12216 = ORIENTED_EDGE ( 'NONE', *, *, #3922, .T. ) ;
#12217 = DIRECTION ( 'NONE',  ( -0.9227826878668545785, -0.3853207896976533209, 0.000000000000000000 ) ) ;
#12218 = CIRCLE ( 'NONE', #23953, 21.00000000000000000 ) ;
#12219 = PLANE ( 'NONE',  #22759 ) ;
#12220 = EDGE_CURVE ( 'NONE', #19509, #25968, #9983, .T. ) ;
#12221 = ORIENTED_EDGE ( 'NONE', *, *, #2125, .F. ) ;
#12222 = ORIENTED_EDGE ( 'NONE', *, *, #1264, .T. ) ;
#12223 = DIRECTION ( 'NONE',  ( 0.000000000000000000, 0.000000000000000000, 1.000000000000000000 ) ) ;
#12224 = ORIENTED_EDGE ( 'NONE', *, *, #31921, .F. ) ;
#12225 = EDGE_CURVE ( 'NONE', #30064, #46329, #7992, .T. ) ;
#12226 = CYLINDRICAL_SURFACE ( 'NONE', #37105, 31.99999999999998579 ) ;
#12227 = DIRECTION ( 'NONE',  ( 0.000000000000000000, 0.000000000000000000, -1.000000000000000000 ) ) ;
#12228 = CARTESIAN_POINT ( 'NONE',  ( 11.99999999999999822, 81.96053171279901051, 2.543863470248673764 ) ) ;
#12229 = DIRECTION ( 'NONE',  ( -1.000000000000000000, -0.000000000000000000, -0.000000000000000000 ) ) ;
#12230 = CIRCLE ( 'NONE', #3612, 31.99999999999999289 ) ;
#12231 = EDGE_CURVE ( 'NONE', #23219, #30321, #31102, .T. ) ;
#12232 = DIRECTION ( 'NONE',  ( 0.000000000000000000, 0.000000000000000000, 1.000000000000000000 ) ) ;
#12233 = AXIS2_PLACEMENT_3D ( 'NONE', #36621, #14847, #3085 ) ;
#12234 = CARTESIAN_POINT ( 'NONE',  ( 11.99999999999999822, 31.46837873495072913, -68.27212725128242710 ) ) ;
#12235 = DIRECTION ( 'NONE',  ( 0.000000000000000000, 0.000000000000000000, 1.000000000000000000 ) ) ;
#12236 = CIRCLE ( 'NONE', #30191, 37.49900000000000944 ) ;
#12237 = DIRECTION ( 'NONE',  ( -1.000000000000000000, 0.000000000000000000, 0.000000000000000000 ) ) ;
#12238 = CARTESIAN_POINT ( 'NONE',  ( 0.000000000000000000, 0.000000000000000000, 12.50000000000000000 ) ) ;
#12239 = ADVANCED_FACE ( 'NONE', ( #30767 ), #5066, .T. ) ;
#12240 = EDGE_CURVE ( 'NONE', #31605, #43990, #41543, .T. ) ;
#12241 = ORIENTED_EDGE ( 'NONE', *, *, #38770, .F. ) ;
#12242 = VERTEX_POINT ( 'NONE', #15369 ) ;
#12243 = AXIS2_PLACEMENT_3D ( 'NONE', #42564, #19775, #41837 ) ;
#12244 = FACE_OUTER_BOUND ( 'NONE', #43972, .T. ) ;
#12245 = VERTEX_POINT ( 'NONE', #33941 ) ;
#12246 = DIRECTION ( 'NONE',  ( 0.000000000000000000, 0.000000000000000000, 1.000000000000000000 ) ) ;
#12247 = CARTESIAN_POINT ( 'NONE',  ( -5.565113727472241756, 10.17789316117534959, 42.00000000000001421 ) ) ;
#12248 = ORIENTED_EDGE ( 'NONE', *, *, #28466, .T. ) ;
#12249 = EDGE_CURVE ( 'NONE', #42351, #37895, #422, .T. ) ;
#12250 = VECTOR ( 'NONE', #6093, 1000.000000000000000 ) ;
#12251 = CARTESIAN_POINT ( 'NONE',  ( 0.000000000000000000, 16.45098606841173705, -33.79645857604496229 ) ) ;
#12252 = ORIENTED_EDGE ( 'NONE', *, *, #47091, .T. ) ;
#12253 = ORIENTED_EDGE ( 'NONE', *, *, #46995, .T. ) ;
#12254 = ORIENTED_EDGE ( 'NONE', *, *, #17632, .F. ) ;
#12255 = EDGE_LOOP ( 'NONE', ( #2021, #1152, #9734, #38077 ) ) ;
#12256 = AXIS2_PLACEMENT_3D ( 'NONE', #46153, #633, #8217 ) ;
#12257 = CARTESIAN_POINT ( 'NONE',  ( 0.000000000000000000, 72.35432306680485226, -20.40083707022909110 ) ) ;
#12258 = VERTEX_POINT ( 'NONE', #19259 ) ;
#12259 = ORIENTED_EDGE ( 'NONE', *, *, #34403, .T. ) ;
#12260 = CARTESIAN_POINT ( 'NONE',  ( 15.00000000000000000, 9.615535125379096826, 24.73947219025905042 ) ) ;
#12261 = VERTEX_POINT ( 'NONE', #15592 ) ;
#12262 = DIRECTION ( 'NONE',  ( -1.000000000000000000, -0.000000000000000000, 0.000000000000000000 ) ) ;
#12263 = ORIENTED_EDGE ( 'NONE', *, *, #41082, .F. ) ;
#12264 = CIRCLE ( 'NONE', #6768, 16.00000000000000000 ) ;
#12265 = CARTESIAN_POINT ( 'NONE',  ( 5.999999999999999112, -64.81221759200379040, 50.23322058963324110 ) ) ;
#12266 = DIRECTION ( 'NONE',  ( -0.000000000000000000, 0.2079116908177543743, 0.9781476007338066880 ) ) ;
#12267 = ORIENTED_EDGE ( 'NONE', *, *, #27987, .F. ) ;
#12268 = CARTESIAN_POINT ( 'NONE',  ( 10.00000000000000000, 0.000000000000000000, 0.000000000000000000 ) ) ;
#12269 = VERTEX_POINT ( 'NONE', #30521 ) ;
#12270 = CARTESIAN_POINT ( 'NONE',  ( 0.000000000000000000, 0.000000000000000000, 0.000000000000000000 ) ) ;
#12271 = CARTESIAN_POINT ( 'NONE',  ( 0.000000000000000000, 81.50828551894240093, -8.966570791699803422 ) ) ;
#12272 = ORIENTED_EDGE ( 'NONE', *, *, #825, .F. ) ;
#12273 = AXIS2_PLACEMENT_3D ( 'NONE', #37795, #1326, #46605 ) ;
#12274 = LINE ( 'NONE', #12033, #26400 ) ;
#12275 = ORIENTED_EDGE ( 'NONE', *, *, #20720, .F. ) ;
#12276 = EDGE_LOOP ( 'NONE', ( #14116, #1461 ) ) ;
#12277 = CARTESIAN_POINT ( 'NONE',  ( 0.000000000000000000, 0.000000000000000000, 0.000000000000000000 ) ) ;
#12278 = CARTESIAN_POINT ( 'NONE',  ( 10.00000000000000000, -51.02545421589285723, -55.20638768913812555 ) ) ;
#12279 = ORIENTED_EDGE ( 'NONE', *, *, #16790, .F. ) ;
#12280 = EDGE_CURVE ( 'NONE', #2339, #37110, #45445, .T. ) ;
#12281 = DIRECTION ( 'NONE',  ( -1.000000000000000000, -0.000000000000000000, -0.000000000000000000 ) ) ;
#12282 = LINE ( 'NONE', #20091, #44635 ) ;
#12283 = CARTESIAN_POINT ( 'NONE',  ( 15.00000000000000000, -23.29833615347104470, 3.418703333116808629 ) ) ;
#12284 = AXIS2_PLACEMENT_3D ( 'NONE', #41304, #37863, #8246 ) ;
#12285 = DIRECTION ( 'NONE',  ( 1.000000000000000000, -0.000000000000000000, -0.000000000000000000 ) ) ;
#12286 = EDGE_CURVE ( 'NONE', #33476, #16326, #3734, .T. ) ;
#12287 = CARTESIAN_POINT ( 'NONE',  ( 0.000000000000000000, 38.55633173627010279, 16.65560815589424593 ) ) ;
#12288 = AXIS2_PLACEMENT_3D ( 'NONE', #20456, #16088, #42503 ) ;
#12289 = DIRECTION ( 'NONE',  ( 1.000000000000000000, 0.000000000000000000, 0.000000000000000000 ) ) ;
#12290 = FACE_OUTER_BOUND ( 'NONE', #41017, .T. ) ;
#12291 = EDGE_CURVE ( 'NONE', #16979, #41890, #6034, .T. ) ;
#12292 = LINE ( 'NONE', #16429, #20928 ) ;
#12293 = CARTESIAN_POINT ( 'NONE',  ( 11.59999999999999787, 1.420590287010929336E-15, 42.00000000000001421 ) ) ;
#12294 = ORIENTED_EDGE ( 'NONE', *, *, #22596, .T. ) ;
#12295 = ORIENTED_EDGE ( 'NONE', *, *, #11929, .T. ) ;
#12296 = CARTESIAN_POINT ( 'NONE',  ( 10.00000000000000000, -75.16055320797016748, -18.89407956138335365 ) ) ;
#12297 = CARTESIAN_POINT ( 'NONE',  ( 11.99999999999999822, 0.000000000000000000, 0.000000000000000000 ) ) ;
#12298 = DIRECTION ( 'NONE',  ( 0.000000000000000000, 0.000000000000000000, 1.000000000000000000 ) ) ;
#12299 = VERTEX_POINT ( 'NONE', #17029 ) ;
#12300 = ADVANCED_FACE ( 'NONE', ( #46670 ), #9208, .F. ) ;
#12301 = ORIENTED_EDGE ( 'NONE', *, *, #12030, .F. ) ;
#12302 = CIRCLE ( 'NONE', #25580, 31.99999999999998224 ) ;
#12303 = DIRECTION ( 'NONE',  ( 0.000000000000000000, 0.4067366430757887730, -0.9135454576426059736 ) ) ;
#12304 = ORIENTED_EDGE ( 'NONE', *, *, #9761, .T. ) ;
#12305 = EDGE_CURVE ( 'NONE', #13689, #47062, #3423, .T. ) ;
#12306 = LINE ( 'NONE', #46554, #37767 ) ;
#12307 = AXIS2_PLACEMENT_3D ( 'NONE', #30828, #45752, #46231 ) ;
#12308 = FACE_OUTER_BOUND ( 'NONE', #23093, .T. ) ;
#12309 = ORIENTED_EDGE ( 'NONE', *, *, #39691, .F. ) ;
#12310 = EDGE_CURVE ( 'NONE', #13430, #35720, #35873, .T. ) ;
#12311 = VECTOR ( 'NONE', #45551, 1000.000000000000000 ) ;
#12312 = CARTESIAN_POINT ( 'NONE',  ( 11.99999999999999822, -31.46837873495025306, 68.27212725128265447 ) ) ;
#12313 = ORIENTED_EDGE ( 'NONE', *, *, #3741, .T. ) ;
#12314 = AXIS2_PLACEMENT_3D ( 'NONE', #7337, #36705, #29611 ) ;
#12315 = EDGE_CURVE ( 'NONE', #24628, #6878, #12842, .T. ) ;
#12316 = FACE_OUTER_BOUND ( 'NONE', #45403, .T. ) ;
#12317 = DIRECTION ( 'NONE',  ( -1.000000000000000000, -0.000000000000000000, -0.000000000000000000 ) ) ;
#12318 = ORIENTED_EDGE ( 'NONE', *, *, #7636, .F. ) ;
#12320 = ORIENTED_EDGE ( 'NONE', *, *, #15202, .F. ) ;
#12319 = CARTESIAN_POINT ( 'NONE',  ( 11.99999999999999822, 0.000000000000000000, 0.000000000000000000 ) ) ;
#12321 = VERTEX_POINT ( 'NONE', #39803 ) ;
#12322 = CARTESIAN_POINT ( 'NONE',  ( 10.00000000000000000, 0.000000000000000000, 0.000000000000000000 ) ) ;
#12323 = CARTESIAN_POINT ( 'NONE',  ( 26.09152095774781799, -124.8716048804687375, 5.500000000000000000 ) ) ;
#12324 = CARTESIAN_POINT ( 'NONE',  ( 0.000000000000000000, 68.26794271651262136, 31.47745569255165066 ) ) ;
#12326 = CARTESIAN_POINT ( 'NONE',  ( 0.000000000000000000, -120.0000000000000000, -40.00000000000000711 ) ) ;
#12325 = CIRCLE ( 'NONE', #46744, 31.99999999999998934 ) ;
#12327 = EDGE_LOOP ( 'NONE', ( #19579, #41452, #26835, #18336 ) ) ;
#12328 = FACE_OUTER_BOUND ( 'NONE', #29013, .T. ) ;
#12329 = VERTEX_POINT ( 'NONE', #27833 ) ;
#12330 = ORIENTED_EDGE ( 'NONE', *, *, #32508, .F. ) ;
#12331 = EDGE_CURVE ( 'NONE', #21662, #18852, #36277, .T. ) ;
#12332 = DIRECTION ( 'NONE',  ( 0.000000000000000000, 0.6691306063588563502, 0.7431448254773960205 ) ) ;
#12334 = EDGE_CURVE ( 'NONE', #20027, #22296, #29217, .T. ) ;
#12333 = VECTOR ( 'NONE', #2998, 1000.000000000000000 ) ;
#12335 = LINE ( 'NONE', #7916, #6649 ) ;
#12336 = CARTESIAN_POINT ( 'NONE',  ( 10.00000000000000000, 0.000000000000000000, 0.000000000000000000 ) ) ;
#12337 = FACE_OUTER_BOUND ( 'NONE', #20881, .T. ) ;
#12338 = VERTEX_POINT ( 'NONE', #39571 ) ;
#12339 = DIRECTION ( 'NONE',  ( -1.000000000000000000, 0.000000000000000000, 0.000000000000000000 ) ) ;
#12340 = CYLINDRICAL_SURFACE ( 'NONE', #18214, 82.00000000000000000 ) ;
#12341 = EDGE_CURVE ( 'NONE', #24133, #14824, #36113, .T. ) ;
#12342 = DIRECTION ( 'NONE',  ( -0.6064928550163533050, -0.7950889364178781449, 0.000000000000000000 ) ) ;
#12343 = CARTESIAN_POINT ( 'NONE',  ( 0.000000000000000000, 77.49459641780886443, -0.8261519478433788644 ) ) ;
#12344 = DIRECTION ( 'NONE',  ( -0.3311129884571295534, -0.9435911131814398445, 0.000000000000000000 ) ) ;
#12345 = AXIS2_PLACEMENT_3D ( 'NONE', #26611, #19981, #23650 ) ;
#12346 = CARTESIAN_POINT ( 'NONE',  ( 5.999999999999999112, -50.23322058963299241, -64.81221759200397514 ) ) ;
#12348 = EDGE_CURVE ( 'NONE', #29809, #35093, #28061, .T. ) ;
#12347 = PRESENTATION_STYLE_ASSIGNMENT (( #4747 ) ) ;
#12349 = CYLINDRICAL_SURFACE ( 'NONE', #5252, 16.00000000000000000 ) ;
#12350 = CARTESIAN_POINT ( 'NONE',  ( 10.00000000000000000, -68.27212725128254078, -31.46837873495049465 ) ) ;
#12351 = CARTESIAN_POINT ( 'NONE',  ( 50.00005079999999680, 0.000000000000000000, 0.000000000000000000 ) ) ;
#12352 = ORIENTED_EDGE ( 'NONE', *, *, #35778, .F. ) ;
#12353 = AXIS2_PLACEMENT_3D ( 'NONE', #13249, #28170, #24499 ) ;
#12354 = PLANE ( 'NONE',  #19348 ) ;
#12355 = DIRECTION ( 'NONE',  ( -1.000000000000000000, 0.000000000000000000, 0.000000000000000000 ) ) ;
#12356 = ORIENTED_EDGE ( 'NONE', *, *, #25576, .T. ) ;
#12357 = ORIENTED_EDGE ( 'NONE', *, *, #13825, .T. ) ;
#12358 = DIRECTION ( 'NONE',  ( 0.000000000000000000, -0.8910065241883722287, 0.4539904997395382558 ) ) ;
#12359 = CARTESIAN_POINT ( 'NONE',  ( 10.00000000000000000, 0.000000000000000000, 0.000000000000000000 ) ) ;
#12360 = ORIENTED_EDGE ( 'NONE', *, *, #20386, .F. ) ;
#12361 = CIRCLE ( 'NONE', #1418, 77.49899999999999523 ) ;
#12362 = EDGE_CURVE ( 'NONE', #31758, #41512, #2116, .T. ) ;
#12363 = ORIENTED_EDGE ( 'NONE', *, *, #10167, .F. ) ;
#12364 = CIRCLE ( 'NONE', #46747, 82.00000000000000000 ) ;
#12365 = ORIENTED_EDGE ( 'NONE', *, *, #17529, .T. ) ;
#12366 = ORIENTED_EDGE ( 'NONE', *, *, #2016, .T. ) ;
#12367 = AXIS2_PLACEMENT_3D ( 'NONE', #31779, #13388, #8992 ) ;
#12368 = ORIENTED_EDGE ( 'NONE', *, *, #15473, .F. ) ;
#12369 = CARTESIAN_POINT ( 'NONE',  ( 12.00000000000000000, -23.29833615347109088, -3.418703333116486665 ) ) ;
#12370 = ORIENTED_EDGE ( 'NONE', *, *, #44723, .F. ) ;
#12371 = DIRECTION ( 'NONE',  ( 0.000000000000000000, 0.000000000000000000, -1.000000000000000000 ) ) ;
#12372 = DIRECTION ( 'NONE',  ( 0.000000000000000000, 0.7071067811865487940, -0.7071067811865463515 ) ) ;
#12373 = EDGE_LOOP ( 'NONE', ( #7541, #3033, #10763, #46094 ) ) ;
#12374 = CARTESIAN_POINT ( 'NONE',  ( 10.00000000000000000, -14.67089635893764665, 73.72996012237435082 ) ) ;
#12375 =( GEOMETRIC_REPRESENTATION_CONTEXT ( 3 ) GLOBAL_UNCERTAINTY_ASSIGNED_CONTEXT ( ( #33523 ) ) GLOBAL_UNIT_ASSIGNED_CONTEXT ( ( #40232, #31759, #28065 ) ) REPRESENTATION_CONTEXT ( 'NONE', 'WORKASPACE' ) );
#12376 = ORIENTED_EDGE ( 'NONE', *, *, #31970, .F. ) ;
#12377 = CARTESIAN_POINT ( 'NONE',  ( 1.250000000000000000, -12.36245420541525597, -1.199999999999999956 ) ) ;
#12378 = CARTESIAN_POINT ( 'NONE',  ( 10.00000000000000000, 27.05870788708267582, -26.08949754952995903 ) ) ;
#12379 = CARTESIAN_POINT ( 'NONE',  ( 10.00000000000000000, 71.91182617369230456, -28.89263327155667938 ) ) ;
#12380 = CIRCLE ( 'NONE', #22509, 82.00000000000000000 ) ;
#12381 = VERTEX_POINT ( 'NONE', #35641 ) ;
#12382 = ORIENTED_EDGE ( 'NONE', *, *, #44235, .T. ) ;
#12383 = CYLINDRICAL_SURFACE ( 'NONE', #9144, 12.50000000000000000 ) ;
#12384 = ORIENTED_EDGE ( 'NONE', *, *, #38679, .F. ) ;
#12385 = EDGE_CURVE ( 'NONE', #2031, #12921, #23906, .T. ) ;
#12386 = DIRECTION ( 'NONE',  ( 0.000000000000000000, 0.000000000000000000, 1.000000000000000000 ) ) ;
#12387 = CARTESIAN_POINT ( 'NONE',  ( 0.000000000000000000, 0.000000000000000000, 0.000000000000000000 ) ) ;
#12388 = FACE_OUTER_BOUND ( 'NONE', #48366, .T. ) ;
#12389 = CARTESIAN_POINT ( 'NONE',  ( 0.000000000000000000, 0.000000000000000000, 0.000000000000000000 ) ) ;
#12390 = CARTESIAN_POINT ( 'NONE',  ( 15.00000000000000000, 9.615535125378766423, -24.73947219025917121 ) ) ;
#12391 = ADVANCED_FACE ( 'NONE', ( #47130 ), #20457, .F. ) ;
#12392 = DIRECTION ( 'NONE',  ( 0.000000000000000000, -0.3090169943749349057, -0.9510565162951577500 ) ) ;
#12393 = DIRECTION ( 'NONE',  ( 0.000000000000000000, -0.4539904997395541320, 0.8910065241883640130 ) ) ;
#12394 = ORIENTED_EDGE ( 'NONE', *, *, #48389, .F. ) ;
#12395 = CARTESIAN_POINT ( 'NONE',  ( 0.000000000000000000, 9.188173127307290855, 40.98264845739752360 ) ) ;
#12396 = LINE ( 'NONE', #7978, #10286 ) ;
#12397 = CARTESIAN_POINT ( 'NONE',  ( 11.99999999999999822, -5.256550761633395297, 77.32052557432841411 ) ) ;
#12398 = ORIENTED_EDGE ( 'NONE', *, *, #41952, .T. ) ;
#12399 = ORIENTED_EDGE ( 'NONE', *, *, #38888, .T. ) ;
#12401 = EDGE_CURVE ( 'NONE', #7113, #15986, #17511, .T. ) ;
#12400 = DIRECTION ( 'NONE',  ( -1.000000000000000000, -0.000000000000000000, 0.000000000000000000 ) ) ;
#12402 = CARTESIAN_POINT ( 'NONE',  ( 10.00000000000000000, 74.65374052328660071, -8.840884882374309583 ) ) ;
#12403 = EDGE_CURVE ( 'NONE', #9900, #43945, #15957, .T. ) ;
#12404 = VECTOR ( 'NONE', #24186, 1000.000000000000000 ) ;
#12405 = DIRECTION ( 'NONE',  ( -1.000000000000000000, 0.000000000000000000, 0.000000000000000000 ) ) ;
#12406 = CARTESIAN_POINT ( 'NONE',  ( 10.00000000000000000, 51.03279382321088065, 55.19960302592086521 ) ) ;
#12407 = VECTOR ( 'NONE', #31466, 1000.000000000000000 ) ;
#12408 = DIRECTION ( 'NONE',  ( 1.000000000000000000, 0.000000000000000000, 0.000000000000000000 ) ) ;
#12409 = CARTESIAN_POINT ( 'NONE',  ( 0.000000000000000000, 0.000000000000000000, 0.000000000000000000 ) ) ;
#12410 = DIRECTION ( 'NONE',  ( -1.000000000000000000, 0.000000000000000000, 0.000000000000000000 ) ) ;
#12411 = EDGE_LOOP ( 'NONE', ( #13626, #32475, #18789, #13425 ) ) ;
#12412 = EDGE_CURVE ( 'NONE', #10381, #47625, #9935, .T. ) ;
#12413 = ORIENTED_EDGE ( 'NONE', *, *, #9664, .T. ) ;
#12414 = PRODUCT_DEFINITION_SHAPE ( 'NONE', 'NONE',  #36966 ) ;
#12415 = CARTESIAN_POINT ( 'NONE',  ( 10.00000000000000000, -37.16516213103280108, 4.992566952384862589 ) ) ;
#12416 = ORIENTED_EDGE ( 'NONE', *, *, #6973, .T. ) ;
#12417 = CIRCLE ( 'NONE', #39777, 31.99999999999999289 ) ;
#12418 = ORIENTED_EDGE ( 'NONE', *, *, #756, .T. ) ;
#12419 = DIRECTION ( 'NONE',  ( 0.6064928550163531940, 0.7950889364178782559, 0.000000000000000000 ) ) ;
#12420 = ORIENTED_EDGE ( 'NONE', *, *, #9331, .F. ) ;
#12421 = ORIENTED_EDGE ( 'NONE', *, *, #24813, .F. ) ;
#12422 = VECTOR ( 'NONE', #22028, 1000.000000000000000 ) ;
#12423 = CARTESIAN_POINT ( 'NONE',  ( 26.47460221209471598, -121.8961639463267090, -5.500000000000000000 ) ) ;
#12424 = DIRECTION ( 'NONE',  ( -1.000000000000000000, 0.000000000000000000, 0.000000000000000000 ) ) ;
#12425 = EDGE_CURVE ( 'NONE', #22554, #32703, #42545, .T. ) ;
#12426 = AXIS2_PLACEMENT_3D ( 'NONE', #32050, #23720, #31089 ) ;
#12427 = ORIENTED_EDGE ( 'NONE', *, *, #6973, .F. ) ;
#12428 = ORIENTED_EDGE ( 'NONE', *, *, #19467, .T. ) ;
#12429 = VECTOR ( 'NONE', #28975, 1000.000000000000000 ) ;
#12430 = EDGE_CURVE ( 'NONE', #3463, #21150, #21425, .T. ) ;
#12431 = LINE ( 'NONE', #8739, #18606 ) ;
#12433 = EDGE_LOOP ( 'NONE', ( #25790, #21297, #8918, #9270 ) ) ;
#12432 = DIRECTION ( 'NONE',  ( -1.000000000000000000, 0.000000000000000000, -0.000000000000000000 ) ) ;
#12434 = CARTESIAN_POINT ( 'NONE',  ( 11.99999999999999822, -81.50828551894234408, 8.966570791700414489 ) ) ;
#12435 = ORIENTED_EDGE ( 'NONE', *, *, #46852, .T. ) ;
#12436 = CARTESIAN_POINT ( 'NONE',  ( 21.85433023846371370, -135.0628101570779620, 5.500000000000000000 ) ) ;
#12437 = VERTEX_POINT ( 'NONE', #42756 ) ;
#12438 = ORIENTED_EDGE ( 'NONE', *, *, #34994, .F. ) ;
#12439 = CARTESIAN_POINT ( 'NONE',  ( -10.43921258969510824, -98.89258801967538659, 5.500000000000000000 ) ) ;
#12440 = DIRECTION ( 'NONE',  ( 0.000000000000000000, 0.8910065241883688980, -0.4539904997395446951 ) ) ;
#12441 = ORIENTED_EDGE ( 'NONE', *, *, #33647, .F. ) ;
#12442 = DIRECTION ( 'NONE',  ( 0.000000000000000000, -0.5877852522924803536, 0.8090169943749422332 ) ) ;
#12443 = CARTESIAN_POINT ( 'NONE',  ( 10.00000000000000000, 41.76937507738875155, -62.50329211542393892 ) ) ;
#12444 = EDGE_CURVE ( 'NONE', #25916, #11028, #11270, .T. ) ;
#12445 = DIRECTION ( 'NONE',  ( 0.000000000000000000, 0.000000000000000000, 1.000000000000000000 ) ) ;
#12446 = ORIENTED_EDGE ( 'NONE', *, *, #19334, .F. ) ;
#12447 = EDGE_CURVE ( 'NONE', #23509, #1910, #22144, .T. ) ;
#12448 = ADVANCED_FACE ( 'NONE', ( #25807 ), #14580, .T. ) ;
#12449 = ORIENTED_EDGE ( 'NONE', *, *, #24148, .F. ) ;
#12450 = AXIS2_PLACEMENT_3D ( 'NONE', #35518, #27955, #42873 ) ;
#12451 = DIRECTION ( 'NONE',  ( 0.000000000000000000, -0.4539904997395350361, -0.8910065241883738940 ) ) ;
#12452 = LINE ( 'NONE', #9018, #29786 ) ;
#12453 = ORIENTED_EDGE ( 'NONE', *, *, #20046, .F. ) ;
#12454 = FACE_OUTER_BOUND ( 'NONE', #23444, .T. ) ;
#12455 = VERTEX_POINT ( 'NONE', #18480 ) ;
#12456 = CYLINDRICAL_SURFACE ( 'NONE', #45714, 32.00000000000000000 ) ;
#12457 = CARTESIAN_POINT ( 'NONE',  ( 11.99999999999999822, 41.19522573413733113, 65.64334221924924861 ) ) ;
#12458 = CARTESIAN_POINT ( 'NONE',  ( 0.000000000000000000, 37.22597642581158084, -5.202137450156524068 ) ) ;
#12459 = EDGE_CURVE ( 'NONE', #22407, #37035, #5792, .T. ) ;
#12460 = DIRECTION ( 'NONE',  ( -1.000000000000000000, 0.000000000000000000, 0.000000000000000000 ) ) ;
#12461 = EDGE_LOOP ( 'NONE', ( #44220, #26448, #28866, #4788 ) ) ;
#12462 = DIRECTION ( 'NONE',  ( 0.000000000000000000, 0.000000000000000000, 1.000000000000000000 ) ) ;
#12463 = CARTESIAN_POINT ( 'NONE',  ( 10.00000000000000000, 37.58145647212453611, 16.68533520207917675 ) ) ;
#12464 = AXIS2_PLACEMENT_3D ( 'NONE', #23286, #7634, #30631 ) ;
#12465 = CARTESIAN_POINT ( 'NONE',  ( 10.00000000000000000, 0.000000000000000000, 0.000000000000000000 ) ) ;
#12466 = AXIS2_PLACEMENT_3D ( 'NONE', #9281, #1960, #16879 ) ;
#12467 = CARTESIAN_POINT ( 'NONE',  ( 10.00000000000000000, -23.16143007188376757, -73.95703589263997912 ) ) ;
#12468 = TOROIDAL_SURFACE ( 'NONE', #39823, 12.80000000000000071, 0.2999999999999999334 ) ;
#12469 = CARTESIAN_POINT ( 'NONE',  ( 10.00000000000000000, -12.26510123303284594, 35.53030884539080603 ) ) ;
#12470 = ORIENTED_EDGE ( 'NONE', *, *, #3713, .T. ) ;
#12471 = VERTEX_POINT ( 'NONE', #10896 ) ;
#12472 = CARTESIAN_POINT ( 'NONE',  ( 0.000000000000000000, 2.946379043147425492, -75.11764819372145041 ) ) ;
#12473 = ORIENTED_EDGE ( 'NONE', *, *, #17328, .T. ) ;
#12474 = ORIENTED_EDGE ( 'NONE', *, *, #38695, .F. ) ;
#12475 = DIRECTION ( 'NONE',  ( -1.000000000000000000, 0.000000000000000000, -0.000000000000000000 ) ) ;
#12476 = DIRECTION ( 'NONE',  ( 0.000000000000000000, 0.8910065241883690090, -0.4539904997395446395 ) ) ;
#12477 = VERTEX_POINT ( 'NONE', #17753 ) ;
#12478 = EDGE_CURVE ( 'NONE', #1469, #4110, #41006, .T. ) ;
#12479 = EDGE_CURVE ( 'NONE', #911, #9557, #36358, .T. ) ;
#12480 = CARTESIAN_POINT ( 'NONE',  ( 0.000000000000000000, -5.202137450156655518, 37.22597642581156663 ) ) ;
#12481 = ORIENTED_EDGE ( 'NONE', *, *, #45645, .T. ) ;
#12482 = ORIENTED_EDGE ( 'NONE', *, *, #6405, .T. ) ;
#12483 = EDGE_CURVE ( 'NONE', #6361, #36067, #26117, .T. ) ;
#12484 = ORIENTED_EDGE ( 'NONE', *, *, #12655, .F. ) ;
#12485 = EDGE_LOOP ( 'NONE', ( #29353, #31179, #24058, #46017 ) ) ;
#12486 = ORIENTED_EDGE ( 'NONE', *, *, #4368, .T. ) ;
#12487 = ORIENTED_EDGE ( 'NONE', *, *, #924, .T. ) ;
#12488 = EDGE_CURVE ( 'NONE', #1183, #18610, #313, .T. ) ;
#12489 = CIRCLE ( 'NONE', #3887, 32.00000000000000000 ) ;
#12490 = DIRECTION ( 'NONE',  ( 0.000000000000000000, 0.000000000000000000, 1.000000000000000000 ) ) ;
#12492 = ORIENTED_EDGE ( 'NONE', *, *, #9825, .F. ) ;
#12491 = AXIS2_PLACEMENT_3D ( 'NONE', #26332, #37096, #7490 ) ;
#12493 = DIRECTION ( 'NONE',  ( -1.000000000000000000, 0.000000000000000000, -0.000000000000000000 ) ) ;
#12494 = VERTEX_POINT ( 'NONE', #21897 ) ;
#12495 = DIRECTION ( 'NONE',  ( 0.000000000000000000, 0.000000000000000000, 1.000000000000000000 ) ) ;
#12496 = AXIS2_PLACEMENT_3D ( 'NONE', #39814, #25586, #43488 ) ;
#12497 = CYLINDRICAL_SURFACE ( 'NONE', #35600, 82.00000000000000000 ) ;
#12498 = DIRECTION ( 'NONE',  ( -1.000000000000000000, 0.000000000000000000, 0.000000000000000000 ) ) ;
#12499 = ORIENTED_EDGE ( 'NONE', *, *, #47959, .T. ) ;
#12500 = COLOUR_RGB ( '', 0.08235294, 0.09019608, 0.10196078) ;
#12501 = EDGE_CURVE ( 'NONE', #36119, #48169, #33931, .T. ) ;
#12502 = LINE ( 'NONE', #12740, #5574 ) ;
#12503 = ADVANCED_FACE ( 'NONE', ( #18223 ), #11139, .T. ) ;
#12504 = ORIENTED_EDGE ( 'NONE', *, *, #9177, .T. ) ;
#12505 = CARTESIAN_POINT ( 'NONE',  ( 0.000000000000000000, 28.89263327155746097, 71.91182617369197771 ) ) ;
#12506 = CARTESIAN_POINT ( 'NONE',  ( 10.00000000000000000, 0.000000000000000000, 0.000000000000000000 ) ) ;
#12507 = ORIENTED_EDGE ( 'NONE', *, *, #26075, .F. ) ;
#12508 = CARTESIAN_POINT ( 'NONE',  ( 10.00000000000000000, 0.000000000000000000, 0.000000000000000000 ) ) ;
#12509 = ORIENTED_EDGE ( 'NONE', *, *, #23657, .T. ) ;
#12510 = CIRCLE ( 'NONE', #45332, 77.49899999999999523 ) ;
#12511 = VERTEX_POINT ( 'NONE', #32678 ) ;
#12512 = FACE_OUTER_BOUND ( 'NONE', #32750, .T. ) ;
#12513 = DIRECTION ( 'NONE',  ( -1.000000000000000000, 0.000000000000000000, -0.000000000000000000 ) ) ;
#12514 = CARTESIAN_POINT ( 'NONE',  ( 15.00000000000000000, -1.278221433540507546, -26.51162292216071492 ) ) ;
#12515 = DIRECTION ( 'NONE',  ( 0.000000000000000000, 0.000000000000000000, 1.000000000000000000 ) ) ;
#12516 = DIRECTION ( 'NONE',  ( 0.000000000000000000, 0.000000000000000000, 1.000000000000000000 ) ) ;
#12517 = PRODUCT_DEFINITION_SHAPE ( 'NONE', 'NONE',  #48462 ) ;
#12518 = DIRECTION ( 'NONE',  ( 0.000000000000000000, -0.2079116908177641998, -0.9781476007338046896 ) ) ;
#12519 = CARTESIAN_POINT ( 'NONE',  ( 10.00000000000000000, 0.000000000000000000, 0.000000000000000000 ) ) ;
#12520 = EDGE_CURVE ( 'NONE', #42057, #18546, #7471, .T. ) ;
#12521 = CARTESIAN_POINT ( 'NONE',  ( 10.00000000000000000, -26.79245525562691199, -32.34446384430000876 ) ) ;
#12522 = DIRECTION ( 'NONE',  ( -1.000000000000000000, 0.000000000000000000, -0.000000000000000000 ) ) ;
#12523 = CARTESIAN_POINT ( 'NONE',  ( -26.53422223201112828, -120.6595836127786043, 5.500000000000000000 ) ) ;
#12524 = DIRECTION ( 'NONE',  ( 0.000000000000000000, 0.3826834323650841752, 0.9238795325112891810 ) ) ;
#12525 = SHAPE_REPRESENTATION ( 'fast gear_ISO - Spur gear 2M 40T 20PA 10FW ---S40A75H50L38.0N', ( #11636 ), #21829 ) ;
#12526 = FACE_OUTER_BOUND ( 'NONE', #2852, .T. ) ;
#12527 = PLANE ( 'NONE',  #12091 ) ;
#12528 = CARTESIAN_POINT ( 'NONE',  ( -1.250000000000000000, -12.36245420541525597, -1.199999999999999956 ) ) ;
#12529 = VERTEX_POINT ( 'NONE', #15054 ) ;
#12530 = ORIENTED_EDGE ( 'NONE', *, *, #22932, .F. ) ;
#12531 = AXIS2_PLACEMENT_3D ( 'NONE', #14351, #11160, #48355 ) ;
#12532 = CARTESIAN_POINT ( 'NONE',  ( -12.50000000000000000, -107.5000000000000000, 2.500000000000000000 ) ) ;
#12533 = CIRCLE ( 'NONE', #39879, 37.49900000000000233 ) ;
#12534 = ORIENTED_EDGE ( 'NONE', *, *, #4353, .F. ) ;
#12535 = CARTESIAN_POINT ( 'NONE',  ( 10.00000000000000000, 4.992566952385523393, -37.16516213103272293 ) ) ;
#12536 = VECTOR ( 'NONE', #36716, 1000.000000000000000 ) ;
#12537 = PRODUCT_CONTEXT ( 'NONE', #20072, 'mechanical' ) ;
#12538 = DIRECTION ( 'NONE',  ( -1.000000000000000000, 0.000000000000000000, -0.000000000000000000 ) ) ;
#12539 = VERTEX_POINT ( 'NONE', #43700 ) ;
#12540 = CIRCLE ( 'NONE', #37546, 77.49900000000000944 ) ;
#12541 = AXIS2_PLACEMENT_3D ( 'NONE', #6725, #21652, #6960 ) ;
#12542 = VECTOR ( 'NONE', #44280, 1000.000000000000000 ) ;
#12543 = FACE_OUTER_BOUND ( 'NONE', #16882, .T. ) ;
#12544 = EDGE_CURVE ( 'NONE', #38965, #37445, #8118, .T. ) ;
#12545 = VERTEX_POINT ( 'NONE', #10409 ) ;
#12546 = EDGE_CURVE ( 'NONE', #37697, #34943, #29497, .T. ) ;
#12547 = LINE ( 'NONE', #9576, #44080 ) ;
#12548 = DIRECTION ( 'NONE',  ( 0.000000000000000000, 0.8090169943749445647, 0.5877852522924770229 ) ) ;
#12549 = VERTEX_POINT ( 'NONE', #29003 ) ;
#12551 = ORIENTED_EDGE ( 'NONE', *, *, #21256, .T. ) ;
#12550 = CARTESIAN_POINT ( 'NONE',  ( 12.00000000000000000, 23.49999999999999645, 1.499999999999995337 ) ) ;
#12552 = EDGE_LOOP ( 'NONE', ( #28037, #46867, #32553, #14547 ) ) ;
#12553 = CARTESIAN_POINT ( 'NONE',  ( 24.95699195200416654, -110.9640411295978595, 5.500000000000000000 ) ) ;
#12554 = EDGE_CURVE ( 'NONE', #21021, #3684, #37076, .T. ) ;
#12555 = DIRECTION ( 'NONE',  ( 0.000000000000000000, 0.000000000000000000, 1.000000000000000000 ) ) ;
#12556 = LINE ( 'NONE', #19879, #24747 ) ;
#12557 = EDGE_CURVE ( 'NONE', #9289, #47392, #21671, .T. ) ;
#12558 = FACE_OUTER_BOUND ( 'NONE', #24927, .T. ) ;
#12559 = CIRCLE ( 'NONE', #40704, 37.49900000000001654 ) ;
#12560 = CARTESIAN_POINT ( 'NONE',  ( 10.00000000000000000, -0.8828120875903202602, 37.48860685352291000 ) ) ;
#12561 = ORIENTED_EDGE ( 'NONE', *, *, #39079, .F. ) ;
#12562 = DIRECTION ( 'NONE',  ( -1.000000000000000000, 0.000000000000000000, 0.000000000000000000 ) ) ;
#12563 = ORIENTED_EDGE ( 'NONE', *, *, #30627, .T. ) ;
#12564 = ADVANCED_FACE ( 'NONE', ( #40749 ), #7217, .T. ) ;
#12565 = CARTESIAN_POINT ( 'NONE',  ( 15.00000000000000000, 16.83928648764922542, -16.46020748918050458 ) ) ;
#12566 = AXIS2_PLACEMENT_3D ( 'NONE', #46828, #27754, #39236 ) ;
#12567 = VECTOR ( 'NONE', #6882, 1000.000000000000000 ) ;
#12568 = FACE_OUTER_BOUND ( 'NONE', #11649, .T. ) ;
#12569 = DIRECTION ( 'NONE',  ( -1.000000000000000000, 0.000000000000000000, 0.000000000000000000 ) ) ;
#12570 = CARTESIAN_POINT ( 'NONE',  ( 11.99999999999999822, -72.35160999960801576, -20.41045688087902121 ) ) ;
#12571 = VERTEX_POINT ( 'NONE', #25571 ) ;
#12572 = CARTESIAN_POINT ( 'NONE',  ( 0.000000000000000000, -39.47590169984795239, -71.87247863392457248 ) ) ;
#12573 = CARTESIAN_POINT ( 'NONE',  ( 15.00000000000000000, -10.45096189432344502, -21.10159698893425784 ) ) ;
#12574 = VECTOR ( 'NONE', #18859, 1000.000000000000000 ) ;
#12575 = DIRECTION ( 'NONE',  ( -1.000000000000000000, 0.000000000000000000, -0.000000000000000000 ) ) ;
#12576 = DIRECTION ( 'NONE',  ( 0.000000000000000000, 0.000000000000000000, 1.000000000000000000 ) ) ;
#12577 = EDGE_CURVE ( 'NONE', #6444, #22246, #37855, .T. ) ;
#12578 = CARTESIAN_POINT ( 'NONE',  ( 0.000000000000000000, -69.42325613327466272, 34.44570377933573724 ) ) ;
#12579 = DIRECTION ( 'NONE',  ( -1.000000000000000000, -0.000000000000000000, 0.000000000000000000 ) ) ;
#12580 = LINE ( 'NONE', #31438, #40034 ) ;
#12582 = DIRECTION ( 'NONE',  ( -0.000000000000000000, -0.000000000000000000, -1.000000000000000000 ) ) ;
#12581 = APPLICATION_CONTEXT ( 'automotive_design' ) ;
#12583 = DIRECTION ( 'NONE',  ( -1.000000000000000000, 0.000000000000000000, 0.000000000000000000 ) ) ;
#12584 = CARTESIAN_POINT ( 'NONE',  ( -2.977765906491215642, 1.885622467823562354E-15, 15.39727592589476579 ) ) ;
#12585 = ORIENTED_EDGE ( 'NONE', *, *, #42885, .T. ) ;
#12586 = ORIENTED_EDGE ( 'NONE', *, *, #42517, .T. ) ;
#12587 = PLANE ( 'NONE',  #6616 ) ;
#12588 = ORIENTED_EDGE ( 'NONE', *, *, #1610, .T. ) ;
#12589 = VERTEX_POINT ( 'NONE', #4756 ) ;
#12590 = CYLINDRICAL_SURFACE ( 'NONE', #5005, 16.00000000000000000 ) ;
#12591 = CARTESIAN_POINT ( 'NONE',  ( 0.000000000000000000, 0.000000000000000000, 0.000000000000000000 ) ) ;
#12592 = ORIENTED_EDGE ( 'NONE', *, *, #3030, .F. ) ;
#12593 = AXIS2_PLACEMENT_3D ( 'NONE', #41412, #14744, #3474 ) ;
#12594 = EDGE_CURVE ( 'NONE', #38214, #27745, #30231, .T. ) ;
#12595 = AXIS2_PLACEMENT_3D ( 'NONE', #21526, #2666, #9782 ) ;
#12596 = CIRCLE ( 'NONE', #47721, 1.000000000000000888 ) ;
#12597 = EDGE_CURVE ( 'NONE', #20955, #20223, #23119, .T. ) ;
#12598 = ORIENTED_EDGE ( 'NONE', *, *, #21877, .F. ) ;
#12599 = EDGE_CURVE ( 'NONE', #14436, #44520, #5009, .T. ) ;
#12600 = VERTEX_POINT ( 'NONE', #44910 ) ;
#12601 = EDGE_CURVE ( 'NONE', #3686, #22056, #41721, .T. ) ;
#12602 = CIRCLE ( 'NONE', #7148, 15.99999999999999822 ) ;
#12603 = AXIS2_PLACEMENT_3D ( 'NONE', #47479, #10521, #17852 ) ;
#12604 = DIRECTION ( 'NONE',  ( 0.000000000000000000, -0.6691306063588579045, 0.7431448254773945772 ) ) ;
#12605 = CIRCLE ( 'NONE', #3901, 16.00000000000000000 ) ;
#12606 = EDGE_CURVE ( 'NONE', #7073, #40831, #26889, .T. ) ;
#12607 = CYLINDRICAL_SURFACE ( 'NONE', #46134, 82.00000000000000000 ) ;
#12608 = CARTESIAN_POINT ( 'NONE',  ( 11.99999999999999822, 0.000000000000000000, 0.000000000000000000 ) ) ;
#12609 = ORIENTED_EDGE ( 'NONE', *, *, #43049, .T. ) ;
#12610 = FACE_OUTER_BOUND ( 'NONE', #39752, .T. ) ;
#12611 = EDGE_LOOP ( 'NONE', ( #579, #15198, #30675, #8568 ) ) ;
#12612 = ORIENTED_EDGE ( 'NONE', *, *, #24109, .T. ) ;
#12613 = LINE ( 'NONE', #12377, #12407 ) ;
#12614 = CARTESIAN_POINT ( 'NONE',  ( -10.00000000000000000, 0.000000000000000000, 0.000000000000000000 ) ) ;
#12615 = LINE ( 'NONE', #27542, #14161 ) ;
#12616 = ORIENTED_EDGE ( 'NONE', *, *, #32003, .T. ) ;
#12617 = ORIENTED_EDGE ( 'NONE', *, *, #7410, .T. ) ;
#12618 = DIRECTION ( 'NONE',  ( -1.000000000000000000, 0.000000000000000000, 0.000000000000000000 ) ) ;
#12619 = VERTEX_POINT ( 'NONE', #15306 ) ;
#12620 = EDGE_CURVE ( 'NONE', #38853, #2339, #45637, .T. ) ;
#12621 = DIRECTION ( 'NONE',  ( -1.000000000000000000, -0.000000000000000000, -0.000000000000000000 ) ) ;
#12622 = CARTESIAN_POINT ( 'NONE',  ( 2.047646702416564768, -96.54137380445985173, -5.500000000000000000 ) ) ;
#12623 = CARTESIAN_POINT ( 'NONE',  ( -11.59999999999999964, -0.8299999999999986278, -1.199999999999999956 ) ) ;
#12624 = CARTESIAN_POINT ( 'NONE',  ( 0.000000000000000000, 0.000000000000000000, 0.000000000000000000 ) ) ;
#12625 = LINE ( 'NONE', #9191, #17220 ) ;
#12626 = DIRECTION ( 'NONE',  ( 0.000000000000000000, 0.000000000000000000, 1.000000000000000000 ) ) ;
#12627 = DIRECTION ( 'NONE',  ( 0.000000000000000000, 0.000000000000000000, 1.000000000000000000 ) ) ;
#12628 = ORIENTED_EDGE ( 'NONE', *, *, #37290, .T. ) ;
#12629 = DIRECTION ( 'NONE',  ( 0.000000000000000000, 0.000000000000000000, 1.000000000000000000 ) ) ;
#12630 = LINE ( 'NONE', #19706, #23789 ) ;
#12631 = CIRCLE ( 'NONE', #3245, 15.99999999999999822 ) ;
#12632 = DIRECTION ( 'NONE',  ( 0.000000000000000000, 0.000000000000000000, 1.000000000000000000 ) ) ;
#12633 = ADVANCED_FACE ( 'NONE', ( #30963 ), #45627, .F. ) ;
#12634 = CARTESIAN_POINT ( 'NONE',  ( -25.50183398199384754, -112.6408924756582053, 5.500000000000000000 ) ) ;
#12635 = ORIENTED_EDGE ( 'NONE', *, *, #45344, .T. ) ;
#12636 = ORIENTED_EDGE ( 'NONE', *, *, #30178, .F. ) ;
#12637 = AXIS2_PLACEMENT_3D ( 'NONE', #15556, #11890, #41999 ) ;
#12638 = CARTESIAN_POINT ( 'NONE',  ( 11.99999999999999822, -31.46837873494930093, -68.27212725128309501 ) ) ;
#12639 = VECTOR ( 'NONE', #34635, 1000.000000000000000 ) ;
#12640 = AXIS2_PLACEMENT_3D ( 'NONE', #24884, #25116, #43502 ) ;
#12641 = CARTESIAN_POINT ( 'NONE',  ( 5.000000000000000000, -35.47612816024539484, 22.48208911017487921 ) ) ;
#12642 = CARTESIAN_POINT ( 'NONE',  ( -5.250000000000000888, -13.95926121303099343, -1.199999999999999956 ) ) ;
#12643 = EDGE_CURVE ( 'NONE', #30256, #22671, #30809, .T. ) ;
#12644 = AXIS2_PLACEMENT_3D ( 'NONE', #42018, #26833, #41528 ) ;
#12645 = CYLINDRICAL_SURFACE ( 'NONE', #1340, 31.99999999999998579 ) ;
#12646 = CARTESIAN_POINT ( 'NONE',  ( 0.000000000000000000, 0.000000000000000000, 77.49899999999999523 ) ) ;
#12647 = FACE_OUTER_BOUND ( 'NONE', #20659, .T. ) ;
#12648 = CARTESIAN_POINT ( 'NONE',  ( -0.8815729230226008184, -93.47222532549339746, 5.500000000000000000 ) ) ;
#12649 = ORIENTED_EDGE ( 'NONE', *, *, #21016, .T. ) ;
#12650 = CIRCLE ( 'NONE', #14212, 12.49999999999999822 ) ;
#12651 = ORIENTED_EDGE ( 'NONE', *, *, #1219, .T. ) ;
#12652 = SURFACE_STYLE_USAGE ( .BOTH. , #17035 ) ;
#12653 = CARTESIAN_POINT ( 'NONE',  ( 5.999999999999999112, -74.74816331893453025, 33.71516098798714722 ) ) ;
#12654 = ORIENTED_EDGE ( 'NONE', *, *, #9217, .F. ) ;
#12655 = EDGE_CURVE ( 'NONE', #32749, #21372, #12121, .T. ) ;
#12656 = ORIENTED_EDGE ( 'NONE', *, *, #22478, .F. ) ;
#12657 = ADVANCED_FACE ( 'NONE', ( #45889 ), #42196, .T. ) ;
#12658 = ORIENTED_EDGE ( 'NONE', *, *, #21216, .F. ) ;
#12659 = CARTESIAN_POINT ( 'NONE',  ( 11.99999999999999822, -8.966570791701281351, 81.50828551894223040 ) ) ;
#12660 = ADVANCED_FACE ( 'NONE', ( #8651 ), #15775, .T. ) ;
#12661 = VERTEX_POINT ( 'NONE', #22868 ) ;
#12662 = EDGE_CURVE ( 'NONE', #7732, #44453, #22627, .T. ) ;
#12663 = AXIS2_PLACEMENT_3D ( 'NONE', #42668, #15989, #42168 ) ;
#12664 = EDGE_CURVE ( 'NONE', #16286, #4226, #3464, .T. ) ;
#12665 = DIRECTION ( 'NONE',  ( 0.000000000000000000, 0.9969173337331276308, 0.07845909572784874608 ) ) ;
#12666 = AXIS2_PLACEMENT_3D ( 'NONE', #40432, #2484, #17659 ) ;
#12667 = DIRECTION ( 'NONE',  ( 1.000000000000000000, 0.000000000000000000, 0.000000000000000000 ) ) ;
#12668 = ORIENTED_EDGE ( 'NONE', *, *, #23476, .F. ) ;
#12669 = EDGE_LOOP ( 'NONE', ( #3046, #46163, #15914, #47676 ) ) ;
#12670 = AXIS2_PLACEMENT_3D ( 'NONE', #27513, #42689, #31193 ) ;
#12671 = AXIS2_PLACEMENT_3D ( 'NONE', #44174, #21887, #44652 ) ;
#12672 = DIRECTION ( 'NONE',  ( 0.000000000000000000, 0.000000000000000000, 1.000000000000000000 ) ) ;
#12674 = ORIENTED_EDGE ( 'NONE', *, *, #6572, .F. ) ;
#12673 = FACE_OUTER_BOUND ( 'NONE', #45099, .T. ) ;
#12675 = CARTESIAN_POINT ( 'NONE',  ( -42.50000000000000000, 1.530808498934191521E-15, 12.50000000000000000 ) ) ;
#12676 = EDGE_LOOP ( 'NONE', ( #31853, #1657, #3797, #27230 ) ) ;
#12677 = DIRECTION ( 'NONE',  ( -1.000000000000000000, 0.000000000000000000, 0.000000000000000000 ) ) ;
#12678 = ORIENTED_EDGE ( 'NONE', *, *, #29902, .T. ) ;
#12679 = ORIENTED_EDGE ( 'NONE', *, *, #28082, .F. ) ;
#12680 = CARTESIAN_POINT ( 'NONE',  ( 0.000000000000000000, 76.41127070299273782, 12.93880638057342836 ) ) ;
#12681 = CARTESIAN_POINT ( 'NONE',  ( 0.000000000000000000, 0.000000000000000000, 0.000000000000000000 ) ) ;
#12682 = VECTOR ( 'NONE', #10749, 1000.000000000000000 ) ;
#12683 = VERTEX_POINT ( 'NONE', #4999 ) ;
#12684 = DIRECTION ( 'NONE',  ( -1.000000000000000000, -0.000000000000000000, -0.000000000000000000 ) ) ;
#12685 = DIRECTION ( 'NONE',  ( -1.000000000000000000, 0.000000000000000000, 0.000000000000000000 ) ) ;
#12686 = DIRECTION ( 'NONE',  ( 0.000000000000000000, 0.000000000000000000, 1.000000000000000000 ) ) ;
#12687 = ORIENTED_EDGE ( 'NONE', *, *, #3557, .F. ) ;
#12688 = ORIENTED_EDGE ( 'NONE', *, *, #2144, .F. ) ;
#12689 = LINE ( 'NONE', #16360, #26653 ) ;
#12690 = DIRECTION ( 'NONE',  ( 0.000000000000000000, 1.445602896647339410E-16, -1.000000000000000000 ) ) ;
#12691 = EDGE_LOOP ( 'NONE', ( #35785, #27240, #37288, #24394 ) ) ;
#12692 = DIRECTION ( 'NONE',  ( 1.000000000000000000, -0.000000000000000000, -0.000000000000000000 ) ) ;
#12693 = ORIENTED_EDGE ( 'NONE', *, *, #9219, .T. ) ;
#12694 = CIRCLE ( 'NONE', #168, 16.00000000000000000 ) ;
#12695 = FACE_OUTER_BOUND ( 'NONE', #2974, .T. ) ;
#12696 = CARTESIAN_POINT ( 'NONE',  ( 15.00000000000000000, 23.49999999999999645, 1.499999999999995337 ) ) ;
#12697 = DIRECTION ( 'NONE',  ( 0.000000000000000000, 0.000000000000000000, -1.000000000000000000 ) ) ;
#12698 = ORIENTED_EDGE ( 'NONE', *, *, #16321, .T. ) ;
#12699 = CARTESIAN_POINT ( 'NONE',  ( 10.00000000000000000, -70.52718814184240159, -26.02418014898383802 ) ) ;
#12700 = DIRECTION ( 'NONE',  ( 0.000000000000000000, -0.6494480483301903195, 0.7604059656000252687 ) ) ;
#12702 = CIRCLE ( 'NONE', #39251, 35.50000000000000711 ) ;
#12701 = CYLINDRICAL_SURFACE ( 'NONE', #582, 82.00000000000000000 ) ;
#12703 = FACE_OUTER_BOUND ( 'NONE', #33360, .T. ) ;
#12704 = LINE ( 'NONE', #16376, #37948 ) ;
#12705 = ORIENTED_EDGE ( 'NONE', *, *, #11954, .T. ) ;
#12706 = CIRCLE ( 'NONE', #7209, 31.99999999999998934 ) ;
#12707 = CARTESIAN_POINT ( 'NONE',  ( -11.70000000000000107, 0.000000000000000000, 0.000000000000000000 ) ) ;
#12708 = AXIS2_PLACEMENT_3D ( 'NONE', #48436, #25672, #7808 ) ;
#12709 = VERTEX_POINT ( 'NONE', #34850 ) ;
#12710 = CARTESIAN_POINT ( 'NONE',  ( -3.000000000000000000, -0.9646360437375307573, 23.52805723605590060 ) ) ;
#12711 = EDGE_CURVE ( 'NONE', #16717, #5383, #7700, .T. ) ;
#12712 = ORIENTED_EDGE ( 'NONE', *, *, #11871, .F. ) ;
#12713 = DIRECTION ( 'NONE',  ( 1.000000000000000000, 0.000000000000000000, 0.000000000000000000 ) ) ;
#12714 = ADVANCED_FACE ( 'NONE', ( #29977 ), #26313, .T. ) ;
#12715 = DIRECTION ( 'NONE',  ( -1.000000000000000000, 0.000000000000000000, -0.000000000000000000 ) ) ;
#12716 = EDGE_LOOP ( 'NONE', ( #6066, #17255, #14971, #10243 ) ) ;
#12717 = ADVANCED_FACE ( 'NONE', ( #15532 ), #30466, .F. ) ;
#12718 = ORIENTED_EDGE ( 'NONE', *, *, #28071, .T. ) ;
#12719 = EDGE_CURVE ( 'NONE', #16993, #26599, #5830, .T. ) ;
#12720 = CARTESIAN_POINT ( 'NONE',  ( 10.00000000000000000, 0.000000000000000000, 0.000000000000000000 ) ) ;
#12721 = ORIENTED_EDGE ( 'NONE', *, *, #9922, .F. ) ;
#12722 = EDGE_LOOP ( 'NONE', ( #30852, #34071, #11896, #40587 ) ) ;
#12723 = ADVANCED_FACE ( 'NONE', ( #2283 ), #16499, .T. ) ;
#12724 = ORIENTED_EDGE ( 'NONE', *, *, #39541, .F. ) ;
#12725 = CIRCLE ( 'NONE', #35391, 77.49899999999999523 ) ;
#12726 = CIRCLE ( 'NONE', #3306, 42.00000000000000000 ) ;
#12727 = CIRCLE ( 'NONE', #15066, 37.49900000000001654 ) ;
#12728 = CARTESIAN_POINT ( 'NONE',  ( 5.000000000000000000, -63.97538442413463855, 51.29473840253199768 ) ) ;
#12729 = VERTEX_POINT ( 'NONE', #2065 ) ;
#12730 = VERTEX_POINT ( 'NONE', #31694 ) ;
#12731 = CYLINDRICAL_SURFACE ( 'NONE', #42695, 82.00000000000000000 ) ;
#12732 = ORIENTED_EDGE ( 'NONE', *, *, #38131, .F. ) ;
#12733 = DIRECTION ( 'NONE',  ( 0.000000000000000000, 0.9723699203976756689, 0.2334453638559094157 ) ) ;
#12734 = CIRCLE ( 'NONE', #8802, 42.00000000000000000 ) ;
#12735 = ADVANCED_FACE ( 'NONE', ( #9619 ), #21120, .T. ) ;
#12736 = CARTESIAN_POINT ( 'NONE',  ( -3.000000000000000000, -4.261787119644969479, -26.19803753235780519 ) ) ;
#12737 = CARTESIAN_POINT ( 'NONE',  ( 10.00000000000000000, 0.000000000000000000, 0.000000000000000000 ) ) ;
#12738 = AXIS2_PLACEMENT_3D ( 'NONE', #35446, #30827, #30569 ) ;
#12739 = EDGE_LOOP ( 'NONE', ( #17399, #40372, #9874, #39815 ) ) ;
#12740 = CARTESIAN_POINT ( 'NONE',  ( 11.99999999999999822, 24.73286445877705475, 73.44644590900068692 ) ) ;
#12741 = ORIENTED_EDGE ( 'NONE', *, *, #41797, .F. ) ;
#12742 = DIRECTION ( 'NONE',  ( 0.000000000000000000, 0.000000000000000000, 1.000000000000000000 ) ) ;
#12743 = DIRECTION ( 'NONE',  ( -1.000000000000000000, 0.000000000000000000, -0.000000000000000000 ) ) ;
#12744 = ORIENTED_EDGE ( 'NONE', *, *, #34134, .F. ) ;
#12745 = FACE_OUTER_BOUND ( 'NONE', #38537, .T. ) ;
#12746 = EDGE_LOOP ( 'NONE', ( #25637, #33473, #22950, #20560 ) ) ;
#12747 = EDGE_LOOP ( 'NONE', ( #11969, #31247, #26879, #8752 ) ) ;
#12748 = DIRECTION ( 'NONE',  ( -1.000000000000000000, -0.000000000000000000, -0.000000000000000000 ) ) ;
#12749 = CARTESIAN_POINT ( 'NONE',  ( 10.00000000000000000, 37.58145647212455032, -0.6853352020786441789 ) ) ;
#12750 = VECTOR ( 'NONE', #27288, 1000.000000000000000 ) ;
#12751 = CARTESIAN_POINT ( 'NONE',  ( 10.00000000000000000, -9.188173127307592836, 40.98264845739746676 ) ) ;
#12752 = CARTESIAN_POINT ( 'NONE',  ( 11.99999999999999822, 0.000000000000000000, 0.000000000000000000 ) ) ;
#12753 = DIRECTION ( 'NONE',  ( 0.000000000000000000, 0.000000000000000000, 1.000000000000000000 ) ) ;
#12754 = CARTESIAN_POINT ( 'NONE',  ( 10.00000000000000000, -6.736453364083292428, -36.88895765772640800 ) ) ;
#12755 = CARTESIAN_POINT ( 'NONE',  ( 10.00000000000000000, 76.66974797899837313, 11.30684508768368524 ) ) ;
#12756 = DIRECTION ( 'NONE',  ( -1.000000000000000000, 0.000000000000000000, 0.000000000000000000 ) ) ;
#12757 = EDGE_CURVE ( 'NONE', #12729, #15261, #46843, .T. ) ;
#12758 = CARTESIAN_POINT ( 'NONE',  ( 10.00000000000000000, 0.000000000000000000, 0.000000000000000000 ) ) ;
#12759 = CARTESIAN_POINT ( 'NONE',  ( 10.00000000000000000, -12.26510123303284594, 35.53030884539080603 ) ) ;
#12760 = DIRECTION ( 'NONE',  ( 0.000000000000000000, -0.6494480483301903195, 0.7604059656000252687 ) ) ;
#12761 = EDGE_CURVE ( 'NONE', #5067, #42424, #44914, .T. ) ;
#12762 = FACE_OUTER_BOUND ( 'NONE', #33239, .T. ) ;
#12763 = DIRECTION ( 'NONE',  ( -1.000000000000000000, 0.000000000000000000, 0.000000000000000000 ) ) ;
#12765 = CIRCLE ( 'NONE', #11993, 77.49899999999999523 ) ;
#12764 = SURFACE_STYLE_FILL_AREA ( #4931 ) ;
#12766 = CARTESIAN_POINT ( 'NONE',  ( -10.00000000000000000, 0.000000000000000000, 0.000000000000000000 ) ) ;
#12767 = EDGE_CURVE ( 'NONE', #23915, #11671, #34730, .T. ) ;
#12768 = ORIENTED_EDGE ( 'NONE', *, *, #45344, .F. ) ;
#12769 = CIRCLE ( 'NONE', #40119, 31.99999999999999289 ) ;
#12770 = ORIENTED_EDGE ( 'NONE', *, *, #41962, .T. ) ;
#12771 = CARTESIAN_POINT ( 'NONE',  ( 10.00000000000000000, -22.64427369931148348, -30.00120703465229965 ) ) ;
#12772 = CARTESIAN_POINT ( 'NONE',  ( 10.00000000000000000, 0.000000000000000000, 0.000000000000000000 ) ) ;
#12773 = AXIS2_PLACEMENT_3D ( 'NONE', #4330, #11438, #401 ) ;
#12774 = AXIS2_PLACEMENT_3D ( 'NONE', #13164, #20752, #35681 ) ;
#12775 = APPLICATION_PROTOCOL_DEFINITION ( 'draft international standard', 'automotive_design', 1998, #32577 ) ;
#12776 = AXIS2_PLACEMENT_3D ( 'NONE', #13645, #25609, #32490 ) ;
#12777 = FACE_OUTER_BOUND ( 'NONE', #25289, .T. ) ;
#12778 = EDGE_LOOP ( 'NONE', ( #18955, #21842, #14482, #33443 ) ) ;
#12779 = EDGE_CURVE ( 'NONE', #37478, #6985, #13547, .T. ) ;
#12780 = EDGE_CURVE ( 'NONE', #14949, #37649, #27518, .T. ) ;
#12781 = CIRCLE ( 'NONE', #6516, 77.49900000000000944 ) ;
#12782 = VECTOR ( 'NONE', #100, 1000.000000000000000 ) ;
#12783 = AXIS2_PLACEMENT_3D ( 'NONE', #25272, #29926, #28956 ) ;
#12784 = FACE_OUTER_BOUND ( 'NONE', #2354, .T. ) ;
#12785 = ORIENTED_EDGE ( 'NONE', *, *, #6757, .T. ) ;
#12786 = FILL_AREA_STYLE ('',( #46313 ) ) ;
#12787 = VECTOR ( 'NONE', #35834, 1000.000000000000000 ) ;
#12788 = EDGE_CURVE ( 'NONE', #34798, #30855, #28008, .T. ) ;
#12789 = CARTESIAN_POINT ( 'NONE',  ( 0.000000000000000000, 18.89407956138362010, -75.16055320797013906 ) ) ;
#12790 = ORIENTED_EDGE ( 'NONE', *, *, #21162, .T. ) ;
#12791 = DIRECTION ( 'NONE',  ( -0.000000000000000000, -0.000000000000000000, -1.000000000000000000 ) ) ;
#12792 = VERTEX_POINT ( 'NONE', #35333 ) ;
#12794 = ORIENTED_EDGE ( 'NONE', *, *, #21056, .T. ) ;
#12793 = LINE ( 'NONE', #9117, #7468 ) ;
#12795 = ORIENTED_EDGE ( 'NONE', *, *, #22006, .F. ) ;
#12796 = DIRECTION ( 'NONE',  ( 0.9580045777625458836, 0.2867529058022011412, 0.000000000000000000 ) ) ;
#12797 = DIRECTION ( 'NONE',  ( 1.000000000000000000, 0.000000000000000000, -0.000000000000000000 ) ) ;
#12798 = CARTESIAN_POINT ( 'NONE',  ( 10.00000000000000000, -37.22597642581161637, 5.202137450156258502 ) ) ;
#12799 = DIRECTION ( 'NONE',  ( 0.000000000000000000, 0.000000000000000000, -1.000000000000000000 ) ) ;
#12800 = AXIS2_PLACEMENT_3D ( 'NONE', #13908, #28830, #43294 ) ;
#12801 = CARTESIAN_POINT ( 'NONE',  ( 10.00000000000000000, -27.13269053701114331, 25.88420570971391754 ) ) ;
#12802 = ORIENTED_EDGE ( 'NONE', *, *, #12118, .T. ) ;
#12803 = LINE ( 'NONE', #42671, #40481 ) ;
#12804 = EDGE_LOOP ( 'NONE', ( #29222, #42099, #26290, #12808 ) ) ;
#12805 = CIRCLE ( 'NONE', #40165, 82.00000000000000000 ) ;
#12806 = DIRECTION ( 'NONE',  ( 0.000000000000000000, 0.000000000000000000, 1.000000000000000000 ) ) ;
#12807 = AXIS2_PLACEMENT_3D ( 'NONE', #12871, #20686, #46883 ) ;
#12808 = ORIENTED_EDGE ( 'NONE', *, *, #26666, .T. ) ;
#12809 = VECTOR ( 'NONE', #30179, 1000.000000000000000 ) ;
#12810 = FACE_OUTER_BOUND ( 'NONE', #9444, .T. ) ;
#12811 = LINE ( 'NONE', #4734, #10991 ) ;
#12812 = DIRECTION ( 'NONE',  ( 0.4796670183876317051, -0.8774505977381971134, 0.000000000000000000 ) ) ;
#12813 = VERTEX_POINT ( 'NONE', #5726 ) ;
#12814 = CARTESIAN_POINT ( 'NONE',  ( -11.59999999999999787, 0.000000000000000000, -54.99999999999998579 ) ) ;
#12815 = CARTESIAN_POINT ( 'NONE',  ( 0.000000000000000000, -24.73286445877757345, 73.44644590900053061 ) ) ;
#12816 = DIRECTION ( 'NONE',  ( 0.000000000000000000, 0.000000000000000000, -1.000000000000000000 ) ) ;
#12817 = DIRECTION ( 'NONE',  ( -1.000000000000000000, 0.000000000000000000, 0.000000000000000000 ) ) ;
#12818 = DIRECTION ( 'NONE',  ( 0.000000000000000000, 0.000000000000000000, 1.000000000000000000 ) ) ;
#12819 = EDGE_CURVE ( 'NONE', #22743, #23433, #358, .T. ) ;
#12820 = AXIS2_PLACEMENT_3D ( 'NONE', #6397, #36249, #17647 ) ;
#12821 = VECTOR ( 'NONE', #3486, 1000.000000000000000 ) ;
#12822 = CARTESIAN_POINT ( 'NONE',  ( 11.99999999999999822, 0.000000000000000000, 0.000000000000000000 ) ) ;
#12823 = DIRECTION ( 'NONE',  ( -1.000000000000000000, 0.000000000000000000, -0.000000000000000000 ) ) ;
#12824 = FACE_OUTER_BOUND ( 'NONE', #3938, .T. ) ;
#12825 = AXIS2_PLACEMENT_3D ( 'NONE', #25732, #40673, #273 ) ;
#12826 = VECTOR ( 'NONE', #38972, 1000.000000000000000 ) ;
#12827 = EDGE_CURVE ( 'NONE', #28374, #29208, #27730, .T. ) ;
#12828 = DIRECTION ( 'NONE',  ( 0.7950889364178796992, -0.6064928550163510845, 0.000000000000000000 ) ) ;
#12829 = LINE ( 'NONE', #24567, #18286 ) ;
#12830 = EDGE_CURVE ( 'NONE', #37280, #12571, #42582, .T. ) ;
#12831 = CIRCLE ( 'NONE', #46436, 31.99999999999998579 ) ;
#12832 = ORIENTED_EDGE ( 'NONE', *, *, #18878, .T. ) ;
#12833 = ORIENTED_EDGE ( 'NONE', *, *, #30510, .T. ) ;
#12834 = DIRECTION ( 'NONE',  ( -1.000000000000000000, 0.000000000000000000, -0.000000000000000000 ) ) ;
#12835 = ORIENTED_EDGE ( 'NONE', *, *, #23805, .T. ) ;
#12836 = CARTESIAN_POINT ( 'NONE',  ( 11.99999999999999822, -51.02545421589363883, 55.20638768913742922 ) ) ;
#12837 = DIRECTION ( 'NONE',  ( -1.000000000000000000, 0.000000000000000000, 0.000000000000000000 ) ) ;
#12838 = EDGE_LOOP ( 'NONE', ( #39572, #13508, #18455, #2377 ) ) ;
#12839 = EDGE_CURVE ( 'NONE', #43487, #21261, #20646, .T. ) ;
#12840 = ADVANCED_FACE ( 'NONE', ( #36055 ), #16269, .T. ) ;
#12841 = CIRCLE ( 'NONE', #44102, 31.99999999999998934 ) ;
#12842 = CIRCLE ( 'NONE', #27698, 42.00000000000000000 ) ;
#12843 = CARTESIAN_POINT ( 'NONE',  ( 0.000000000000000000, 68.55367621811141987, 44.99326035066079044 ) ) ;
#12844 = VERTEX_POINT ( 'NONE', #13076 ) ;
#12845 = CIRCLE ( 'NONE', #26150, 31.99999999999999289 ) ;
#12846 = ORIENTED_EDGE ( 'NONE', *, *, #26268, .F. ) ;
#12847 = ADVANCED_FACE ( 'NONE', ( #35584 ), #12587, .F. ) ;
#12848 = VECTOR ( 'NONE', #1159, 1000.000000000000000 ) ;
#12849 = AXIS2_PLACEMENT_3D ( 'NONE', #48213, #17862, #2690 ) ;
#12850 = DIRECTION ( 'NONE',  ( 0.000000000000000000, 0.9238795325112851842, 0.3826834323650938341 ) ) ;
#12851 = AXIS2_PLACEMENT_3D ( 'NONE', #34961, #11975, #27893 ) ;
#12852 = DIRECTION ( 'NONE',  ( 1.000000000000000000, 0.000000000000000000, 0.000000000000000000 ) ) ;
#12853 = CIRCLE ( 'NONE', #44888, 16.00000000000000000 ) ;
#12854 = DIRECTION ( 'NONE',  ( -0.000000000000000000, -0.2079116908177653378, 0.9781476007338044676 ) ) ;
#12855 = VERTEX_POINT ( 'NONE', #1812 ) ;
#12856 = DIRECTION ( 'NONE',  ( 0.2306669878475637314, 0.9730327541852493711, 0.000000000000000000 ) ) ;
#12857 = VERTEX_POINT ( 'NONE', #16744 ) ;
#12858 = AXIS2_PLACEMENT_3D ( 'NONE', #38175, #19541, #950 ) ;
#12859 = ORIENTED_EDGE ( 'NONE', *, *, #23657, .F. ) ;
#12860 = CARTESIAN_POINT ( 'NONE',  ( 0.000000000000000000, 12.24744871391589207, -2.499999999999994671 ) ) ;
#12861 = DIRECTION ( 'NONE',  ( -1.000000000000000000, 0.000000000000000000, 0.000000000000000000 ) ) ;
#12862 = CARTESIAN_POINT ( 'NONE',  ( 10.00000000000000000, -35.38097989696503021, -12.42422080174676147 ) ) ;
#12863 = ORIENTED_EDGE ( 'NONE', *, *, #30890, .F. ) ;
#12864 = ORIENTED_EDGE ( 'NONE', *, *, #17949, .T. ) ;
#12865 = EDGE_LOOP ( 'NONE', ( #360, #20280, #42560, #25164 ) ) ;
#12866 = CARTESIAN_POINT ( 'NONE',  ( -17.26469406256017791, -140.1601175325492648, 5.500000000000000000 ) ) ;
#12867 = ORIENTED_EDGE ( 'NONE', *, *, #20898, .F. ) ;
#12868 = DIRECTION ( 'NONE',  ( 0.000000000000000000, -0.9876883405951359940, -0.1564344650402420822 ) ) ;
#12869 = DIRECTION ( 'NONE',  ( -0.000000000000000000, -0.000000000000000000, -1.000000000000000000 ) ) ;
#12870 = CARTESIAN_POINT ( 'NONE',  ( 11.99999999999999822, 0.000000000000000000, 0.000000000000000000 ) ) ;
#12871 = CARTESIAN_POINT ( 'NONE',  ( -8.637688417678550223, 13.69818742750669749, -64.01812422950393966 ) ) ;
#12872 = DIRECTION ( 'NONE',  ( 0.000000000000000000, 0.4067366430757989870, 0.9135454576426015327 ) ) ;
#12873 = CARTESIAN_POINT ( 'NONE',  ( 2.500000000000000000, 16.00000000000000000, -19.01812422950394676 ) ) ;
#12874 = CARTESIAN_POINT ( 'NONE',  ( 5.000000000000000000, -39.04073710021356192, 15.48615015657568073 ) ) ;
#12875 = VERTEX_POINT ( 'NONE', #46612 ) ;
#12876 = DIRECTION ( 'NONE',  ( 0.000000000000000000, -0.8526401643540970632, 0.5224985647159409163 ) ) ;
#12877 = CARTESIAN_POINT ( 'NONE',  ( 0.000000000000000000, 0.000000000000000000, 0.000000000000000000 ) ) ;
#12878 = DIRECTION ( 'NONE',  ( -0.9730327541852497042, 0.2306669878475623159, 0.000000000000000000 ) ) ;
#12879 = AXIS2_PLACEMENT_3D ( 'NONE', #38949, #42858, #35254 ) ;
#12880 = DIRECTION ( 'NONE',  ( -1.000000000000000000, 0.000000000000000000, 0.000000000000000000 ) ) ;
#12881 = ORIENTED_EDGE ( 'NONE', *, *, #24862, .T. ) ;
#12882 = CYLINDRICAL_SURFACE ( 'NONE', #1285, 12.49999999999999645 ) ;
#12883 = AXIS2_PLACEMENT_3D ( 'NONE', #37820, #30722, #4776 ) ;
#12884 = AXIS2_PLACEMENT_3D ( 'NONE', #43170, #31933, #20164 ) ;
#12885 = EDGE_CURVE ( 'NONE', #3577, #26816, #19872, .T. ) ;
#12886 = DIRECTION ( 'NONE',  ( 0.000000000000000000, 0.000000000000000000, 1.000000000000000000 ) ) ;
#12887 = CARTESIAN_POINT ( 'NONE',  ( 6.000000000000000000, -29.01471420065506379, -76.69515212746047439 ) ) ;
#12888 = EDGE_CURVE ( 'NONE', #7136, #6878, #32410, .T. ) ;
#12889 = EDGE_CURVE ( 'NONE', #12338, #1784, #19119, .T. ) ;
#12890 = DIRECTION ( 'NONE',  ( 0.000000000000000000, 1.224646799147353207E-16, 1.000000000000000000 ) ) ;
#12891 = FACE_OUTER_BOUND ( 'NONE', #29204, .T. ) ;
#12892 = CIRCLE ( 'NONE', #21472, 82.00000000000000000 ) ;
#12893 = AXIS2_PLACEMENT_3D ( 'NONE', #25094, #35876, #10168 ) ;
#12894 = CARTESIAN_POINT ( 'NONE',  ( -2.977765906491215642, 0.000000000000000000, -15.77977592589476608 ) ) ;
#12895 = DIRECTION ( 'NONE',  ( -1.000000000000000000, 0.000000000000000000, 0.000000000000000000 ) ) ;
#12897 = EDGE_CURVE ( 'NONE', #13811, #28502, #41776, .T. ) ;
#12896 = ORIENTED_EDGE ( 'NONE', *, *, #46418, .F. ) ;
#12898 = AXIS2_PLACEMENT_3D ( 'NONE', #25140, #32727, #47648 ) ;
#12899 = CARTESIAN_POINT ( 'NONE',  ( 10.00000000000000000, 0.000000000000000000, 0.000000000000000000 ) ) ;
#12900 = CIRCLE ( 'NONE', #47271, 82.00000000000000000 ) ;
#12901 = CIRCLE ( 'NONE', #35565, 16.00000000000000000 ) ;
#12902 = ORIENTED_EDGE ( 'NONE', *, *, #35405, .F. ) ;
#12903 = CARTESIAN_POINT ( 'NONE',  ( 0.000000000000000000, 0.000000000000000000, 0.000000000000000000 ) ) ;
#12904 = CIRCLE ( 'NONE', #26164, 31.99999999999999289 ) ;
#12905 = EDGE_LOOP ( 'NONE', ( #5275, #12122, #1140, #32700 ) ) ;
#12906 = EDGE_CURVE ( 'NONE', #28234, #46631, #25754, .T. ) ;
#12907 = ORIENTED_EDGE ( 'NONE', *, *, #5937, .T. ) ;
#12908 = EDGE_CURVE ( 'NONE', #31098, #16116, #6927, .T. ) ;
#12909 = ORIENTED_EDGE ( 'NONE', *, *, #8241, .T. ) ;
#12910 = LINE ( 'NONE', #9456, #45268 ) ;
#12911 = ORIENTED_EDGE ( 'NONE', *, *, #47579, .T. ) ;
#12912 = EDGE_CURVE ( 'NONE', #22184, #41493, #6693, .T. ) ;
#12913 = VECTOR ( 'NONE', #27384, 1000.000000000000000 ) ;
#12914 = LINE ( 'NONE', #34930, #10911 ) ;
#12915 = AXIS2_PLACEMENT_3D ( 'NONE', #21880, #18457, #86 ) ;
#12916 = DIRECTION ( 'NONE',  ( -1.000000000000000000, 0.000000000000000000, 0.000000000000000000 ) ) ;
#12917 = ORIENTED_EDGE ( 'NONE', *, *, #12885, .F. ) ;
#12918 = ORIENTED_EDGE ( 'NONE', *, *, #14929, .F. ) ;
#12919 = DIRECTION ( 'NONE',  ( -1.000000000000000000, -0.000000000000000000, 0.000000000000000000 ) ) ;
#12921 = VERTEX_POINT ( 'NONE', #7414 ) ;
#12920 = CARTESIAN_POINT ( 'NONE',  ( 0.000000000000000000, -17.28742895386031719, -75.54627589209962935 ) ) ;
#12922 = EDGE_CURVE ( 'NONE', #13574, #29150, #1130, .T. ) ;
#12923 = DIRECTION ( 'NONE',  ( -1.000000000000000000, 0.000000000000000000, 0.000000000000000000 ) ) ;
#12924 = CIRCLE ( 'NONE', #7429, 42.00000000000000000 ) ;
#12925 = AXIS2_PLACEMENT_3D ( 'NONE', #48060, #21386, #33131 ) ;
#12926 = VERTEX_POINT ( 'NONE', #18161 ) ;
#12927 = DIRECTION ( 'NONE',  ( -1.000000000000000000, 0.000000000000000000, -0.000000000000000000 ) ) ;
#12928 = VERTEX_POINT ( 'NONE', #40470 ) ;
#12929 = EDGE_LOOP ( 'NONE', ( #27132, #39761, #8839, #32115 ) ) ;
#12930 = DIRECTION ( 'NONE',  ( 0.000000000000000000, 0.000000000000000000, 1.000000000000000000 ) ) ;
#12931 = DIRECTION ( 'NONE',  ( -0.000000000000000000, -0.000000000000000000, -1.000000000000000000 ) ) ;
#12932 = ORIENTED_EDGE ( 'NONE', *, *, #45666, .T. ) ;
#12933 = AXIS2_PLACEMENT_3D ( 'NONE', #48429, #40143, #23165 ) ;
#12934 = DIRECTION ( 'NONE',  ( 0.000000000000000000, -0.5877852522924803536, 0.8090169943749422332 ) ) ;
#12935 = DIRECTION ( 'NONE',  ( 0.000000000000000000, -0.9876883405951393247, 0.1564344650402205161 ) ) ;
#12936 = CARTESIAN_POINT ( 'NONE',  ( 11.99999999999999822, -55.19960302592104284, 51.03279382321070301 ) ) ;
#12938 = ORIENTED_EDGE ( 'NONE', *, *, #32443, .T. ) ;
#12937 = AXIS2_PLACEMENT_3D ( 'NONE', #22847, #40730, #3271 ) ;
#12939 = AXIS2_PLACEMENT_3D ( 'NONE', #37171, #3141, #18323 ) ;
#12940 = EDGE_LOOP ( 'NONE', ( #9152, #36255, #25407, #46641 ) ) ;
#12941 = CARTESIAN_POINT ( 'NONE',  ( 5.000000000000002665, 80.55351364060611274, -15.33399622253396544 ) ) ;
#12942 = CARTESIAN_POINT ( 'NONE',  ( 0.000000000000000000, -15.33399622253541317, 80.55351364060584274 ) ) ;
#12943 = VECTOR ( 'NONE', #29436, 1000.000000000000000 ) ;
#12944 = ORIENTED_EDGE ( 'NONE', *, *, #48300, .T. ) ;
#12945 = EDGE_CURVE ( 'NONE', #15777, #25011, #10115, .T. ) ;
#12946 = CARTESIAN_POINT ( 'NONE',  ( 10.00000000000000000, 0.9569279952884607310, 2.500000000000015543 ) ) ;
#12947 = ORIENTED_EDGE ( 'NONE', *, *, #15294, .T. ) ;
#12948 = FACE_OUTER_BOUND ( 'NONE', #11534, .T. ) ;
#12949 = ADVANCED_FACE ( 'NONE', ( #37016 ), #25517, .T. ) ;
#12950 = CARTESIAN_POINT ( 'NONE',  ( 12.00000000000000000, -23.29833615347109088, -3.418703333116486665 ) ) ;
#12951 = CARTESIAN_POINT ( 'NONE',  ( 0.000000000000000000, 0.000000000000000000, 0.000000000000000000 ) ) ;
#12952 = CIRCLE ( 'NONE', #8210, 31.99999999999999289 ) ;
#12953 = DIRECTION ( 'NONE',  ( -1.000000000000000000, 0.000000000000000000, -0.000000000000000000 ) ) ;
#12954 = ADVANCED_FACE ( 'NONE', ( #48037 ), #29194, .T. ) ;
#12955 = DIRECTION ( 'NONE',  ( 0.000000000000000000, 0.7604059656000322631, -0.6494480483301821039 ) ) ;
#12956 = CARTESIAN_POINT ( 'NONE',  ( -10.00000000000000000, 0.000000000000000000, 0.000000000000000000 ) ) ;
#12957 = CIRCLE ( 'NONE', #36377, 31.99999999999998224 ) ;
#12958 = CARTESIAN_POINT ( 'NONE',  ( 0.000000000000000000, 0.000000000000000000, 42.00000000000001421 ) ) ;
#12959 = DIRECTION ( 'NONE',  ( 0.000000000000000000, 0.000000000000000000, 1.000000000000000000 ) ) ;
#12960 = CYLINDRICAL_SURFACE ( 'NONE', #34796, 16.00000000000000000 ) ;
#12961 = EDGE_CURVE ( 'NONE', #29904, #36506, #38674, .T. ) ;
#12962 = DIRECTION ( 'NONE',  ( -1.000000000000000000, 0.000000000000000000, 0.000000000000000000 ) ) ;
#12963 =( NAMED_UNIT ( * ) PLANE_ANGLE_UNIT ( ) SI_UNIT ( $, .RADIAN. ) );
#12964 = ORIENTED_EDGE ( 'NONE', *, *, #7177, .T. ) ;
#12965 = AXIS2_PLACEMENT_3D ( 'NONE', #46572, #13041, #27974 ) ;
#12966 = AXIS2_PLACEMENT_3D ( 'NONE', #43620, #33072, #13282 ) ;
#12967 = ORIENTED_EDGE ( 'NONE', *, *, #42773, .T. ) ;
#12968 = ORIENTED_EDGE ( 'NONE', *, *, #11664, .F. ) ;
#12969 = VECTOR ( 'NONE', #10398, 1000.000000000000000 ) ;
#12970 = DIRECTION ( 'NONE',  ( -1.000000000000000000, -0.000000000000000000, 0.000000000000000000 ) ) ;
#12971 = CARTESIAN_POINT ( 'NONE',  ( 0.000000000000000000, 16.45098606841173705, -33.79645857604496229 ) ) ;
#12972 = CIRCLE ( 'NONE', #30161, 16.00000000000000355 ) ;
#12973 = ORIENTED_EDGE ( 'NONE', *, *, #16747, .T. ) ;
#12974 = FACE_OUTER_BOUND ( 'NONE', #15903, .T. ) ;
#12975 = ORIENTED_EDGE ( 'NONE', *, *, #721, .F. ) ;
#12976 = EDGE_LOOP ( 'NONE', ( #717, #13098, #30977, #42853 ) ) ;
#12977 = CIRCLE ( 'NONE', #46591, 37.49900000000001654 ) ;
#12978 = ORIENTED_EDGE ( 'NONE', *, *, #36932, .T. ) ;
#12979 = VECTOR ( 'NONE', #3053, 1000.000000000000000 ) ;
#12980 = CIRCLE ( 'NONE', #36416, 82.00000000000000000 ) ;
#12981 = DIRECTION ( 'NONE',  ( 0.000000000000000000, 0.000000000000000000, -1.000000000000000000 ) ) ;
#12982 = ORIENTED_EDGE ( 'NONE', *, *, #20177, .F. ) ;
#12983 = ORIENTED_EDGE ( 'NONE', *, *, #29319, .F. ) ;
#12984 = DIRECTION ( 'NONE',  ( 0.9781476007338070211, 0.000000000000000000, -0.2079116908177527367 ) ) ;
#12985 = ORIENTED_EDGE ( 'NONE', *, *, #1238, .F. ) ;
#12986 = DIRECTION ( 'NONE',  ( 1.000000000000000000, -0.000000000000000000, -0.000000000000000000 ) ) ;
#12987 = DIRECTION ( 'NONE',  ( 0.1850432970638656582, -0.9827303690289285187, 0.000000000000000000 ) ) ;
#12988 = DIRECTION ( 'NONE',  ( 0.000000000000000000, -0.3090169943749548342, 0.9510565162951510887 ) ) ;
#12989 = CIRCLE ( 'NONE', #20804, 37.49900000000001654 ) ;
#12990 = ORIENTED_EDGE ( 'NONE', *, *, #11015, .F. ) ;
#12991 = DIRECTION ( 'NONE',  ( 0.000000000000000000, 0.000000000000000000, 1.000000000000000000 ) ) ;
#12992 = ORIENTED_EDGE ( 'NONE', *, *, #22877, .T. ) ;
#12993 = LINE ( 'NONE', #42849, #21121 ) ;
#12994 = CYLINDRICAL_SURFACE ( 'NONE', #6320, 77.49899999999999523 ) ;
#12995 = CIRCLE ( 'NONE', #2026, 17.37152077436032371 ) ;
#12996 = FACE_OUTER_BOUND ( 'NONE', #44737, .T. ) ;
#12997 = VERTEX_POINT ( 'NONE', #29677 ) ;
#12998 = ORIENTED_EDGE ( 'NONE', *, *, #1281, .T. ) ;
#12999 = EDGE_CURVE ( 'NONE', #956, #17342, #7162, .T. ) ;
#13000 = DIRECTION ( 'NONE',  ( 0.000000000000000000, -0.9510565162951566398, 0.3090169943749380144 ) ) ;
#13001 = CYLINDRICAL_SURFACE ( 'NONE', #22284, 16.00000000000000000 ) ;
#13002 = ORIENTED_EDGE ( 'NONE', *, *, #39937, .F. ) ;
#13003 = CARTESIAN_POINT ( 'NONE',  ( 11.99999999999999822, -74.65374052328644439, -8.840884882375878107 ) ) ;
#13004 = AXIS2_PLACEMENT_3D ( 'NONE', #21350, #16967, #2988 ) ;
#13005 = DIRECTION ( 'NONE',  ( -1.000000000000000000, 0.000000000000000000, 0.000000000000000000 ) ) ;
#13006 = DIRECTION ( 'NONE',  ( -1.000000000000000000, -0.000000000000000000, -0.000000000000000000 ) ) ;
#13007 = ORIENTED_EDGE ( 'NONE', *, *, #38456, .F. ) ;
#13008 = ADVANCED_FACE ( 'NONE', ( #25037 ), #3495, .T. ) ;
#13009 = CARTESIAN_POINT ( 'NONE',  ( -103.9230484541323705, -180.0000000000004832, -5.500000000000000000 ) ) ;
#13010 = DIRECTION ( 'NONE',  ( 0.000000000000000000, -0.9510565162951565288, 0.3090169943749384029 ) ) ;
#13011 = CARTESIAN_POINT ( 'NONE',  ( 10.00000000000000000, -6.555932627142143865, -37.01155633439065440 ) ) ;
#13012 = VERTEX_POINT ( 'NONE', #32401 ) ;
#13013 = CARTESIAN_POINT ( 'NONE',  ( 0.000000000000000000, 0.000000000000000000, 0.000000000000000000 ) ) ;
#13014 = CARTESIAN_POINT ( 'NONE',  ( 10.00000000000000000, 56.15606465354958488, 59.75363087400094031 ) ) ;
#13015 = CARTESIAN_POINT ( 'NONE',  ( 0.000000000000000000, 27.74655509720669500, 77.16300072079670258 ) ) ;
#13016 = ADVANCED_FACE ( 'NONE', ( #47327 ), #13801, .T. ) ;
#13017 = AXIS2_PLACEMENT_3D ( 'NONE', #35024, #31866, #12760 ) ;
#13018 = ADVANCED_FACE ( 'NONE', ( #6445 ), #32628, .T. ) ;
#13019 = LINE ( 'NONE', #20102, #20537 ) ;
#13020 = CARTESIAN_POINT ( 'NONE',  ( 0.000000000000000000, 50.23322058963348979, 64.81221759200361987 ) ) ;
#13021 = DIRECTION ( 'NONE',  ( -1.000000000000000000, -0.000000000000000000, -0.000000000000000000 ) ) ;
#13022 = FACE_OUTER_BOUND ( 'NONE', #6425, .T. ) ;
#13023 = ORIENTED_EDGE ( 'NONE', *, *, #19007, .F. ) ;
#13024 = ORIENTED_EDGE ( 'NONE', *, *, #39065, .T. ) ;
#13025 = AXIS2_PLACEMENT_3D ( 'NONE', #1203, #20038, #42316 ) ;
#13026 = CYLINDRICAL_SURFACE ( 'NONE', #15149, 82.00000000000000000 ) ;
#13027 = DIRECTION ( 'NONE',  ( -1.000000000000000000, 0.000000000000000000, 0.000000000000000000 ) ) ;
#13028 = ADVANCED_FACE ( 'NONE', ( #21622 ), #3004, .T. ) ;
#13029 = CARTESIAN_POINT ( 'NONE',  ( 0.4966694826857007139, -118.5846133302278247, 2.500000000000000000 ) ) ;
#13030 = ORIENTED_EDGE ( 'NONE', *, *, #35049, .T. ) ;
#13031 = CIRCLE ( 'NONE', #46636, 16.00000000000000000 ) ;
#13032 = DIRECTION ( 'NONE',  ( 0.000000000000000000, -0.8090169943749497827, -0.5877852522924698064 ) ) ;
#13033 = CARTESIAN_POINT ( 'NONE',  ( 10.00000000000000000, -35.92658777277517856, 10.74501242461269257 ) ) ;
#13034 = AXIS2_PLACEMENT_3D ( 'NONE', #41647, #34288, #38954 ) ;
#13035 = ORIENTED_EDGE ( 'NONE', *, *, #33647, .T. ) ;
#13036 = EDGE_CURVE ( 'NONE', #28215, #26631, #4471, .T. ) ;
#13037 = DIRECTION ( 'NONE',  ( -1.000000000000000000, -0.000000000000000000, -0.000000000000000000 ) ) ;
#13038 = CIRCLE ( 'NONE', #16939, 31.99999999999998579 ) ;
#13039 = DIRECTION ( 'NONE',  ( 0.000000000000000000, 0.000000000000000000, 1.000000000000000000 ) ) ;
#13040 = VERTEX_POINT ( 'NONE', #34541 ) ;
#13041 = DIRECTION ( 'NONE',  ( -1.000000000000000000, 0.000000000000000000, 0.000000000000000000 ) ) ;
#13042 = EDGE_CURVE ( 'NONE', #15966, #21714, #20699, .T. ) ;
#13043 = ORIENTED_EDGE ( 'NONE', *, *, #5466, .T. ) ;
#13044 = ORIENTED_EDGE ( 'NONE', *, *, #3501, .F. ) ;
#13045 = MECHANICAL_DESIGN_GEOMETRIC_PRESENTATION_REPRESENTATION (  '', ( #26317 ), #19277 ) ;
#13046 = DIRECTION ( 'NONE',  ( -1.000000000000000000, 0.000000000000000000, 0.000000000000000000 ) ) ;
#13047 = EDGE_CURVE ( 'NONE', #36756, #15863, #8191, .T. ) ;
#13048 = CARTESIAN_POINT ( 'NONE',  ( 10.00000000000000000, 16.95692799528845995, 2.500000000000000000 ) ) ;
#13049 = DIRECTION ( 'NONE',  ( 0.000000000000000000, -0.3090169943749548342, 0.9510565162951511997 ) ) ;
#13050 = DIRECTION ( 'NONE',  ( 0.000000000000000000, 0.3090169943749450088, -0.9510565162951544194 ) ) ;
#13051 = DIRECTION ( 'NONE',  ( 0.000000000000000000, 0.000000000000000000, 1.000000000000000000 ) ) ;
#13052 = ORIENTED_EDGE ( 'NONE', *, *, #3603, .F. ) ;
#13053 = DIRECTION ( 'NONE',  ( 0.000000000000000000, 0.000000000000000000, 1.000000000000000000 ) ) ;
#13054 = VERTEX_POINT ( 'NONE', #30647 ) ;
#13055 = CARTESIAN_POINT ( 'NONE',  ( -10.00000000000000000, 0.000000000000000000, 0.000000000000000000 ) ) ;
#13056 = CARTESIAN_POINT ( 'NONE',  ( 10.00000000000000000, 12.93880638057314059, 76.41127070299278046 ) ) ;
#13057 = CARTESIAN_POINT ( 'NONE',  ( 0.000000000000000000, -79.10210256391353312, -21.60688246758668640 ) ) ;
#13058 = CARTESIAN_POINT ( 'NONE',  ( 0.000000000000000000, 0.000000000000000000, 42.00000000000001421 ) ) ;
#13059 = ORIENTED_EDGE ( 'NONE', *, *, #2245, .T. ) ;
#13060 = DIRECTION ( 'NONE',  ( -1.000000000000000000, -0.000000000000000000, -0.000000000000000000 ) ) ;
#13061 = EDGE_CURVE ( 'NONE', #39405, #19937, #41809, .T. ) ;
#13062 = CARTESIAN_POINT ( 'NONE',  ( 10.00000000000000000, 75.11725578898472122, -2.956366410619845730 ) ) ;
#13063 = ADVANCED_FACE ( 'NONE', ( #11575, #19144, #4229, #12061, #8376, #45563, #15964, #11807, #23302, #26990, #3983, #23061, #550, #30414, #38236, #19376, #19608 ), #30906, .F. ) ;
#13064 = EDGE_CURVE ( 'NONE', #22172, #14427, #18888, .T. ) ;
#13065 = CARTESIAN_POINT ( 'NONE',  ( 0.000000000000000000, -54.21277698773636899, -55.38113227695839669 ) ) ;
#13066 = DIRECTION ( 'NONE',  ( -1.000000000000000000, 0.000000000000000000, -0.000000000000000000 ) ) ;
#13067 = CARTESIAN_POINT ( 'NONE',  ( 10.00000000000000000, 0.000000000000000000, 0.000000000000000000 ) ) ;
#13068 = AXIS2_PLACEMENT_3D ( 'NONE', #22902, #4551, #23381 ) ;
#13069 = DIRECTION ( 'NONE',  ( 1.000000000000000000, -0.000000000000000000, 0.000000000000000000 ) ) ;
#13070 = CYLINDRICAL_SURFACE ( 'NONE', #21244, 31.99999999999999289 ) ;
#13071 = DIRECTION ( 'NONE',  ( 0.000000000000000000, 0.000000000000000000, 1.000000000000000000 ) ) ;
#13072 = AXIS2_PLACEMENT_3D ( 'NONE', #19781, #8048, #11736 ) ;
#13073 = FACE_OUTER_BOUND ( 'NONE', #6281, .T. ) ;
#13074 = FACE_OUTER_BOUND ( 'NONE', #22831, .T. ) ;
#13075 = VERTEX_POINT ( 'NONE', #8128 ) ;
#13076 = CARTESIAN_POINT ( 'NONE',  ( 0.000000000000000000, 60.67117009219216328, -55.16347631942977614 ) ) ;
#13077 = CIRCLE ( 'NONE', #29487, 77.49899999999998101 ) ;
#13078 = EDGE_LOOP ( 'NONE', ( #17891, #26992, #46119, #14165 ) ) ;
#13079 = DIRECTION ( 'NONE',  ( 0.000000000000000000, 0.000000000000000000, 1.000000000000000000 ) ) ;
#13080 = DIRECTION ( 'NONE',  ( 0.000000000000000000, 0.000000000000000000, 1.000000000000000000 ) ) ;
#13081 = VERTEX_POINT ( 'NONE', #295 ) ;
#13082 = CIRCLE ( 'NONE', #8384, 82.00000000000000000 ) ;
#13083 = LINE ( 'NONE', #9163, #368 ) ;
#13084 = ORIENTED_EDGE ( 'NONE', *, *, #31893, .F. ) ;
#13085 = ORIENTED_EDGE ( 'NONE', *, *, #12478, .T. ) ;
#13086 = EDGE_CURVE ( 'NONE', #23062, #25598, #26262, .T. ) ;
#13087 = CIRCLE ( 'NONE', #13865, 31.99999999999998579 ) ;
#13088 = EDGE_CURVE ( 'NONE', #39316, #40825, #39471, .T. ) ;
#13089 = FACE_OUTER_BOUND ( 'NONE', #12722, .T. ) ;
#13090 = DIRECTION ( 'NONE',  ( -1.000000000000000000, -0.000000000000000000, -0.000000000000000000 ) ) ;
#13091 = PLANE ( 'NONE',  #4337 ) ;
#13092 = ADVANCED_FACE ( 'NONE', ( #15001 ), #42144, .F. ) ;
#13093 = ORIENTED_EDGE ( 'NONE', *, *, #13205, .F. ) ;
#13094 = CIRCLE ( 'NONE', #45134, 31.99999999999998579 ) ;
#13095 = CARTESIAN_POINT ( 'NONE',  ( -3.000000000000000000, 14.60985201121729737, -18.46759930825687945 ) ) ;
#13096 = EDGE_LOOP ( 'NONE', ( #18894, #28701, #24154, #9692 ) ) ;
#13097 = EDGE_CURVE ( 'NONE', #9519, #26793, #41200, .T. ) ;
#13098 = ORIENTED_EDGE ( 'NONE', *, *, #11228, .F. ) ;
#13099 = DIRECTION ( 'NONE',  ( 0.000000000000000000, -0.7604059656000369261, 0.6494480483301766638 ) ) ;
#13100 = DIRECTION ( 'NONE',  ( -1.000000000000000000, 0.000000000000000000, 0.000000000000000000 ) ) ;
#13101 = CARTESIAN_POINT ( 'NONE',  ( 10.00000000000000000, 22.74946021919133088, 29.81001611431016229 ) ) ;
#13102 = ORIENTED_EDGE ( 'NONE', *, *, #26628, .T. ) ;
#13103 = VECTOR ( 'NONE', #283, 999.9999999999998863 ) ;
#13104 = VERTEX_POINT ( 'NONE', #37505 ) ;
#13105 = DIRECTION ( 'NONE',  ( 0.2306669878475623159, 0.9730327541852497042, -0.000000000000000000 ) ) ;
#13106 = ORIENTED_EDGE ( 'NONE', *, *, #16689, .F. ) ;
#13107 = FACE_OUTER_BOUND ( 'NONE', #42765, .T. ) ;
#13108 = LINE ( 'NONE', #16781, #45681 ) ;
#13109 = DIRECTION ( 'NONE',  ( -0.8774505977381983346, -0.4796670183876294291, 0.000000000000000000 ) ) ;
#13110 = CARTESIAN_POINT ( 'NONE',  ( 0.000000000000000000, 0.000000000000000000, 0.000000000000000000 ) ) ;
#13111 = DIRECTION ( 'NONE',  ( 0.000000000000000000, 0.000000000000000000, 1.000000000000000000 ) ) ;
#13112 = DIRECTION ( 'NONE',  ( 0.000000000000000000, -0.2334453638558922628, -0.9723699203976798877 ) ) ;
#13113 = DIRECTION ( 'NONE',  ( 1.000000000000000000, 0.000000000000000000, 0.000000000000000000 ) ) ;
#13114 = EDGE_CURVE ( 'NONE', #22226, #26939, #33823, .T. ) ;
#13115 = ORIENTED_EDGE ( 'NONE', *, *, #42534, .F. ) ;
#13116 = EDGE_CURVE ( 'NONE', #34190, #46809, #45101, .T. ) ;
#13117 = CARTESIAN_POINT ( 'NONE',  ( -3.000000000000000000, 14.60985201121704513, 18.46759930825707841 ) ) ;
#13118 = DIRECTION ( 'NONE',  ( 0.000000000000000000, 1.000000000000000000, 0.000000000000000000 ) ) ;
#13119 = AXIS2_PLACEMENT_3D ( 'NONE', #17629, #36942, #37200 ) ;
#13120 = DIRECTION ( 'NONE',  ( 0.000000000000000000, 0.000000000000000000, -1.000000000000000000 ) ) ;
#13121 = LINE ( 'NONE', #27088, #20750 ) ;
#13122 = VERTEX_POINT ( 'NONE', #20336 ) ;
#13123 = FILL_AREA_STYLE ('',( #28279 ) ) ;
#13124 = CYLINDRICAL_SURFACE ( 'NONE', #10298, 31.99999999999998579 ) ;
#13125 = DIRECTION ( 'NONE',  ( 0.5200609990132993854, 0.8541291221503275466, -0.000000000000000000 ) ) ;
#13126 = DIRECTION ( 'NONE',  ( 1.000000000000000000, 0.000000000000000000, 0.000000000000000000 ) ) ;
#13127 = DIRECTION ( 'NONE',  ( -1.000000000000000000, -0.000000000000000000, 0.000000000000000000 ) ) ;
#13128 = EDGE_CURVE ( 'NONE', #844, #17342, #12005, .T. ) ;
#13129 = AXIS2_PLACEMENT_3D ( 'NONE', #36270, #3207, #10815 ) ;
#13130 = CARTESIAN_POINT ( 'NONE',  ( 0.000000000000000000, 0.000000000000000000, 0.000000000000000000 ) ) ;
#13131 = DIRECTION ( 'NONE',  ( -1.000000000000000000, -0.000000000000000000, -0.000000000000000000 ) ) ;
#13132 = ORIENTED_EDGE ( 'NONE', *, *, #25564, .T. ) ;
#13133 = DIRECTION ( 'NONE',  ( -1.000000000000000000, 0.000000000000000000, 0.000000000000000000 ) ) ;
#13134 = CIRCLE ( 'NONE', #47497, 16.00000000000000000 ) ;
#13135 = VERTEX_POINT ( 'NONE', #31144 ) ;
#13136 = AXIS2_PLACEMENT_3D ( 'NONE', #18254, #21198, #29286 ) ;
#13137 = DIRECTION ( 'NONE',  ( 0.000000000000000000, 0.4539904997395412534, 0.8910065241883706744 ) ) ;
#13138 = ORIENTED_EDGE ( 'NONE', *, *, #770, .F. ) ;
#13139 = EDGE_LOOP ( 'NONE', ( #7482, #21531, #26753, #19634 ) ) ;
#13140 = ORIENTED_EDGE ( 'NONE', *, *, #7660, .F. ) ;
#13141 = DIRECTION ( 'NONE',  ( 0.000000000000000000, 0.000000000000000000, 1.000000000000000000 ) ) ;
#13142 = ORIENTED_EDGE ( 'NONE', *, *, #23288, .T. ) ;
#13143 = CIRCLE ( 'NONE', #3740, 77.49899999999999523 ) ;
#13144 = VERTEX_POINT ( 'NONE', #31633 ) ;
#13145 = CARTESIAN_POINT ( 'NONE',  ( 0.000000000000000000, 0.000000000000000000, 0.000000000000000000 ) ) ;
#13146 = DIRECTION ( 'NONE',  ( -1.000000000000000000, -0.000000000000000000, 0.000000000000000000 ) ) ;
#13147 = ADVANCED_FACE ( 'NONE', ( #42879 ), #13026, .T. ) ;
#13148 = VERTEX_POINT ( 'NONE', #46066 ) ;
#13149 = VERTEX_POINT ( 'NONE', #23781 ) ;
#13150 = EDGE_CURVE ( 'NONE', #3749, #45952, #16681, .T. ) ;
#13151 = LINE ( 'NONE', #27357, #39735 ) ;
#13153 = ORIENTED_EDGE ( 'NONE', *, *, #40118, .T. ) ;
#13152 = CARTESIAN_POINT ( 'NONE',  ( 0.000000000000000000, -36.13751322684404244, -21.40280677340410165 ) ) ;
#13154 = CYLINDRICAL_SURFACE ( 'NONE', #39190, 21.00000000000000000 ) ;
#13155 = VERTEX_POINT ( 'NONE', #28173 ) ;
#13156 = ORIENTED_EDGE ( 'NONE', *, *, #33765, .F. ) ;
#13157 = CARTESIAN_POINT ( 'NONE',  ( 7.543218489614351263, -11.91259227951415056, -1.199999999999999956 ) ) ;
#13158 = EDGE_CURVE ( 'NONE', #45459, #9046, #20839, .T. ) ;
#13159 = VERTEX_POINT ( 'NONE', #13253 ) ;
#13160 = LINE ( 'NONE', #31788, #47803 ) ;
#13161 = FACE_OUTER_BOUND ( 'NONE', #20605, .T. ) ;
#13162 = CIRCLE ( 'NONE', #40521, 77.49899999999999523 ) ;
#13163 = DIRECTION ( 'NONE',  ( 0.000000000000000000, 0.000000000000000000, 1.000000000000000000 ) ) ;
#13164 = CARTESIAN_POINT ( 'NONE',  ( -11.63999999999999702, 0.000000000000000000, 0.000000000000000000 ) ) ;
#13165 = CARTESIAN_POINT ( 'NONE',  ( 0.000000000000000000, 3.894527615417885169, 81.90746397400390322 ) ) ;
#13166 = CIRCLE ( 'NONE', #17069, 31.99999999999997868 ) ;
#13167 = ORIENTED_EDGE ( 'NONE', *, *, #28339, .F. ) ;
#13168 = ORIENTED_EDGE ( 'NONE', *, *, #16492, .T. ) ;
#13169 = EDGE_CURVE ( 'NONE', #12299, #9209, #2010, .T. ) ;
#13170 = LINE ( 'NONE', #42797, #3984 ) ;
#13171 = FACE_OUTER_BOUND ( 'NONE', #38080, .T. ) ;
#13172 = ORIENTED_EDGE ( 'NONE', *, *, #46546, .F. ) ;
#13173 = EDGE_CURVE ( 'NONE', #34848, #3678, #9640, .T. ) ;
#13174 = CARTESIAN_POINT ( 'NONE',  ( 6.000000000000000000, -2.543863470248951320, 81.96053171279901051 ) ) ;
#13175 = ORIENTED_EDGE ( 'NONE', *, *, #26594, .T. ) ;
#13176 = CARTESIAN_POINT ( 'NONE',  ( 2.047646702416564768, -96.54137380445985173, 2.500000000000000000 ) ) ;
#13177 = FACE_OUTER_BOUND ( 'NONE', #39704, .T. ) ;
#13178 = LINE ( 'NONE', #28106, #30076 ) ;
#13179 = AXIS2_PLACEMENT_3D ( 'NONE', #14204, #29377, #44303 ) ;
#13180 = DIRECTION ( 'NONE',  ( 1.000000000000000000, -0.000000000000000000, -0.000000000000000000 ) ) ;
#13181 = VERTEX_POINT ( 'NONE', #27958 ) ;
#13182 = SURFACE_SIDE_STYLE ('',( #9028 ) ) ;
#13183 = CIRCLE ( 'NONE', #2233, 16.00000000000000355 ) ;
#13184 = DIRECTION ( 'NONE',  ( -1.000000000000000000, -0.000000000000000000, 0.000000000000000000 ) ) ;
#13185 = EDGE_CURVE ( 'NONE', #44456, #36840, #14337, .T. ) ;
#13186 = VERTEX_POINT ( 'NONE', #5197 ) ;
#13187 = CARTESIAN_POINT ( 'NONE',  ( -3.000000000000000000, -1.278221433540145391, -26.51162292216073979 ) ) ;
#13188 = CARTESIAN_POINT ( 'NONE',  ( 0.000000000000000000, -37.58145647212455032, 16.68533520207890319 ) ) ;
#13189 = LINE ( 'NONE', #17091, #38769 ) ;
#13190 = ORIENTED_EDGE ( 'NONE', *, *, #19572, .F. ) ;
#13191 = LINE ( 'NONE', #42818, #37812 ) ;
#13192 =( LENGTH_UNIT ( ) NAMED_UNIT ( * ) SI_UNIT ( .MILLI., .METRE. ) );
#13193 = VERTEX_POINT ( 'NONE', #46553 ) ;
#13194 = VERTEX_POINT ( 'NONE', #16213 ) ;
#13195 = VERTEX_POINT ( 'NONE', #5668 ) ;
#13196 = AXIS2_PLACEMENT_3D ( 'NONE', #43740, #6537, #32952 ) ;
#13197 = AXIS2_PLACEMENT_3D ( 'NONE', #32726, #3099, #40561 ) ;
#13198 = DIRECTION ( 'NONE',  ( -1.000000000000000000, -0.000000000000000000, -0.000000000000000000 ) ) ;
#13199 = CARTESIAN_POINT ( 'NONE',  ( 0.000000000000000000, 2.571758278209441661E-15, -21.00000000000000000 ) ) ;
#13200 = AXIS2_PLACEMENT_3D ( 'NONE', #1840, #46871, #19686 ) ;
#13201 = ORIENTED_EDGE ( 'NONE', *, *, #14653, .T. ) ;
#13202 = ADVANCED_FACE ( 'NONE', ( #2228 ), #35525, .T. ) ;
#13203 = FACE_OUTER_BOUND ( 'NONE', #12746, .T. ) ;
#13204 = CYLINDRICAL_SURFACE ( 'NONE', #37886, 31.99999999999998579 ) ;
#13205 = EDGE_CURVE ( 'NONE', #34289, #31027, #34662, .T. ) ;
#13206 = EDGE_LOOP ( 'NONE', ( #18907, #46388, #14710, #45050 ) ) ;
#13207 = ORIENTED_EDGE ( 'NONE', *, *, #4353, .T. ) ;
#13208 = VERTEX_POINT ( 'NONE', #43112 ) ;
#13209 = ORIENTED_EDGE ( 'NONE', *, *, #44991, .T. ) ;
#13210 = PRODUCT ( 'fast gear_ISO - Spur gear 2M 40T 20PA 10FW ---S40A75H50L38.0N', 'fast gear_ISO - Spur gear 2M 40T 20PA 10FW ---S40A75H50L38.0N', '', ( #23787 ) ) ;
#13211 = EDGE_CURVE ( 'NONE', #30765, #19987, #36238, .T. ) ;
#13212 = ADVANCED_FACE ( 'NONE', ( #39447 ), #5427, .T. ) ;
#13213 = CARTESIAN_POINT ( 'NONE',  ( 2.874421927457452952, -143.3717286177755739, -2.500000000000000000 ) ) ;
#13214 = EDGE_CURVE ( 'NONE', #46211, #12014, #6550, .T. ) ;
#13215 = EDGE_LOOP ( 'NONE', ( #22049, #4956, #14430, #47154 ) ) ;
#13216 = CARTESIAN_POINT ( 'NONE',  ( 0.000000000000000000, 0.000000000000000000, 52.00000000000002132 ) ) ;
#13217 = EDGE_CURVE ( 'NONE', #10347, #11083, #47182, .T. ) ;
#13218 = ORIENTED_EDGE ( 'NONE', *, *, #30848, .T. ) ;
#13219 = APPLICATION_CONTEXT ( 'automotive_design' ) ;
#13220 = CARTESIAN_POINT ( 'NONE',  ( 0.000000000000000000, 0.000000000000000000, 0.000000000000000000 ) ) ;
#13221 = DIRECTION ( 'NONE',  ( -1.000000000000000000, 0.000000000000000000, 0.000000000000000000 ) ) ;
#13222 = CARTESIAN_POINT ( 'NONE',  ( 10.00000000000000000, 75.11764819372142199, 2.946379043147685728 ) ) ;
#13223 = EDGE_LOOP ( 'NONE', ( #30013, #9481, #20485, #13172 ) ) ;
#13224 = DIRECTION ( 'NONE',  ( -1.000000000000000000, -0.000000000000000000, -0.000000000000000000 ) ) ;
#13225 = EDGE_LOOP ( 'NONE', ( #32790, #29420, #40296, #40662 ) ) ;
#13226 = DIRECTION ( 'NONE',  ( -0.000000000000000000, 0.9135454576426060846, 0.4067366430757888285 ) ) ;
#13227 = CARTESIAN_POINT ( 'NONE',  ( 5.999999999999999112, 27.74655509720669500, 77.16300072079670258 ) ) ;
#13228 = CARTESIAN_POINT ( 'NONE',  ( 0.000000000000000000, -21.32104025579091910, -30.84782396557241313 ) ) ;
#13229 = ORIENTED_EDGE ( 'NONE', *, *, #10111, .T. ) ;
#13230 = AXIS2_PLACEMENT_3D ( 'NONE', #11472, #26394, #38128 ) ;
#13231 = VERTEX_POINT ( 'NONE', #1753 ) ;
#13232 = CARTESIAN_POINT ( 'NONE',  ( 0.000000000000000000, 74.65374052328648702, 8.840884882375350529 ) ) ;
#13233 = CARTESIAN_POINT ( 'NONE',  ( 12.00000000000000000, -25.60904388321925040, -6.976881207771167048 ) ) ;
#13234 = ORIENTED_EDGE ( 'NONE', *, *, #14464, .T. ) ;
#13235 = CARTESIAN_POINT ( 'NONE',  ( -15.44521549751111422, -137.7748507232956001, 5.500000000000000000 ) ) ;
#13236 = DIRECTION ( 'NONE',  ( -0.000000000000000000, -0.000000000000000000, -1.000000000000000000 ) ) ;
#13237 = CARTESIAN_POINT ( 'NONE',  ( 10.00000000000000000, -35.95386929396248377, -10.96151621346525751 ) ) ;
#13238 = AXIS2_PLACEMENT_3D ( 'NONE', #37770, #37527, #18679 ) ;
#13239 = DIRECTION ( 'NONE',  ( 0.000000000000000000, 0.000000000000000000, 1.000000000000000000 ) ) ;
#13240 = CYLINDRICAL_SURFACE ( 'NONE', #20852, 77.49899999999999523 ) ;
#13241 = ADVANCED_FACE ( 'NONE', ( #1279 ), #46300, .T. ) ;
#13242 = DIRECTION ( 'NONE',  ( 0.000000000000000000, 0.000000000000000000, 1.000000000000000000 ) ) ;
#13243 = LINE ( 'NONE', #39188, #31790 ) ;
#13244 = CARTESIAN_POINT ( 'NONE',  ( 10.00000000000000000, -59.03961581697367933, -46.53671651294010303 ) ) ;
#13245 = CARTESIAN_POINT ( 'NONE',  ( 11.99999999999999822, -18.89407956138310496, 75.16055320797023853 ) ) ;
#13246 = CARTESIAN_POINT ( 'NONE',  ( -26.53422223201112828, -120.6595836127786043, 2.500000000000000000 ) ) ;
#13247 = ADVANCED_FACE ( 'NONE', ( #25876 ), #426, .T. ) ;
#13248 = FACE_OUTER_BOUND ( 'NONE', #43916, .T. ) ;
#13249 = CARTESIAN_POINT ( 'NONE',  ( 0.000000000000000000, -36.73666225445845157, -65.58780272294114866 ) ) ;
#13250 = VERTEX_POINT ( 'NONE', #3113 ) ;
#13251 = STYLED_ITEM ( 'NONE', ( #47905 ), #26873 ) ;
#13252 = EDGE_LOOP ( 'NONE', ( #35840, #8599, #14909, #36886 ) ) ;
#13253 = CARTESIAN_POINT ( 'NONE',  ( 12.00000000000000000, 23.59884966291538433, 12.14883922797231186 ) ) ;
#13254 = DIRECTION ( 'NONE',  ( -1.000000000000000000, -0.000000000000000000, -0.000000000000000000 ) ) ;
#13255 = ITEM_DEFINED_TRANSFORMATION ( 'NONE', 'NONE', #17083,  #11636 ) ;
#13256 = CARTESIAN_POINT ( 'NONE',  ( 0.000000000000000000, -41.76937507738745836, -62.50329211542482710 ) ) ;
#13257 = EDGE_LOOP ( 'NONE', ( #26573, #18526, #22155, #31131 ) ) ;
#13258 = EDGE_LOOP ( 'NONE', ( #27782, #22358, #22819, #8781 ) ) ;
#13259 = CIRCLE ( 'NONE', #19487, 12.49999999999999822 ) ;
#13260 = VECTOR ( 'NONE', #16822, 1000.000000000000000 ) ;
#13261 = EDGE_CURVE ( 'NONE', #33075, #27936, #15909, .T. ) ;
#13262 = CARTESIAN_POINT ( 'NONE',  ( 10.00000000000000000, 0.000000000000000000, 0.000000000000000000 ) ) ;
#13263 = VERTEX_POINT ( 'NONE', #15372 ) ;
#13264 = CARTESIAN_POINT ( 'NONE',  ( 11.99999999999999822, -68.27212725128298132, 31.46837873494953541 ) ) ;
#13265 = AXIS2_PLACEMENT_3D ( 'NONE', #45170, #41738, #33892 ) ;
#13266 = VERTEX_POINT ( 'NONE', #29325 ) ;
#13268 = ADVANCED_FACE ( 'NONE', ( #44252 ), #21731, .F. ) ;
#13267 = DIRECTION ( 'NONE',  ( 0.000000000000000000, 1.000000000000000000, 3.469446951953616555E-15 ) ) ;
#13269 = CARTESIAN_POINT ( 'NONE',  ( 0.000000000000000000, 60.67117009219135326, 55.16347631943062169 ) ) ;
#13270 = VECTOR ( 'NONE', #19633, 1000.000000000000000 ) ;
#13271 = EDGE_CURVE ( 'NONE', #17893, #12095, #22158, .T. ) ;
#13272 = CARTESIAN_POINT ( 'NONE',  ( -3.759344165985237129, 0.000000000000000000, -19.05560546998412974 ) ) ;
#13273 = VERTEX_POINT ( 'NONE', #44486 ) ;
#13275 = ORIENTED_EDGE ( 'NONE', *, *, #47665, .F. ) ;
#13274 = DIRECTION ( 'NONE',  ( -0.000000000000000000, -0.000000000000000000, -1.000000000000000000 ) ) ;
#13276 = ORIENTED_EDGE ( 'NONE', *, *, #1446, .F. ) ;
#13277 = ADVANCED_FACE ( 'NONE', ( #11203 ), #33704, .T. ) ;
#13278 = FACE_BOUND ( 'NONE', #20861, .T. ) ;
#13279 = CARTESIAN_POINT ( 'NONE',  ( 21.85433023846371370, -135.0628101570779620, 5.500000000000000000 ) ) ;
#13280 = DIRECTION ( 'NONE',  ( -1.000000000000000000, 0.000000000000000000, 0.000000000000000000 ) ) ;
#13281 = CARTESIAN_POINT ( 'NONE',  ( 0.000000000000000000, 34.94270380257741948, -74.18225833017852722 ) ) ;
#13282 = DIRECTION ( 'NONE',  ( 0.000000000000000000, 0.000000000000000000, 1.000000000000000000 ) ) ;
#13283 = ORIENTED_EDGE ( 'NONE', *, *, #43883, .F. ) ;
#13284 = CARTESIAN_POINT ( 'NONE',  ( 12.00000000000000000, 22.07842321921492612, 8.187992925817123790 ) ) ;
#13285 = VERTEX_POINT ( 'NONE', #15123 ) ;
#13286 = ORIENTED_EDGE ( 'NONE', *, *, #7045, .F. ) ;
#13287 = CARTESIAN_POINT ( 'NONE',  ( 0.000000000000000000, 0.000000000000000000, 0.000000000000000000 ) ) ;
#13288 = ORIENTED_EDGE ( 'NONE', *, *, #15138, .F. ) ;
#13289 = CARTESIAN_POINT ( 'NONE',  ( 10.00000000000000000, 0.000000000000000000, 0.000000000000000000 ) ) ;
#13290 = LINE ( 'NONE', #38268, #13309 ) ;
#13291 = DIRECTION ( 'NONE',  ( 0.000000000000000000, 0.000000000000000000, -1.000000000000000000 ) ) ;
#13292 = ORIENTED_EDGE ( 'NONE', *, *, #15260, .T. ) ;
#13293 = DIRECTION ( 'NONE',  ( -1.000000000000000000, -0.000000000000000000, 0.000000000000000000 ) ) ;
#13294 = DIRECTION ( 'NONE',  ( 0.000000000000000000, 0.000000000000000000, 1.000000000000000000 ) ) ;
#13295 = EDGE_CURVE ( 'NONE', #1706, #22671, #22469, .T. ) ;
#13296 = CARTESIAN_POINT ( 'NONE',  ( -3.000000000000000000, 0.000000000000000000, 0.000000000000000000 ) ) ;
#13297 = FACE_OUTER_BOUND ( 'NONE', #33300, .T. ) ;
#13299 = AXIS2_PLACEMENT_3D ( 'NONE', #10036, #39907, #21283 ) ;
#13298 = CYLINDRICAL_SURFACE ( 'NONE', #31777, 16.00000000000000000 ) ;
#13300 = ORIENTED_EDGE ( 'NONE', *, *, #16265, .T. ) ;
#13301 = VECTOR ( 'NONE', #8672, 1000.000000000000000 ) ;
#13302 = CARTESIAN_POINT ( 'NONE',  ( 10.00000000000000000, -33.79645857604501913, -16.45098606841161626 ) ) ;
#13303 = CARTESIAN_POINT ( 'NONE',  ( 11.99999999999999822, 71.21200624218795383, 40.65526001592638039 ) ) ;
#13304 = CARTESIAN_POINT ( 'NONE',  ( 11.99999999999999822, 46.54456581323805153, 59.03342792756280488 ) ) ;
#13305 = DIRECTION ( 'NONE',  ( -1.000000000000000000, 0.000000000000000000, 0.000000000000000000 ) ) ;
#13306 = CIRCLE ( 'NONE', #29708, 15.99999999999999467 ) ;
#13307 = CARTESIAN_POINT ( 'NONE',  ( 10.00000000000000000, 65.58780272294076497, 36.73666225445916211 ) ) ;
#13308 = DIRECTION ( 'NONE',  ( -1.000000000000000000, 0.000000000000000000, -0.000000000000000000 ) ) ;
#13309 = VECTOR ( 'NONE', #23570, 1000.000000000000000 ) ;
#13310 = CARTESIAN_POINT ( 'NONE',  ( -11.99999999999999645, 0.000000000000000000, 0.000000000000000000 ) ) ;
#13311 = AXIS2_PLACEMENT_3D ( 'NONE', #11304, #10314, #14728 ) ;
#13312 = ORIENTED_EDGE ( 'NONE', *, *, #39246, .F. ) ;
#13313 = FACE_OUTER_BOUND ( 'NONE', #13257, .T. ) ;
#13314 = ADVANCED_FACE ( 'NONE', ( #24754 ), #41310, .T. ) ;
#13315 = DIRECTION ( 'NONE',  ( 0.000000000000000000, 0.000000000000000000, 1.000000000000000000 ) ) ;
#13316 = ORIENTED_EDGE ( 'NONE', *, *, #23833, .F. ) ;
#13317 = DIRECTION ( 'NONE',  ( 0.000000000000000000, 0.000000000000000000, 1.000000000000000000 ) ) ;
#13318 = ORIENTED_EDGE ( 'NONE', *, *, #6102, .T. ) ;
#13319 = EDGE_CURVE ( 'NONE', #19209, #36599, #29797, .T. ) ;
#13320 = ORIENTED_EDGE ( 'NONE', *, *, #5732, .F. ) ;
#13321 = EDGE_CURVE ( 'NONE', #16029, #2989, #46422, .T. ) ;
#13322 = EDGE_CURVE ( 'NONE', #42528, #14101, #171, .T. ) ;
#13323 = VECTOR ( 'NONE', #18728, 1000.000000000000000 ) ;
#13324 = ORIENTED_EDGE ( 'NONE', *, *, #28393, .T. ) ;
#13325 = LINE ( 'NONE', #24102, #23716 ) ;
#13326 = CIRCLE ( 'NONE', #40680, 82.00000000000000000 ) ;
#13327 = EDGE_CURVE ( 'NONE', #37807, #4251, #44841, .T. ) ;
#13328 = CARTESIAN_POINT ( 'NONE',  ( 11.99999999999999822, -75.11725578898470701, 2.956366410620372864 ) ) ;
#13329 = DIRECTION ( 'NONE',  ( 0.000000000000000000, 0.000000000000000000, 1.000000000000000000 ) ) ;
#13330 = VECTOR ( 'NONE', #34749, 1000.000000000000000 ) ;
#13331 = ORIENTED_EDGE ( 'NONE', *, *, #32293, .T. ) ;
#13332 = LINE ( 'NONE', #9642, #3170 ) ;
#13333 = EDGE_CURVE ( 'NONE', #33441, #38765, #1052, .T. ) ;
#13334 = EDGE_LOOP ( 'NONE', ( #10685, #48073, #31465, #36842 ) ) ;
#13335 = ORIENTED_EDGE ( 'NONE', *, *, #8363, .T. ) ;
#13336 = CARTESIAN_POINT ( 'NONE',  ( -7.572224309238338336, -145.4393675041377492, 5.500000000000000000 ) ) ;
#13337 = DIRECTION ( 'NONE',  ( -1.000000000000000000, 0.000000000000000000, 0.000000000000000000 ) ) ;
#13338 = AXIS2_PLACEMENT_3D ( 'NONE', #1315, #39235, #46100 ) ;
#13339 = DIRECTION ( 'NONE',  ( -1.000000000000000000, 0.000000000000000000, 0.000000000000000000 ) ) ;
#13340 = ORIENTED_EDGE ( 'NONE', *, *, #15283, .F. ) ;
#13341 = VERTEX_POINT ( 'NONE', #3359 ) ;
#13342 = ORIENTED_EDGE ( 'NONE', *, *, #18720, .F. ) ;
#13343 = AXIS2_PLACEMENT_3D ( 'NONE', #1484, #16411, #38940 ) ;
#13344 = DIRECTION ( 'NONE',  ( -1.000000000000000000, -0.000000000000000000, 0.000000000000000000 ) ) ;
#13345 = ORIENTED_EDGE ( 'NONE', *, *, #46356, .F. ) ;
#13346 = DIRECTION ( 'NONE',  ( 0.000000000000000000, 0.000000000000000000, 1.000000000000000000 ) ) ;
#13347 = LINE ( 'NONE', #2551, #21463 ) ;
#13348 = DIRECTION ( 'NONE',  ( 0.000000000000000000, 0.000000000000000000, 1.000000000000000000 ) ) ;
#13349 = CARTESIAN_POINT ( 'NONE',  ( 5.000000000000000000, -50.23322058963298531, -64.81221759200398935 ) ) ;
#13350 = CARTESIAN_POINT ( 'NONE',  ( 0.000000000000000000, 76.41127070299290835, -12.93880638057231991 ) ) ;
#13351 = CARTESIAN_POINT ( 'NONE',  ( -42.50000000000000000, 0.000000000000000000, -15.77977592589476608 ) ) ;
#13352 = FACE_OUTER_BOUND ( 'NONE', #10004, .T. ) ;
#13353 = LINE ( 'NONE', #39788, #9771 ) ;
#13354 = CARTESIAN_POINT ( 'NONE',  ( 6.000000000000000000, -34.94270380257585629, -74.18225833017926618 ) ) ;
#13355 = CARTESIAN_POINT ( 'NONE',  ( 10.00000000000000000, -55.20638768913724448, -51.02545421589383068 ) ) ;
#13356 = EDGE_LOOP ( 'NONE', ( #44325, #11443, #26694, #16184 ) ) ;
#13357 = DIRECTION ( 'NONE',  ( -1.000000000000000000, 0.000000000000000000, 0.000000000000000000 ) ) ;
#13358 = CARTESIAN_POINT ( 'NONE',  ( 10.00000000000000000, 0.000000000000000000, 0.000000000000000000 ) ) ;
#13359 = CARTESIAN_POINT ( 'NONE',  ( 10.00000000000000000, 36.88895765772633695, 6.736453364083687667 ) ) ;
#13360 = LINE ( 'NONE', #46414, #33459 ) ;
#13361 = AXIS2_PLACEMENT_3D ( 'NONE', #35319, #12106, #27030 ) ;
#13362 = ADVANCED_FACE ( 'NONE', ( #4102 ), #19015, .T. ) ;
#13363 = DIRECTION ( 'NONE',  ( 0.000000000000000000, 0.000000000000000000, 1.000000000000000000 ) ) ;
#13364 = DIRECTION ( 'NONE',  ( 0.000000000000000000, 0.000000000000000000, 1.000000000000000000 ) ) ;
#13365 = VECTOR ( 'NONE', #13390, 1000.000000000000000 ) ;
#13366 = ORIENTED_EDGE ( 'NONE', *, *, #27370, .T. ) ;
#13367 = LINE ( 'NONE', #47132, #34780 ) ;
#13368 = VECTOR ( 'NONE', #34333, 1000.000000000000000 ) ;
#13369 = CIRCLE ( 'NONE', #38381, 31.99999999999998224 ) ;
#13370 = EDGE_CURVE ( 'NONE', #42780, #40355, #8073, .T. ) ;
#13371 = ORIENTED_EDGE ( 'NONE', *, *, #17030, .F. ) ;
#13372 = EDGE_CURVE ( 'NONE', #1493, #45724, #23727, .T. ) ;
#13373 = LINE ( 'NONE', #20957, #8782 ) ;
#13374 = VECTOR ( 'NONE', #202, 1000.000000000000000 ) ;
#13375 = ORIENTED_EDGE ( 'NONE', *, *, #31092, .T. ) ;
#13376 = CIRCLE ( 'NONE', #3221, 31.99999999999998579 ) ;
#13377 = ORIENTED_EDGE ( 'NONE', *, *, #20654, .T. ) ;
#13378 = CARTESIAN_POINT ( 'NONE',  ( 5.000000000000002665, 3.894527615417891830, 81.90746397400390322 ) ) ;
#13379 = VERTEX_POINT ( 'NONE', #33235 ) ;
#13380 = ADVANCED_FACE ( 'NONE', ( #29560 ), #10959, .T. ) ;
#13381 = EDGE_CURVE ( 'NONE', #10994, #5603, #2613, .T. ) ;
#13382 = ORIENTED_EDGE ( 'NONE', *, *, #5024, .T. ) ;
#13383 = DIRECTION ( 'NONE',  ( 0.000000000000000000, 0.000000000000000000, 1.000000000000000000 ) ) ;
#13384 = FACE_OUTER_BOUND ( 'NONE', #31814, .T. ) ;
#13385 = ORIENTED_EDGE ( 'NONE', *, *, #46869, .F. ) ;
#13386 = ORIENTED_EDGE ( 'NONE', *, *, #44607, .F. ) ;
#13387 = ORIENTED_EDGE ( 'NONE', *, *, #5566, .F. ) ;
#13388 = DIRECTION ( 'NONE',  ( -1.000000000000000000, -0.000000000000000000, -0.000000000000000000 ) ) ;
#13389 = EDGE_CURVE ( 'NONE', #28753, #22152, #15836, .T. ) ;
#13391 = VERTEX_POINT ( 'NONE', #19724 ) ;
#13390 = DIRECTION ( 'NONE',  ( -1.000000000000000000, -0.000000000000000000, -0.000000000000000000 ) ) ;
#13392 = CIRCLE ( 'NONE', #2444, 16.00000000000000355 ) ;
#13393 = DIRECTION ( 'NONE',  ( 0.000000000000000000, -0.8090169943749531134, 0.5877852522924653655 ) ) ;
#13395 = VERTEX_POINT ( 'NONE', #1399 ) ;
#13394 = CIRCLE ( 'NONE', #26676, 16.00000000000000000 ) ;
#13396 = VERTEX_POINT ( 'NONE', #8486 ) ;
#13397 = CARTESIAN_POINT ( 'NONE',  ( 0.000000000000000000, 75.11764819372149304, -2.946379043146603482 ) ) ;
#13398 = VERTEX_POINT ( 'NONE', #19260 ) ;
#13399 = LINE ( 'NONE', #18191, #44500 ) ;
#13400 = ORIENTED_EDGE ( 'NONE', *, *, #9337, .T. ) ;
#13401 = VECTOR ( 'NONE', #448, 1000.000000000000000 ) ;
#13402 = DIRECTION ( 'NONE',  ( -1.000000000000000000, -0.000000000000000000, 0.000000000000000000 ) ) ;
#13403 = DIRECTION ( 'NONE',  ( 0.000000000000000000, 0.8526401643540936215, -0.5224985647159469115 ) ) ;
#13404 = FACE_OUTER_BOUND ( 'NONE', #39279, .T. ) ;
#13405 = CYLINDRICAL_SURFACE ( 'NONE', #40887, 77.49899999999999523 ) ;
#13406 = ORIENTED_EDGE ( 'NONE', *, *, #2168, .F. ) ;
#13407 = FACE_OUTER_BOUND ( 'NONE', #18940, .T. ) ;
#13408 = DIRECTION ( 'NONE',  ( 0.000000000000000000, 0.000000000000000000, 1.000000000000000000 ) ) ;
#13409 = ORIENTED_EDGE ( 'NONE', *, *, #11887, .T. ) ;
#13410 = CIRCLE ( 'NONE', #12541, 82.00000000000000000 ) ;
#13411 = CARTESIAN_POINT ( 'NONE',  ( 11.99999999999999822, 39.78640506895604290, 66.50666863322015843 ) ) ;
#13412 = VERTEX_POINT ( 'NONE', #663 ) ;
#13413 = CIRCLE ( 'NONE', #19642, 77.49900000000000944 ) ;
#13414 = DIRECTION ( 'NONE',  ( 0.000000000000000000, 0.2334453638559060296, -0.9723699203976764460 ) ) ;
#13415 = DIRECTION ( 'NONE',  ( -1.000000000000000000, 0.000000000000000000, 0.000000000000000000 ) ) ;
#13416 = DIRECTION ( 'NONE',  ( 0.000000000000000000, -0.9723699203976740035, -0.2334453638559160216 ) ) ;
#13417 = CARTESIAN_POINT ( 'NONE',  ( -10.00000000000000000, 0.000000000000000000, 0.000000000000000000 ) ) ;
#13418 = DIRECTION ( 'NONE',  ( -1.000000000000000000, -0.000000000000000000, 0.000000000000000000 ) ) ;
#13419 = DIRECTION ( 'NONE',  ( 0.000000000000000000, -0.3826834323650772363, -0.9238795325112919565 ) ) ;
#13420 = EDGE_LOOP ( 'NONE', ( #40786, #3390, #34381, #31026 ) ) ;
#13421 = EDGE_CURVE ( 'NONE', #45038, #41084, #29183, .T. ) ;
#13422 = DIRECTION ( 'NONE',  ( 0.000000000000000000, -0.3090169943749349057, -0.9510565162951577500 ) ) ;
#13423 = LINE ( 'NONE', #43531, #45614 ) ;
#13424 = DIRECTION ( 'NONE',  ( -1.000000000000000000, 0.000000000000000000, 0.000000000000000000 ) ) ;
#13425 = ORIENTED_EDGE ( 'NONE', *, *, #47465, .T. ) ;
#13426 = EDGE_CURVE ( 'NONE', #7999, #31795, #19985, .T. ) ;
#13427 = CARTESIAN_POINT ( 'NONE',  ( 10.00000000000000000, 76.41127070299273782, 12.93880638057342836 ) ) ;
#13428 = EDGE_CURVE ( 'NONE', #45301, #4301, #16325, .T. ) ;
#13429 = ORIENTED_EDGE ( 'NONE', *, *, #44968, .T. ) ;
#13430 = VERTEX_POINT ( 'NONE', #30525 ) ;
#13431 = ORIENTED_EDGE ( 'NONE', *, *, #7578, .T. ) ;
#13432 = CIRCLE ( 'NONE', #23587, 1.000000000000000000 ) ;
#13433 = VECTOR ( 'NONE', #27013, 1000.000000000000000 ) ;
#13434 = VECTOR ( 'NONE', #8868, 1000.000000000000114 ) ;
#13435 = CARTESIAN_POINT ( 'NONE',  ( 10.00000000000000000, 74.18225833017937987, -34.94270380257560049 ) ) ;
#13436 = VECTOR ( 'NONE', #1803, 1000.000000000000000 ) ;
#13437 = DIRECTION ( 'NONE',  ( -1.000000000000000000, -0.000000000000000000, -0.000000000000000000 ) ) ;
#13438 = ORIENTED_EDGE ( 'NONE', *, *, #24868, .F. ) ;
#13439 = AXIS2_PLACEMENT_3D ( 'NONE', #47644, #13893, #2157 ) ;
#13440 = ADVANCED_FACE ( 'NONE', ( #34416 ), #30773, .T. ) ;
#13441 = EDGE_CURVE ( 'NONE', #23235, #31274, #38602, .T. ) ;
#13442 = EDGE_LOOP ( 'NONE', ( #14366, #15558, #22499, #47027 ) ) ;
#13443 = EDGE_CURVE ( 'NONE', #22912, #21369, #37874, .T. ) ;
#13444 = DIRECTION ( 'NONE',  ( -0.8225049752423791993, -0.5687579148473745905, 0.000000000000000000 ) ) ;
#13445 = CIRCLE ( 'NONE', #32219, 77.49899999999999523 ) ;
#13446 = ORIENTED_EDGE ( 'NONE', *, *, #47671, .T. ) ;
#13447 = ORIENTED_EDGE ( 'NONE', *, *, #30051, .T. ) ;
#13448 = ORIENTED_EDGE ( 'NONE', *, *, #40954, .T. ) ;
#13449 = VERTEX_POINT ( 'NONE', #16096 ) ;
#13450 = EDGE_CURVE ( 'NONE', #39014, #39398, #27566, .T. ) ;
#13451 = CARTESIAN_POINT ( 'NONE',  ( 0.000000000000000000, 0.000000000000000000, 0.000000000000000000 ) ) ;
#13452 = EDGE_LOOP ( 'NONE', ( #44938, #37913, #22032, #22377 ) ) ;
#13453 = DIRECTION ( 'NONE',  ( 0.000000000000000000, 0.000000000000000000, -1.000000000000000000 ) ) ;
#13454 = ORIENTED_EDGE ( 'NONE', *, *, #12819, .F. ) ;
#13455 = DIRECTION ( 'NONE',  ( -0.9966891607226786576, -0.08130631524009861166, 0.000000000000000000 ) ) ;
#13456 = DIRECTION ( 'NONE',  ( -1.000000000000000000, -0.000000000000000000, 0.000000000000000000 ) ) ;
#13457 = DIRECTION ( 'NONE',  ( 0.000000000000000000, -0.5877852522924624790, -0.8090169943749552228 ) ) ;
#13458 = ORIENTED_EDGE ( 'NONE', *, *, #30304, .T. ) ;
#13459 = FACE_OUTER_BOUND ( 'NONE', #26469, .T. ) ;
#13460 = VERTEX_POINT ( 'NONE', #45950 ) ;
#13461 = DIRECTION ( 'NONE',  ( 0.000000000000000000, -0.9876883405951358830, -0.1564344650402420822 ) ) ;
#13462 = DIRECTION ( 'NONE',  ( 0.000000000000000000, 0.000000000000000000, 1.000000000000000000 ) ) ;
#13463 = VERTEX_POINT ( 'NONE', #26856 ) ;
#13464 = ORIENTED_EDGE ( 'NONE', *, *, #44499, .F. ) ;
#13465 = CARTESIAN_POINT ( 'NONE',  ( -12.00000000000000000, 0.000000000000000000, 0.000000000000000000 ) ) ;
#13466 = CARTESIAN_POINT ( 'NONE',  ( 0.000000000000000000, 40.65526001592612459, 71.21200624218811015 ) ) ;
#13467 = VERTEX_POINT ( 'NONE', #34919 ) ;
#13468 = DIRECTION ( 'NONE',  ( -1.000000000000000000, -0.000000000000000000, -0.000000000000000000 ) ) ;
#13469 = CYLINDRICAL_SURFACE ( 'NONE', #6348, 16.00000000000000000 ) ;
#13470 = DIRECTION ( 'NONE',  ( -1.000000000000000000, -0.000000000000000000, 0.000000000000000000 ) ) ;
#13471 = CARTESIAN_POINT ( 'NONE',  ( 10.00000000000000000, 0.000000000000000000, 0.000000000000000000 ) ) ;
#13472 = VECTOR ( 'NONE', #10882, 1000.000000000000000 ) ;
#13473 = LINE ( 'NONE', #47007, #4436 ) ;
#13474 = CARTESIAN_POINT ( 'NONE',  ( 0.000000000000000000, 0.000000000000000000, 0.000000000000000000 ) ) ;
#13475 = CARTESIAN_POINT ( 'NONE',  ( 0.000000000000000000, 79.10210256391398786, -21.60688246758503084 ) ) ;
#13476 = AXIS2_PLACEMENT_3D ( 'NONE', #9690, #13611, #28547 ) ;
#13477 = EDGE_CURVE ( 'NONE', #41663, #47844, #6453, .T. ) ;
#13478 = DIRECTION ( 'NONE',  ( -1.000000000000000000, 0.000000000000000000, -0.000000000000000000 ) ) ;
#13479 = CARTESIAN_POINT ( 'NONE',  ( 11.99999999999999822, 0.000000000000000000, 0.000000000000000000 ) ) ;
#13480 = EDGE_CURVE ( 'NONE', #17719, #26953, #41794, .T. ) ;
#13481 = DIRECTION ( 'NONE',  ( 0.1850432970638656860, -0.9827303690289285187, 0.000000000000000000 ) ) ;
#13482 = CARTESIAN_POINT ( 'NONE',  ( 15.00000000000000000, -25.60904388321925040, -6.976881207771165272 ) ) ;
#13483 = EDGE_CURVE ( 'NONE', #32098, #46617, #31263, .T. ) ;
#13484 = EDGE_LOOP ( 'NONE', ( #43557, #44261, #35568, #27656 ) ) ;
#13485 = VERTEX_POINT ( 'NONE', #20228 ) ;
#13486 = DIRECTION ( 'NONE',  ( 0.000000000000000000, 0.000000000000000000, -1.000000000000000000 ) ) ;
#13487 = EDGE_CURVE ( 'NONE', #28808, #15783, #24408, .T. ) ;
#13488 = DIRECTION ( 'NONE',  ( 0.000000000000000000, -0.1045284632676429099, -0.9945218953682744001 ) ) ;
#13489 = VECTOR ( 'NONE', #38154, 1000.000000000000000 ) ;
#13490 = CARTESIAN_POINT ( 'NONE',  ( 11.99999999999999822, 0.8261519478441983200, -77.49459641780885022 ) ) ;
#13491 = ORIENTED_EDGE ( 'NONE', *, *, #30247, .F. ) ;
#13492 = ADVANCED_FACE ( 'NONE', ( #23181 ), #7996, .T. ) ;
#13493 = AXIS2_PLACEMENT_3D ( 'NONE', #5475, #42691, #4750 ) ;
#13494 = EDGE_LOOP ( 'NONE', ( #36611, #2282, #29401, #28543 ) ) ;
#13495 = CIRCLE ( 'NONE', #40851, 37.49900000000000944 ) ;
#13496 = EDGE_CURVE ( 'NONE', #21020, #28981, #12185, .T. ) ;
#13497 = DIRECTION ( 'NONE',  ( -1.000000000000000000, -0.000000000000000000, 0.000000000000000000 ) ) ;
#13498 = AXIS2_PLACEMENT_3D ( 'NONE', #42299, #8755, #27139 ) ;
#13499 = DIRECTION ( 'NONE',  ( 0.000000000000000000, 0.000000000000000000, 1.000000000000000000 ) ) ;
#13500 = CIRCLE ( 'NONE', #45569, 16.00000000000000000 ) ;
#13501 = ORIENTED_EDGE ( 'NONE', *, *, #16150, .T. ) ;
#13502 = DIRECTION ( 'NONE',  ( 1.000000000000000000, -0.000000000000000000, -0.000000000000000000 ) ) ;
#13503 = AXIS2_PLACEMENT_3D ( 'NONE', #42922, #20384, #8893 ) ;
#13504 = EDGE_CURVE ( 'NONE', #20013, #45931, #43177, .T. ) ;
#13505 = CARTESIAN_POINT ( 'NONE',  ( 10.00000000000000000, 0.000000000000000000, 0.000000000000000000 ) ) ;
#13506 = AXIS2_PLACEMENT_3D ( 'NONE', #36813, #11123, #22386 ) ;
#13507 = CARTESIAN_POINT ( 'NONE',  ( 0.000000000000000000, 0.000000000000000000, 0.000000000000000000 ) ) ;
#13508 = ORIENTED_EDGE ( 'NONE', *, *, #27099, .T. ) ;
#13509 = DIRECTION ( 'NONE',  ( -1.000000000000000000, -0.000000000000000000, -0.000000000000000000 ) ) ;
#13510 = VECTOR ( 'NONE', #5258, 1000.000000000000000 ) ;
#13511 = VERTEX_POINT ( 'NONE', #42760 ) ;
#13512 = CARTESIAN_POINT ( 'NONE',  ( 0.000000000000000000, 0.000000000000000000, 0.000000000000000000 ) ) ;
#13513 = DIRECTION ( 'NONE',  ( 0.000000000000000000, 0.000000000000000000, 1.000000000000000000 ) ) ;
#13514 = CARTESIAN_POINT ( 'NONE',  ( 15.00000000000000000, 16.83928648764922542, -16.46020748918050458 ) ) ;
#13515 = EDGE_CURVE ( 'NONE', #46188, #41093, #29117, .T. ) ;
#13516 = CARTESIAN_POINT ( 'NONE',  ( 10.00000000000000000, -35.91791733033525702, 68.67312586194982771 ) ) ;
#13517 = DIRECTION ( 'NONE',  ( -1.000000000000000000, 0.000000000000000000, -0.000000000000000000 ) ) ;
#13518 = ORIENTED_EDGE ( 'NONE', *, *, #3518, .F. ) ;
#13519 = PLANE ( 'NONE',  #8398 ) ;
#13520 = ORIENTED_EDGE ( 'NONE', *, *, #24569, .F. ) ;
#13521 = ORIENTED_EDGE ( 'NONE', *, *, #38484, .F. ) ;
#13522 = DIRECTION ( 'NONE',  ( 0.000000000000000000, 0.3826834323650905589, -0.9238795325112864054 ) ) ;
#13523 = DIRECTION ( 'NONE',  ( -1.000000000000000000, 0.000000000000000000, -0.000000000000000000 ) ) ;
#13524 = CARTESIAN_POINT ( 'NONE',  ( 10.00000000000000000, -37.58145647212455032, 0.6853352020789044152 ) ) ;
#13525 = CARTESIAN_POINT ( 'NONE',  ( 0.000000000000000000, -72.35432306680469594, -20.40083707022958848 ) ) ;
#13526 = ORIENTED_EDGE ( 'NONE', *, *, #13878, .F. ) ;
#13527 = CYLINDRICAL_SURFACE ( 'NONE', #23000, 31.99999999999998579 ) ;
#13528 = VECTOR ( 'NONE', #13803, 1000.000000000000000 ) ;
#13529 = CARTESIAN_POINT ( 'NONE',  ( 11.99999999999999822, -68.67312586194971402, -35.91791733033549860 ) ) ;
#13530 = DIRECTION ( 'NONE',  ( -1.000000000000000000, -0.000000000000000000, -0.000000000000000000 ) ) ;
#13531 = DIRECTION ( 'NONE',  ( 0.000000000000000000, 0.000000000000000000, 1.000000000000000000 ) ) ;
#13532 = ADVANCED_FACE ( 'NONE', ( #6271 ), #6040, .T. ) ;
#13533 = CARTESIAN_POINT ( 'NONE',  ( 5.000000000000002665, -3.894527615417340272, -81.90746397400393164 ) ) ;
#13534 = DIRECTION ( 'NONE',  ( -1.000000000000000000, 0.000000000000000000, -0.000000000000000000 ) ) ;
#13535 = LINE ( 'NONE', #17916, #8249 ) ;
#13536 = DIRECTION ( 'NONE',  ( -1.000000000000000000, -0.000000000000000000, -0.000000000000000000 ) ) ;
#13537 = CYLINDRICAL_SURFACE ( 'NONE', #6748, 16.00000000000000000 ) ;
#13538 = ADVANCED_FACE ( 'NONE', ( #2342 ), #13862, .T. ) ;
#13539 = CIRCLE ( 'NONE', #22929, 42.00000000000000000 ) ;
#13540 = CIRCLE ( 'NONE', #36200, 31.99999999999999289 ) ;
#13541 = PLANE ( 'NONE',  #18158 ) ;
#13542 = DIRECTION ( 'NONE',  ( -1.000000000000000000, -0.000000000000000000, -0.000000000000000000 ) ) ;
#13543 = AXIS2_PLACEMENT_3D ( 'NONE', #19525, #20511, #38161 ) ;
#13544 = EDGE_CURVE ( 'NONE', #10193, #39901, #13373, .T. ) ;
#13545 = ORIENTED_EDGE ( 'NONE', *, *, #12385, .T. ) ;
#13546 = ORIENTED_EDGE ( 'NONE', *, *, #4426, .F. ) ;
#13547 = LINE ( 'NONE', #24087, #20652 ) ;
#13548 = AXIS2_PLACEMENT_3D ( 'NONE', #16007, #34577, #34111 ) ;
#13549 = ORIENTED_EDGE ( 'NONE', *, *, #14026, .T. ) ;
#13550 = EDGE_CURVE ( 'NONE', #1729, #47158, #16621, .T. ) ;
#13551 = DIRECTION ( 'NONE',  ( -1.000000000000000000, -0.000000000000000000, 0.000000000000000000 ) ) ;
#13552 = AXIS2_PLACEMENT_3D ( 'NONE', #6932, #22092, #17932 ) ;
#13553 = DIRECTION ( 'NONE',  ( -0.000000000000000000, -0.000000000000000000, -1.000000000000000000 ) ) ;
#13554 = CIRCLE ( 'NONE', #9666, 77.49899999999999523 ) ;
#13555 = VERTEX_POINT ( 'NONE', #39807 ) ;
#13556 = PLANE ( 'NONE',  #29963 ) ;
#13557 = ORIENTED_EDGE ( 'NONE', *, *, #45166, .T. ) ;
#13558 = AXIS2_PLACEMENT_3D ( 'NONE', #22022, #26438, #11744 ) ;
#13559 = EDGE_LOOP ( 'NONE', ( #10801, #41014, #15036, #45501 ) ) ;
#13560 = CIRCLE ( 'NONE', #26844, 77.49900000000000944 ) ;
#13561 = DIRECTION ( 'NONE',  ( 0.000000000000000000, 0.000000000000000000, -1.000000000000000000 ) ) ;
#13562 = ORIENTED_EDGE ( 'NONE', *, *, #43709, .T. ) ;
#13563 = FACE_OUTER_BOUND ( 'NONE', #33142, .T. ) ;
#13564 = AXIS2_PLACEMENT_3D ( 'NONE', #24610, #47113, #47586 ) ;
#13565 = CIRCLE ( 'NONE', #30807, 31.99999999999999645 ) ;
#13566 = LINE ( 'NONE', #39032, #35558 ) ;
#13567 = ORIENTED_EDGE ( 'NONE', *, *, #36413, .F. ) ;
#13568 = LINE ( 'NONE', #32183, #46971 ) ;
#13569 = CIRCLE ( 'NONE', #9643, 77.49900000000000944 ) ;
#13570 = ORIENTED_EDGE ( 'NONE', *, *, #37346, .F. ) ;
#13571 = CYLINDRICAL_SURFACE ( 'NONE', #48338, 31.99999999999999289 ) ;
#13572 = CARTESIAN_POINT ( 'NONE',  ( 10.00000000000000000, 65.64334221924966073, -41.19522573413664190 ) ) ;
#13573 = FACE_OUTER_BOUND ( 'NONE', #6234, .T. ) ;
#13574 = VERTEX_POINT ( 'NONE', #35878 ) ;
#13575 = VECTOR ( 'NONE', #31397, 1000.000000000000000 ) ;
#13576 = ORIENTED_EDGE ( 'NONE', *, *, #44478, .T. ) ;
#13577 = CARTESIAN_POINT ( 'NONE',  ( -7.469491406282094736, 4.756046723998911929, 52.00000000000002132 ) ) ;
#13578 = ORIENTED_EDGE ( 'NONE', *, *, #10868, .F. ) ;
#13579 = AXIS2_PLACEMENT_3D ( 'NONE', #33570, #45308, #28 ) ;
#13580 = DIRECTION ( 'NONE',  ( 0.000000000000000000, 0.000000000000000000, -1.000000000000000000 ) ) ;
#13581 = CIRCLE ( 'NONE', #38612, 31.99999999999999645 ) ;
#13582 = CARTESIAN_POINT ( 'NONE',  ( 0.000000000000000000, 0.000000000000000000, 125.0000000000000000 ) ) ;
#13583 = CARTESIAN_POINT ( 'NONE',  ( -8.637688417678548447, 13.69818742750669571, -45.00000000000000000 ) ) ;
#13584 = DIRECTION ( 'NONE',  ( 0.000000000000000000, 0.000000000000000000, 1.000000000000000000 ) ) ;
#13585 = DIRECTION ( 'NONE',  ( -0.4279312458752990711, -0.9038112904824846527, 0.000000000000000000 ) ) ;
#13586 = AXIS2_PLACEMENT_3D ( 'NONE', #35050, #5939, #42403 ) ;
#13587 = DIRECTION ( 'NONE',  ( -1.000000000000000000, -0.000000000000000000, -0.000000000000000000 ) ) ;
#13588 = CARTESIAN_POINT ( 'NONE',  ( 10.00000000000000000, 33.00180498840046539, 17.80606268964551120 ) ) ;
#13589 = LINE ( 'NONE', #28528, #43402 ) ;
#13590 = CARTESIAN_POINT ( 'NONE',  ( -5.565113727472255967, 10.17789316117534248, -54.99999999999998579 ) ) ;
#13591 = DIRECTION ( 'NONE',  ( -1.000000000000000000, -0.000000000000000000, 0.000000000000000000 ) ) ;
#13592 = ORIENTED_EDGE ( 'NONE', *, *, #21492, .F. ) ;
#13593 = FACE_OUTER_BOUND ( 'NONE', #48289, .T. ) ;
#13594 = EDGE_CURVE ( 'NONE', #44798, #1534, #32463, .T. ) ;
#13595 = DIRECTION ( 'NONE',  ( -0.000000000000000000, 0.000000000000000000, 1.000000000000000000 ) ) ;
#13596 = DIRECTION ( 'NONE',  ( -1.000000000000000000, 0.000000000000000000, -0.000000000000000000 ) ) ;
#13597 = EDGE_CURVE ( 'NONE', #10091, #14358, #43482, .T. ) ;
#13598 = CARTESIAN_POINT ( 'NONE',  ( -12.00000000000000000, 2.123263276254396040E-15, 17.30399999999999849 ) ) ;
#13599 = CIRCLE ( 'NONE', #15181, 37.49900000000000944 ) ;
#13600 = AXIS2_PLACEMENT_3D ( 'NONE', #29896, #42128, #19358 ) ;
#13601 = CARTESIAN_POINT ( 'NONE',  ( 11.99999999999999822, 81.90746397400387480, 3.894527615418187150 ) ) ;
#13602 = CARTESIAN_POINT ( 'NONE',  ( 7.001685179585692254, -14.98378029539707512, -1.199999999999999956 ) ) ;
#13603 = VERTEX_POINT ( 'NONE', #25097 ) ;
#13604 = EDGE_CURVE ( 'NONE', #8489, #40628, #40830, .T. ) ;
#13605 = VECTOR ( 'NONE', #13293, 1000.000000000000000 ) ;
#13607 = VECTOR ( 'NONE', #45669, 1000.000000000000000 ) ;
#13606 = DIRECTION ( 'NONE',  ( -1.000000000000000000, 0.000000000000000000, 0.000000000000000000 ) ) ;
#13608 = AXIS2_PLACEMENT_3D ( 'NONE', #31754, #28288, #20222 ) ;
#13609 = EDGE_CURVE ( 'NONE', #27706, #24980, #1884, .T. ) ;
#13610 = ORIENTED_EDGE ( 'NONE', *, *, #12187, .T. ) ;
#13611 = DIRECTION ( 'NONE',  ( -1.000000000000000000, 0.000000000000000000, -0.000000000000000000 ) ) ;
#13612 = EDGE_LOOP ( 'NONE', ( #37721, #15785, #13770, #47575 ) ) ;
#13613 = ORIENTED_EDGE ( 'NONE', *, *, #19332, .T. ) ;
#13614 = AXIS2_PLACEMENT_3D ( 'NONE', #32397, #5721, #25030 ) ;
#13615 = ORIENTED_EDGE ( 'NONE', *, *, #18288, .T. ) ;
#13616 = VECTOR ( 'NONE', #18086, 1000.000000000000000 ) ;
#13617 = ORIENTED_EDGE ( 'NONE', *, *, #39649, .T. ) ;
#13618 = AXIS2_PLACEMENT_3D ( 'NONE', #1580, #30308, #4112 ) ;
#13619 = CARTESIAN_POINT ( 'NONE',  ( -3.000000000000000000, -18.13022148937263012, 15.02647892043544608 ) ) ;
#13620 = ORIENTED_EDGE ( 'NONE', *, *, #46906, .T. ) ;
#13621 = AXIS2_PLACEMENT_3D ( 'NONE', #34008, #27166, #45767 ) ;
#13622 = EDGE_LOOP ( 'NONE', ( #26938, #27019, #35181, #26155, #22976, #1943 ) ) ;
#13623 = FACE_OUTER_BOUND ( 'NONE', #14786, .T. ) ;
#13625 = VERTEX_POINT ( 'NONE', #16812 ) ;
#13624 = PLANE ( 'NONE',  #30846 ) ;
#13626 = ORIENTED_EDGE ( 'NONE', *, *, #46637, .F. ) ;
#13627 = EDGE_LOOP ( 'NONE', ( #18260, #8094, #40228, #5398 ) ) ;
#13628 = AXIS2_PLACEMENT_3D ( 'NONE', #18647, #27392, #37496 ) ;
#13629 = ORIENTED_EDGE ( 'NONE', *, *, #16817, .T. ) ;
#13630 = DIRECTION ( 'NONE',  ( 0.000000000000000000, 0.000000000000000000, 1.000000000000000000 ) ) ;
#13632 = VERTEX_POINT ( 'NONE', #21430 ) ;
#13631 = DIRECTION ( 'NONE',  ( -1.000000000000000000, -0.000000000000000000, 0.000000000000000000 ) ) ;
#13634 = CARTESIAN_POINT ( 'NONE',  ( 12.00000000000000000, 8.688484142253932063, -21.88630264137371029 ) ) ;
#13633 = VECTOR ( 'NONE', #1496, 999.9999999999998863 ) ;
#13635 = EDGE_CURVE ( 'NONE', #22127, #43691, #15057, .T. ) ;
#13636 = VERTEX_POINT ( 'NONE', #28294 ) ;
#13637 = ORIENTED_EDGE ( 'NONE', *, *, #25183, .T. ) ;
#13638 = PLANE ( 'NONE',  #26301 ) ;
#13639 = VERTEX_POINT ( 'NONE', #5796 ) ;
#13640 = DIRECTION ( 'NONE',  ( 0.000000000000000000, 0.000000000000000000, 1.000000000000000000 ) ) ;
#13641 = VECTOR ( 'NONE', #34609, 1000.000000000000227 ) ;
#13642 = CARTESIAN_POINT ( 'NONE',  ( 0.000000000000000000, 0.000000000000000000, 0.000000000000000000 ) ) ;
#13643 = VECTOR ( 'NONE', #48279, 1000.000000000000000 ) ;
#13644 = ADVANCED_FACE ( 'NONE', ( #24632 ), #42995, .T. ) ;
#13645 = CARTESIAN_POINT ( 'NONE',  ( 0.000000000000000000, -120.0000000000000000, -2.500000000000000000 ) ) ;
#13646 = DIRECTION ( 'NONE',  ( -1.000000000000000000, 0.000000000000000000, 0.000000000000000000 ) ) ;
#13647 = VECTOR ( 'NONE', #8619, 1000.000000000000000 ) ;
#13648 = DIRECTION ( 'NONE',  ( 0.000000000000000000, 0.5877852522924696954, -0.8090169943749498938 ) ) ;
#13649 = EDGE_CURVE ( 'NONE', #45643, #994, #23639, .T. ) ;
#13650 = CARTESIAN_POINT ( 'NONE',  ( 10.00000000000000000, 59.46389618802034960, -49.70050353004825894 ) ) ;
#13651 = CARTESIAN_POINT ( 'NONE',  ( -11.99999999999999645, 2.553388576222231231E-15, 20.69999999999999929 ) ) ;
#13652 = AXIS2_PLACEMENT_3D ( 'NONE', #42463, #41500, #41747 ) ;
#13653 = VECTOR ( 'NONE', #28167, 1000.000000000000000 ) ;
#13654 = EDGE_LOOP ( 'NONE', ( #15330, #35152, #41147, #39676 ) ) ;
#13655 = CIRCLE ( 'NONE', #3483, 16.00000000000000000 ) ;
#13656 = CARTESIAN_POINT ( 'NONE',  ( 0.000000000000000000, 17.28742895386084655, 75.54627589209950145 ) ) ;
#13657 = ORIENTED_EDGE ( 'NONE', *, *, #23488, .F. ) ;
#13658 = AXIS2_PLACEMENT_3D ( 'NONE', #19152, #8857, #8382 ) ;
#13659 = LINE ( 'NONE', #6316, #7423 ) ;
#13660 = AXIS2_PLACEMENT_3D ( 'NONE', #43572, #24012, #16902 ) ;
#13661 = LINE ( 'NONE', #3539, #40395 ) ;
#13662 = CARTESIAN_POINT ( 'NONE',  ( -14.09999999999999964, 1.726751986797767995E-15, -1.199999999999999956 ) ) ;
#13663 = ORIENTED_EDGE ( 'NONE', *, *, #45758, .T. ) ;
#13664 = FACE_OUTER_BOUND ( 'NONE', #35395, .T. ) ;
#13665 = ADVANCED_FACE ( 'NONE', ( #24381 ), #39314, .T. ) ;
#13666 = VECTOR ( 'NONE', #16068, 1000.000000000000000 ) ;
#13667 = ADVANCED_FACE ( 'NONE', ( #31992 ), #47136, .T. ) ;
#13668 = EDGE_CURVE ( 'NONE', #9886, #1706, #8011, .T. ) ;
#13669 = CARTESIAN_POINT ( 'NONE',  ( 10.00000000000000000, 35.91791733033475253, 68.67312586195009771 ) ) ;
#13670 = LINE ( 'NONE', #35699, #41228 ) ;
#13671 = VERTEX_POINT ( 'NONE', #41013 ) ;
#13672 = LINE ( 'NONE', #29068, #3631 ) ;
#13673 = DIRECTION ( 'NONE',  ( -1.000000000000000000, -0.000000000000000000, 0.000000000000000000 ) ) ;
#13674 = DIRECTION ( 'NONE',  ( -1.000000000000000000, 0.000000000000000000, -0.000000000000000000 ) ) ;
#13675 = DIRECTION ( 'NONE',  ( -1.000000000000000000, -0.000000000000000000, 0.000000000000000000 ) ) ;
#13676 = ORIENTED_EDGE ( 'NONE', *, *, #41461, .T. ) ;
#13677 = EDGE_CURVE ( 'NONE', #15673, #24295, #17982, .T. ) ;
#13678 = EDGE_LOOP ( 'NONE', ( #45168, #28516, #5084, #25891 ) ) ;
#13679 = AXIS2_PLACEMENT_3D ( 'NONE', #34712, #16365, #35441 ) ;
#13680 = VECTOR ( 'NONE', #4018, 1000.000000000000000 ) ;
#13681 = VERTEX_POINT ( 'NONE', #43944 ) ;
#13682 = DIRECTION ( 'NONE',  ( 0.000000000000000000, 0.000000000000000000, 1.000000000000000000 ) ) ;
#13683 = CARTESIAN_POINT ( 'NONE',  ( 11.99999999999999822, 44.99326035066052754, 68.55367621811160461 ) ) ;
#13684 = ORIENTED_EDGE ( 'NONE', *, *, #45691, .F. ) ;
#13685 = ORIENTED_EDGE ( 'NONE', *, *, #48236, .F. ) ;
#13686 = VECTOR ( 'NONE', #24591, 1000.000000000000000 ) ;
#13687 = AXIS2_PLACEMENT_3D ( 'NONE', #36115, #35645, #2825 ) ;
#13688 = LINE ( 'NONE', #40829, #6971 ) ;
#13689 = VERTEX_POINT ( 'NONE', #32684 ) ;
#13690 = VERTEX_POINT ( 'NONE', #3552 ) ;
#13691 = VECTOR ( 'NONE', #2923, 1000.000000000000000 ) ;
#13692 = ORIENTED_EDGE ( 'NONE', *, *, #15889, .F. ) ;
#13693 = AXIS2_PLACEMENT_3D ( 'NONE', #7251, #3826, #37357 ) ;
#13694 = LINE ( 'NONE', #14169, #1632 ) ;
#13695 = ADVANCED_FACE ( 'NONE', ( #22406 ), #26318, .T. ) ;
#13696 = ORIENTED_EDGE ( 'NONE', *, *, #14085, .F. ) ;
#13697 = DIRECTION ( 'NONE',  ( 1.000000000000000000, 0.000000000000000000, 0.000000000000000000 ) ) ;
#13698 = ORIENTED_EDGE ( 'NONE', *, *, #11608, .T. ) ;
#13699 = DIRECTION ( 'NONE',  ( -1.000000000000000000, 0.000000000000000000, 0.000000000000000000 ) ) ;
#13700 = EDGE_CURVE ( 'NONE', #39957, #45900, #40072, .T. ) ;
#13701 = CIRCLE ( 'NONE', #28553, 31.99999999999999289 ) ;
#13702 = DIRECTION ( 'NONE',  ( 0.000000000000000000, 0.000000000000000000, -1.000000000000000000 ) ) ;
#13703 = FACE_OUTER_BOUND ( 'NONE', #21089, .T. ) ;
#13704 = EDGE_CURVE ( 'NONE', #47811, #2023, #11401, .T. ) ;
#13705 = ORIENTED_EDGE ( 'NONE', *, *, #27938, .F. ) ;
#13706 = DIRECTION ( 'NONE',  ( 0.000000000000000000, 0.000000000000000000, 1.000000000000000000 ) ) ;
#13707 = EDGE_LOOP ( 'NONE', ( #22408, #43979, #2724, #6867, #7486, #33000, #7797, #45539, #11431, #4636, #11023, #37587, #9348, #16648, #12254, #7997, #35054, #9511, #2009, #47775, #841, #22779, #21272, #47623, #44090, #15913, #27885, #30327, #46365, #27411, #25549, #37043, #45791, #29875, #45069, #42110, #7412, #31358, #43597, #36495, #29634, #29285, #20237, #5034, #41505, #21755, #32859, #27170, #16769, #32855, #10753, #33480, #20373, #1335, #40875, #35940, #2206, #568, #39263, #13578, #21460, #40305, #23129, #42068, #1126, #933, #36876, #47164, #18227, #47698, #47378, #9283, #27364, #6585, #18213, #39918, #46378, #14928, #28103, #28187, #17055, #1403, #28699, #16225, #3080, #18682, #834, #6112, #21825, #10556, #20929, #7356, #20255, #30923, #30831, #5317, #12492, #42916, #12370, #30919, #32996, #47402, #16210, #25828, #34397, #5812, #36722, #24065, #7557, #44040, #21040, #6547, #37052, #30283, #504, #5382, #33160, #38376, #18393, #15405, #3476, #30986, #36707, #27111, #6933, #11837, #43891, #10691, #6173, #7767, #31994, #20396, #41269, #44130, #25714, #3703, #35610, #27910, #27857, #391, #11309, #37475, #30383, #48106, #23750, #11523, #43780, #42606, #12420, #4829, #40005, #42883, #30701, #30027, #41220, #20979, #22729, #21925, #2019, #13491, #48168, #44565, #45730, #14340, #45163, #29532, #48099, #11345, #2474, #40312, #46919, #31390, #37169, #43949, #4488, #34488, #34626, #16187, #7650, #5929, #47804, #43569, #384, #34141, #8457, #24704, #30313, #25007, #39575, #43565, #26619, #9399, #2364, #17420, #12985, #30813, #38910, #41827, #12320, #586, #35329, #21122, #35751, #7792, #34974, #15789, #45835, #39426, #29818, #22531, #39652, #47716, #35116, #5514, #17670, #9849, #5560, #34955, #16863, #6727, #12598, #16328, #20977, #17458, #32470, #15356, #35300, #41951, #13763, #25877, #11512, #5868, #18622, #43056, #12147, #37879, #46855, #46987, #40008, #18073, #2077, #46762, #35685, #4550, #44164, #39843, #7886, #11236, #48260, #41276, #21498, #48174, #42056, #36598, #12656, #3223, #39537, #42170, #31508, #47782, #43453, #47032, #31532, #34790, #41312, #4180, #39723, #36490, #45177, #42745, #8325, #3653, #2746, #10870, #9940, #527, #45698, #3309, #27862, #40606, #2008, #42245, #3100, #38586, #19330, #38061, #41633, #35482, #41678, #34225, #5381, #5489, #20205, #36131, #29231, #11626, #23149, #11824, #32914, #2887, #2387, #27777, #10571, #34125, #10730, #15911, #22878, #28437, #43607, #29862, #23555, #35949, #34827, #11952, #45802, #8991, #1483, #33038, #19213, #15700, #4335, #29927, #22100, #36673, #13685 ) ) ;
#13708 = EDGE_LOOP ( 'NONE', ( #46471, #5347, #12196, #6526 ) ) ;
#13709 = CARTESIAN_POINT ( 'NONE',  ( 0.000000000000000000, 17.28742895386189105, -75.54627589209924565 ) ) ;
#13710 = VECTOR ( 'NONE', #33091, 1000.000000000000000 ) ;
#13711 = CARTESIAN_POINT ( 'NONE',  ( 0.000000000000000000, 0.000000000000000000, 0.000000000000000000 ) ) ;
#13712 = ORIENTED_EDGE ( 'NONE', *, *, #18312, .F. ) ;
#13713 = ORIENTED_EDGE ( 'NONE', *, *, #14915, .F. ) ;
#13714 = CARTESIAN_POINT ( 'NONE',  ( 0.000000000000000000, 80.28980883073758434, 16.65972982744963460 ) ) ;
#13715 = DIRECTION ( 'NONE',  ( 0.000000000000000000, 0.4539904997395479702, -0.8910065241883673437 ) ) ;
#13716 = ORIENTED_EDGE ( 'NONE', *, *, #197, .F. ) ;
#13717 = VERTEX_POINT ( 'NONE', #26065 ) ;
#13718 = LINE ( 'NONE', #21279, #42579 ) ;
#13719 = FACE_OUTER_BOUND ( 'NONE', #14183, .T. ) ;
#13720 = CARTESIAN_POINT ( 'NONE',  ( 0.000000000000000000, 63.97538442413498672, -51.29473840253155004 ) ) ;
#13721 = DIRECTION ( 'NONE',  ( -1.000000000000000000, 0.000000000000000000, 0.000000000000000000 ) ) ;
#13722 = EDGE_CURVE ( 'NONE', #6056, #31411, #33642, .T. ) ;
#13723 = EDGE_CURVE ( 'NONE', #40761, #8066, #10903, .T. ) ;
#13724 = CARTESIAN_POINT ( 'NONE',  ( 0.000000000000000000, 0.000000000000000000, 0.000000000000000000 ) ) ;
#13725 = ORIENTED_EDGE ( 'NONE', *, *, #3025, .T. ) ;
#13726 = AXIS2_PLACEMENT_3D ( 'NONE', #6885, #22041, #14477 ) ;
#13727 = CIRCLE ( 'NONE', #40284, 31.99999999999998579 ) ;
#13728 = CARTESIAN_POINT ( 'NONE',  ( -6.782329983125267248, 10.49999999999999645, -125.0000000000000000 ) ) ;
#13729 = DIRECTION ( 'NONE',  ( 0.000000000000000000, 0.6494480483301793283, 0.7604059656000345946 ) ) ;
#13730 = FACE_OUTER_BOUND ( 'NONE', #2633, .T. ) ;
#13731 = CARTESIAN_POINT ( 'NONE',  ( 0.000000000000000000, -65.64334221924882229, -41.19522573413803457 ) ) ;
#13732 = CARTESIAN_POINT ( 'NONE',  ( 5.000000000000002665, 15.33399622253481986, 80.55351364060595643 ) ) ;
#13733 = CARTESIAN_POINT ( 'NONE',  ( 10.00000000000000000, -31.47745569255189224, 68.26794271651249346 ) ) ;
#13734 = VECTOR ( 'NONE', #41759, 999.9999999999998863 ) ;
#13735 = DIRECTION ( 'NONE',  ( 0.000000000000000000, -0.9238795325112906243, 0.3826834323650805114 ) ) ;
#13736 = EDGE_LOOP ( 'NONE', ( #37970, #31153, #39733, #36174 ) ) ;
#13737 = ORIENTED_EDGE ( 'NONE', *, *, #18529, .F. ) ;
#13738 = ADVANCED_FACE ( 'NONE', ( #15058 ), #37329, .T. ) ;
#13739 = ORIENTED_EDGE ( 'NONE', *, *, #31180, .F. ) ;
#13740 = CIRCLE ( 'NONE', #39528, 1.000000000000000888 ) ;
#13741 = DIRECTION ( 'NONE',  ( -1.000000000000000000, 0.000000000000000000, 0.000000000000000000 ) ) ;
#13742 = AXIS2_PLACEMENT_3D ( 'NONE', #19687, #1106, #5028 ) ;
#13743 = AXIS2_PLACEMENT_3D ( 'NONE', #35554, #20610, #8620 ) ;
#13744 = DIRECTION ( 'NONE',  ( -0.000000000000000000, -0.000000000000000000, -1.000000000000000000 ) ) ;
#13745 = ORIENTED_EDGE ( 'NONE', *, *, #30357, .T. ) ;
#13746 = CIRCLE ( 'NONE', #35654, 15.99999999999999645 ) ;
#13747 = ORIENTED_EDGE ( 'NONE', *, *, #20845, .F. ) ;
#13748 = CARTESIAN_POINT ( 'NONE',  ( 10.00000000000000000, 0.8828120875905820508, -37.48860685352290290 ) ) ;
#13749 = ORIENTED_EDGE ( 'NONE', *, *, #27705, .F. ) ;
#13750 = CARTESIAN_POINT ( 'NONE',  ( 0.000000000000000000, 0.000000000000000000, -43.79999999999998295 ) ) ;
#13751 = VERTEX_POINT ( 'NONE', #48340 ) ;
#13752 = PRESENTATION_STYLE_ASSIGNMENT (( #40644 ) ) ;
#13753 = VECTOR ( 'NONE', #20541, 1000.000000000000000 ) ;
#13754 = VERTEX_POINT ( 'NONE', #33175 ) ;
#13755 = CYLINDRICAL_SURFACE ( 'NONE', #18795, 77.49899999999999523 ) ;
#13756 = ORIENTED_EDGE ( 'NONE', *, *, #47465, .F. ) ;
#13757 = LINE ( 'NONE', #35781, #15659 ) ;
#13758 = ORIENTED_EDGE ( 'NONE', *, *, #11964, .T. ) ;
#13759 = DIRECTION ( 'NONE',  ( -0.000000000000000000, -1.000000000000000000, -0.000000000000000000 ) ) ;
#13760 = ORIENTED_EDGE ( 'NONE', *, *, #10625, .T. ) ;
#13761 = EDGE_CURVE ( 'NONE', #33430, #41296, #41641, .T. ) ;
#13762 = CIRCLE ( 'NONE', #46615, 82.00000000000000000 ) ;
#13763 = ORIENTED_EDGE ( 'NONE', *, *, #9650, .F. ) ;
#13764 = DIRECTION ( 'NONE',  ( -1.000000000000000000, 0.000000000000000000, 0.000000000000000000 ) ) ;
#13765 = CIRCLE ( 'NONE', #38755, 82.00000000000000000 ) ;
#13766 = EDGE_CURVE ( 'NONE', #36599, #26190, #11142, .T. ) ;
#13767 = FACE_OUTER_BOUND ( 'NONE', #33389, .T. ) ;
#13768 = DIRECTION ( 'NONE',  ( -1.000000000000000000, 0.000000000000000000, -0.000000000000000000 ) ) ;
#13770 = ORIENTED_EDGE ( 'NONE', *, *, #17179, .T. ) ;
#13769 = CARTESIAN_POINT ( 'NONE',  ( 0.000000000000000000, -77.19088730480518734, -6.903761155838607166 ) ) ;
#13771 = CARTESIAN_POINT ( 'NONE',  ( 10.00000000000000000, -12.26510123303234501, -35.53030884539098366 ) ) ;
#13772 = ORIENTED_EDGE ( 'NONE', *, *, #21101, .T. ) ;
#13773 = LINE ( 'NONE', #28700, #48267 ) ;
#13774 = VERTEX_POINT ( 'NONE', #3792 ) ;
#13775 = ORIENTED_EDGE ( 'NONE', *, *, #5451, .F. ) ;
#13776 = ADVANCED_FACE ( 'NONE', ( #47843 ), #36597, .T. ) ;
#13777 = DIRECTION ( 'NONE',  ( -1.000000000000000000, -0.000000000000000000, 0.000000000000000000 ) ) ;
#13778 = VERTEX_POINT ( 'NONE', #29981 ) ;
#13779 = DIRECTION ( 'NONE',  ( 0.000000000000000000, -0.2334453638559127742, 0.9723699203976748917 ) ) ;
#13780 = VECTOR ( 'NONE', #32621, 1000.000000000000000 ) ;
#13781 = DIRECTION ( 'NONE',  ( -1.000000000000000000, -0.000000000000000000, -0.000000000000000000 ) ) ;
#13782 = CARTESIAN_POINT ( 'NONE',  ( -10.00000000000000000, 0.000000000000000000, 0.000000000000000000 ) ) ;
#13783 = ORIENTED_EDGE ( 'NONE', *, *, #113, .T. ) ;
#13784 = DIRECTION ( 'NONE',  ( -1.000000000000000000, 0.000000000000000000, 0.000000000000000000 ) ) ;
#13785 = AXIS2_PLACEMENT_3D ( 'NONE', #30145, #7851, #33321 ) ;
#13786 = DIRECTION ( 'NONE',  ( 0.000000000000000000, 0.000000000000000000, 1.000000000000000000 ) ) ;
#13787 = CARTESIAN_POINT ( 'NONE',  ( 0.000000000000000000, -16.23288003029473359, -33.80338159004301701 ) ) ;
#13788 = ADVANCED_FACE ( 'NONE', ( #14817 ), #40756, .T. ) ;
#13789 = CIRCLE ( 'NONE', #45049, 31.99999999999999289 ) ;
#13790 = DIRECTION ( 'NONE',  ( 0.000000000000000000, 0.000000000000000000, 1.000000000000000000 ) ) ;
#13791 = CARTESIAN_POINT ( 'NONE',  ( 0.000000000000000000, -12.42422080174663712, 35.38097989696507994 ) ) ;
#13792 = EDGE_CURVE ( 'NONE', #13231, #28317, #10413, .T. ) ;
#13793 = DIRECTION ( 'NONE',  ( -1.000000000000000000, 0.000000000000000000, 0.000000000000000000 ) ) ;
#13794 = CARTESIAN_POINT ( 'NONE',  ( -10.00000000000000000, 0.000000000000000000, 0.000000000000000000 ) ) ;
#13795 = LINE ( 'NONE', #21611, #13780 ) ;
#13796 = CARTESIAN_POINT ( 'NONE',  ( 1.192633404626820770, -120.9097392825245407, -2.500000000000000000 ) ) ;
#13797 = CARTESIAN_POINT ( 'NONE',  ( 0.000000000000000000, 0.8261519478441983200, -77.49459641780885022 ) ) ;
#13798 = EDGE_CURVE ( 'NONE', #34257, #31329, #32994, .T. ) ;
#13799 = ORIENTED_EDGE ( 'NONE', *, *, #11939, .F. ) ;
#13800 = AXIS2_PLACEMENT_3D ( 'NONE', #25650, #22713, #48183 ) ;
#13801 = CYLINDRICAL_SURFACE ( 'NONE', #39437, 82.00000000000000000 ) ;
#13802 = EDGE_LOOP ( 'NONE', ( #14284, #2491, #28785, #7315 ) ) ;
#13803 = DIRECTION ( 'NONE',  ( -1.000000000000000000, -0.000000000000000000, 0.000000000000000000 ) ) ;
#13804 = VECTOR ( 'NONE', #537, 1000.000000000000114 ) ;
#13805 = CARTESIAN_POINT ( 'NONE',  ( 10.00000000000000000, 0.000000000000000000, 0.000000000000000000 ) ) ;
#13806 = ORIENTED_EDGE ( 'NONE', *, *, #41138, .F. ) ;
#13807 = VERTEX_POINT ( 'NONE', #37566 ) ;
#13808 = EDGE_CURVE ( 'NONE', #12269, #28196, #29262, .T. ) ;
#13809 = CIRCLE ( 'NONE', #26314, 77.49899999999999523 ) ;
#13810 = DIRECTION ( 'NONE',  ( -1.000000000000000000, -0.000000000000000000, -0.000000000000000000 ) ) ;
#13811 = VERTEX_POINT ( 'NONE', #25330 ) ;
#13812 = EDGE_LOOP ( 'NONE', ( #28768, #12253, #39651, #46076 ) ) ;
#13813 = AXIS2_PLACEMENT_3D ( 'NONE', #21725, #28824, #32730 ) ;
#13814 = ORIENTED_EDGE ( 'NONE', *, *, #814, .T. ) ;
#13815 = AXIS2_PLACEMENT_3D ( 'NONE', #32976, #44248, #10952 ) ;
#13816 = CARTESIAN_POINT ( 'NONE',  ( -12.00000000000000000, 0.000000000000000000, -17.30399999999999849 ) ) ;
#13817 = EDGE_LOOP ( 'NONE', ( #4967, #12360, #35609, #20466 ) ) ;
#13818 = EDGE_CURVE ( 'NONE', #18357, #1286, #26823, .T. ) ;
#13819 = DIRECTION ( 'NONE',  ( 0.000000000000000000, -0.5000000000000039968, -0.8660254037844363761 ) ) ;
#13820 = CARTESIAN_POINT ( 'NONE',  ( 8.700667342345820288, -98.11853780484867116, -2.500000000000000000 ) ) ;
#13821 = EDGE_LOOP ( 'NONE', ( #45514, #7615, #10711, #19056 ) ) ;
#13822 = ADVANCED_FACE ( 'NONE', ( #23122 ), #23358, .T. ) ;
#13823 = DIRECTION ( 'NONE',  ( 1.000000000000000000, 0.000000000000000000, 0.000000000000000000 ) ) ;
#13824 = ORIENTED_EDGE ( 'NONE', *, *, #30546, .T. ) ;
#13825 = EDGE_CURVE ( 'NONE', #25099, #37634, #19430, .T. ) ;
#13826 = AXIS2_PLACEMENT_3D ( 'NONE', #25563, #47595, #25083 ) ;
#13827 = DIRECTION ( 'NONE',  ( -1.000000000000000000, -0.000000000000000000, -0.000000000000000000 ) ) ;
#13828 = DIRECTION ( 'NONE',  ( 0.000000000000000000, 0.9945218953682742891, -0.1045284632676436315 ) ) ;
#13829 = DIRECTION ( 'NONE',  ( 0.000000000000000000, 0.5877852522924685852, 0.8090169943749508930 ) ) ;
#13830 = EDGE_CURVE ( 'NONE', #41873, #12437, #36177, .T. ) ;
#13831 = CIRCLE ( 'NONE', #33353, 77.49900000000000944 ) ;
#13832 = ORIENTED_EDGE ( 'NONE', *, *, #32230, .T. ) ;
#13833 = DIRECTION ( 'NONE',  ( -1.000000000000000000, 0.000000000000000000, -0.000000000000000000 ) ) ;
#13834 = ORIENTED_EDGE ( 'NONE', *, *, #43653, .F. ) ;
#13835 = ORIENTED_EDGE ( 'NONE', *, *, #34986, .T. ) ;
#13836 = EDGE_CURVE ( 'NONE', #24941, #45240, #2565, .T. ) ;
#13837 = FACE_BOUND ( 'NONE', #46428, .T. ) ;
#13838 = AXIS2_PLACEMENT_3D ( 'NONE', #939, #34233, #26910 ) ;
#13839 = DIRECTION ( 'NONE',  ( 0.000000000000000000, -0.5877852522924689183, -0.8090169943749504489 ) ) ;
#13840 = DIRECTION ( 'NONE',  ( -1.000000000000000000, -0.000000000000000000, 0.000000000000000000 ) ) ;
#13841 = LINE ( 'NONE', #6726, #26613 ) ;
#13842 = CARTESIAN_POINT ( 'NONE',  ( -12.50000000000000000, -107.5000000000000000, -2.500000000000000000 ) ) ;
#13843 = LINE ( 'NONE', #35372, #41634 ) ;
#13844 = CARTESIAN_POINT ( 'NONE',  ( 0.000000000000000000, -59.03342792756297541, 46.54456581323783126 ) ) ;
#13845 = FACE_OUTER_BOUND ( 'NONE', #47608, .T. ) ;
#13846 = DIRECTION ( 'NONE',  ( 0.08130631524010120681, -0.9966891607226784355, 0.000000000000000000 ) ) ;
#13847 = DIRECTION ( 'NONE',  ( 0.000000000000000000, 0.000000000000000000, -1.000000000000000000 ) ) ;
#13848 = EDGE_LOOP ( 'NONE', ( #30267, #37173, #17096, #4700 ) ) ;
#13849 = AXIS2_PLACEMENT_3D ( 'NONE', #27035, #8420, #38280 ) ;
#13850 = CARTESIAN_POINT ( 'NONE',  ( -6.170112525937308412, 10.87104923258428890, 42.00000000000001421 ) ) ;
#13851 = CARTESIAN_POINT ( 'NONE',  ( 14.09999999999999964, 0.000000000000000000, 0.000000000000000000 ) ) ;
#13852 = LINE ( 'NONE', #9203, #40138 ) ;
#13853 = ORIENTED_EDGE ( 'NONE', *, *, #45342, .F. ) ;
#13854 = PLANE ( 'NONE',  #16883 ) ;
#13855 = AXIS2_PLACEMENT_3D ( 'NONE', #12409, #38846, #17028 ) ;
#13856 = EDGE_CURVE ( 'NONE', #15854, #23327, #4759, .T. ) ;
#13857 = LINE ( 'NONE', #39802, #11513 ) ;
#13858 = DIRECTION ( 'NONE',  ( 1.000000000000000000, -0.000000000000000000, -0.000000000000000000 ) ) ;
#13859 = VERTEX_POINT ( 'NONE', #34857 ) ;
#13860 = CYLINDRICAL_SURFACE ( 'NONE', #48052, 82.00000000000000000 ) ;
#13861 = EDGE_CURVE ( 'NONE', #28645, #40027, #6494, .T. ) ;
#13862 = CYLINDRICAL_SURFACE ( 'NONE', #21289, 77.49899999999999523 ) ;
#13863 = ORIENTED_EDGE ( 'NONE', *, *, #31424, .T. ) ;
#13864 = VERTEX_POINT ( 'NONE', #27523 ) ;
#13865 = AXIS2_PLACEMENT_3D ( 'NONE', #3520, #40263, #43914 ) ;
#13866 = ORIENTED_EDGE ( 'NONE', *, *, #34907, .T. ) ;
#13867 = EDGE_LOOP ( 'NONE', ( #3098, #3444, #25159, #17655 ) ) ;
#13868 = CIRCLE ( 'NONE', #47461, 82.00000000000000000 ) ;
#13869 = CYLINDRICAL_SURFACE ( 'NONE', #7804, 16.00000000000000000 ) ;
#13870 = ORIENTED_EDGE ( 'NONE', *, *, #33417, .T. ) ;
#13871 = ORIENTED_EDGE ( 'NONE', *, *, #41936, .T. ) ;
#13872 = AXIS2_PLACEMENT_3D ( 'NONE', #31134, #27950, #39187 ) ;
#13873 = ADVANCED_FACE ( 'NONE', ( #22874 ), #8910, .T. ) ;
#13874 = DIRECTION ( 'NONE',  ( 0.000000000000000000, 7.228014483236689653E-16, -1.000000000000000000 ) ) ;
#13875 = CARTESIAN_POINT ( 'NONE',  ( -0.4966694826856976608, -121.4153866697721611, 2.500000000000000000 ) ) ;
#13876 = ORIENTED_EDGE ( 'NONE', *, *, #22210, .T. ) ;
#13877 = ORIENTED_EDGE ( 'NONE', *, *, #1551, .F. ) ;
#13878 = EDGE_CURVE ( 'NONE', #15085, #28664, #833, .T. ) ;
#13879 = DIRECTION ( 'NONE',  ( 0.000000000000000000, 0.000000000000000000, 1.000000000000000000 ) ) ;
#13880 = DIRECTION ( 'NONE',  ( -1.000000000000000000, -0.000000000000000000, -0.000000000000000000 ) ) ;
#13881 = CARTESIAN_POINT ( 'NONE',  ( 0.000000000000000000, -22.67460108101774807, -6.353146135318215038 ) ) ;
#13882 = ORIENTED_EDGE ( 'NONE', *, *, #35868, .T. ) ;
#13883 = EDGE_LOOP ( 'NONE', ( #17664, #45388, #45652, #47715 ) ) ;
#13884 = CYLINDRICAL_SURFACE ( 'NONE', #22390, 82.00000000000000000 ) ;
#13885 = VERTEX_POINT ( 'NONE', #4525 ) ;
#13886 = EDGE_CURVE ( 'NONE', #127, #45331, #31524, .T. ) ;
#13887 = FACE_OUTER_BOUND ( 'NONE', #48109, .T. ) ;
#13888 = ADVANCED_FACE ( 'NONE', ( #30238 ), #607, .T. ) ;
#13889 = DIRECTION ( 'NONE',  ( 0.000000000000000000, 0.6691306063588563502, 0.7431448254773960205 ) ) ;
#13890 = DIRECTION ( 'NONE',  ( 0.000000000000000000, 0.2079116908177641720, 0.9781476007338045786 ) ) ;
#13891 = CARTESIAN_POINT ( 'NONE',  ( 0.000000000000000000, -60.67117009219096957, -55.16347631943106933 ) ) ;
#13892 = DIRECTION ( 'NONE',  ( -1.000000000000000000, -0.000000000000000000, -0.000000000000000000 ) ) ;
#13893 = DIRECTION ( 'NONE',  ( 0.000000000000000000, 0.8660254037844432595, -0.4999999999999920064 ) ) ;
#13894 = AXIS2_PLACEMENT_3D ( 'NONE', #21, #19575, #34512 ) ;
#13895 = ORIENTED_EDGE ( 'NONE', *, *, #38182, .T. ) ;
#13896 = DIRECTION ( 'NONE',  ( 0.000000000000000000, -0.8660254037844363761, -0.5000000000000039968 ) ) ;
#13897 = ORIENTED_EDGE ( 'NONE', *, *, #13441, .F. ) ;
#13898 = CARTESIAN_POINT ( 'NONE',  ( -10.00000000000000000, 0.000000000000000000, 0.000000000000000000 ) ) ;
#13899 = DIRECTION ( 'NONE',  ( 1.000000000000000000, 0.000000000000000000, -0.000000000000000000 ) ) ;
#13900 = DIRECTION ( 'NONE',  ( -1.000000000000000000, 0.000000000000000000, 0.000000000000000000 ) ) ;
#13901 = FACE_OUTER_BOUND ( 'NONE', #6392, .T. ) ;
#13902 = CARTESIAN_POINT ( 'NONE',  ( 10.00000000000000000, 0.000000000000000000, 0.000000000000000000 ) ) ;
#13903 = LINE ( 'NONE', #17806, #23256 ) ;
#13904 = ORIENTED_EDGE ( 'NONE', *, *, #24051, .T. ) ;
#13905 = PLANE ( 'NONE',  #6792 ) ;
#13906 = CARTESIAN_POINT ( 'NONE',  ( -13.05994868825747446, -139.5943292883446532, 5.500000000000000000 ) ) ;
#13907 = CARTESIAN_POINT ( 'NONE',  ( 10.00000000000000000, 0.000000000000000000, 0.000000000000000000 ) ) ;
#13908 = CARTESIAN_POINT ( 'NONE',  ( 10.00000000000000000, 0.000000000000000000, 0.000000000000000000 ) ) ;
#13909 = ORIENTED_EDGE ( 'NONE', *, *, #19721, .F. ) ;
#13910 = ORIENTED_EDGE ( 'NONE', *, *, #37128, .F. ) ;
#13911 = AXIS2_PLACEMENT_3D ( 'NONE', #26824, #41760, #34632 ) ;
#13912 = EDGE_CURVE ( 'NONE', #37888, #3320, #26792, .T. ) ;
#13913 = DIRECTION ( 'NONE',  ( -1.000000000000000000, 0.000000000000000000, 0.000000000000000000 ) ) ;
#13914 = CARTESIAN_POINT ( 'NONE',  ( 10.00000000000000000, -15.48615015657555816, -39.04073710021360455 ) ) ;
#13915 = EDGE_CURVE ( 'NONE', #17387, #7054, #41726, .T. ) ;
#13916 = EDGE_LOOP ( 'NONE', ( #21946, #41736, #34725, #3005 ) ) ;
#13917 = CIRCLE ( 'NONE', #31130, 77.49899999999999523 ) ;
#13918 = CARTESIAN_POINT ( 'NONE',  ( 0.000000000000000000, -39.47590169984898978, 71.87247863392400404 ) ) ;
#13919 = AXIS2_PLACEMENT_3D ( 'NONE', #12681, #23942, #31537 ) ;
#13920 = ORIENTED_EDGE ( 'NONE', *, *, #32356, .T. ) ;
#13921 = ORIENTED_EDGE ( 'NONE', *, *, #42208, .F. ) ;
#13922 = VERTEX_POINT ( 'NONE', #12128 ) ;
#13923 = EDGE_CURVE ( 'NONE', #9910, #30912, #41981, .T. ) ;
#13924 = AXIS2_PLACEMENT_3D ( 'NONE', #42281, #16576, #28315 ) ;
#13925 = EDGE_CURVE ( 'NONE', #20359, #35932, #8430, .T. ) ;
#13926 = EDGE_CURVE ( 'NONE', #6721, #34257, #9582, .T. ) ;
#13927 = FACE_OUTER_BOUND ( 'NONE', #15381, .T. ) ;
#13928 = ORIENTED_EDGE ( 'NONE', *, *, #35476, .T. ) ;
#13929 = DIRECTION ( 'NONE',  ( 0.000000000000000000, 0.000000000000000000, 1.000000000000000000 ) ) ;
#13930 = ORIENTED_EDGE ( 'NONE', *, *, #16573, .T. ) ;
#13931 = DIRECTION ( 'NONE',  ( -1.000000000000000000, -0.000000000000000000, -0.000000000000000000 ) ) ;
#13932 = ADVANCED_FACE ( 'NONE', ( #42200 ), #33884, .T. ) ;
#13933 = DIRECTION ( 'NONE',  ( 0.000000000000000000, 0.000000000000000000, 1.000000000000000000 ) ) ;
#13934 = PRODUCT_DEFINITION_FORMATION_WITH_SPECIFIED_SOURCE ( 'ANY', '', #40211, .NOT_KNOWN. ) ;
#13935 = CARTESIAN_POINT ( 'NONE',  ( 0.000000000000000000, 14.66109333815460225, 73.73191006444577056 ) ) ;
#13936 = VERTEX_POINT ( 'NONE', #38541 ) ;
#13937 = CARTESIAN_POINT ( 'NONE',  ( 10.00000000000000000, -71.91182617369167929, -28.89263327155822481 ) ) ;
#13938 = ORIENTED_EDGE ( 'NONE', *, *, #39699, .F. ) ;
#13939 = AXIS2_PLACEMENT_3D ( 'NONE', #21840, #29915, #3978 ) ;
#13940 = DIRECTION ( 'NONE',  ( -1.000000000000000000, -0.000000000000000000, -0.000000000000000000 ) ) ;
#13941 = LINE ( 'NONE', #28150, #14168 ) ;
#13942 = VERTEX_POINT ( 'NONE', #5003 ) ;
#13943 = ORIENTED_EDGE ( 'NONE', *, *, #48121, .T. ) ;
#13944 = CARTESIAN_POINT ( 'NONE',  ( 0.000000000000000000, -44.99326035066101781, 68.55367621811126355 ) ) ;
#13945 = DIRECTION ( 'NONE',  ( -1.000000000000000000, 0.000000000000000000, 0.000000000000000000 ) ) ;
#13946 = ORIENTED_EDGE ( 'NONE', *, *, #5209, .T. ) ;
#13947 = ORIENTED_EDGE ( 'NONE', *, *, #19485, .F. ) ;
#13948 = CARTESIAN_POINT ( 'NONE',  ( 11.99999999999999822, 72.35160999960844208, -20.41045688087747223 ) ) ;
#13949 = CARTESIAN_POINT ( 'NONE',  ( 0.000000000000000000, 0.000000000000000000, -125.0000000000000000 ) ) ;
#13950 = CYLINDRICAL_SURFACE ( 'NONE', #26899, 16.00000000000000000 ) ;
#13951 = DIRECTION ( 'NONE',  ( -1.000000000000000000, 0.000000000000000000, 0.000000000000000000 ) ) ;
#13952 = DIRECTION ( 'NONE',  ( -0.000000000000000000, 0.9781476007338066880, -0.2079116908177543743 ) ) ;
#13953 = DIRECTION ( 'NONE',  ( 0.000000000000000000, 0.000000000000000000, -1.000000000000000000 ) ) ;
#13954 = CARTESIAN_POINT ( 'NONE',  ( 10.00000000000000000, -0.6853352020787742971, -37.58145647212455032 ) ) ;
#13955 = AXIS2_PLACEMENT_3D ( 'NONE', #28576, #43510, #2151 ) ;
#13956 = DIRECTION ( 'NONE',  ( 0.000000000000000000, 0.9723699203976756689, 0.2334453638559095268 ) ) ;
#13957 = VECTOR ( 'NONE', #35691, 1000.000000000000000 ) ;
#13958 = CARTESIAN_POINT ( 'NONE',  ( 10.00000000000000000, 37.22597642581158084, 10.79786254984347593 ) ) ;
#13960 = AXIS2_PLACEMENT_3D ( 'NONE', #1360, #20675, #24112 ) ;
#13959 = CARTESIAN_POINT ( 'NONE',  ( 0.000000000000000000, 0.000000000000000000, 0.000000000000000000 ) ) ;
#13961 = CARTESIAN_POINT ( 'NONE',  ( 0.000000000000000000, 0.000000000000000000, 0.000000000000000000 ) ) ;
#13962 = EDGE_LOOP ( 'NONE', ( #2784, #45454, #5553, #48156 ) ) ;
#13963 = EDGE_CURVE ( 'NONE', #15289, #20089, #20561, .T. ) ;
#13964 = EDGE_LOOP ( 'NONE', ( #16721, #40354, #16017, #10489 ) ) ;
#13965 = EDGE_CURVE ( 'NONE', #361, #29885, #29146, .T. ) ;
#13966 = DIRECTION ( 'NONE',  ( -1.000000000000000000, 0.000000000000000000, -0.000000000000000000 ) ) ;
#13967 = EDGE_CURVE ( 'NONE', #17338, #45908, #2289, .T. ) ;
#13968 = ORIENTED_EDGE ( 'NONE', *, *, #15467, .F. ) ;
#13969 = CARTESIAN_POINT ( 'NONE',  ( 6.000000000000000000, 8.966570791700705811, 81.50828551894228724 ) ) ;
#13970 = EDGE_CURVE ( 'NONE', #37389, #31548, #9880, .T. ) ;
#13971 = ORIENTED_EDGE ( 'NONE', *, *, #3582, .T. ) ;
#13972 = CARTESIAN_POINT ( 'NONE',  ( 10.00000000000000000, 0.000000000000000000, 0.000000000000000000 ) ) ;
#13973 = LINE ( 'NONE', #25468, #40171 ) ;
#13974 = ORIENTED_EDGE ( 'NONE', *, *, #20449, .T. ) ;
#13975 =( NAMED_UNIT ( * ) PLANE_ANGLE_UNIT ( ) SI_UNIT ( $, .RADIAN. ) );
#13976 = EDGE_LOOP ( 'NONE', ( #1952, #12481, #30339, #29946 ) ) ;
#13977 = ADVANCED_FACE ( 'NONE', ( #42700 ), #35589, .T. ) ;
#13978 = EDGE_CURVE ( 'NONE', #45131, #23071, #11176, .T. ) ;
#13979 = VERTEX_POINT ( 'NONE', #39514 ) ;
#13980 = FACE_OUTER_BOUND ( 'NONE', #32630, .T. ) ;
#13981 = ORIENTED_EDGE ( 'NONE', *, *, #32008, .T. ) ;
#13982 = CIRCLE ( 'NONE', #9304, 82.00000000000000000 ) ;
#13983 = FACE_OUTER_BOUND ( 'NONE', #41170, .T. ) ;
#13984 = ORIENTED_EDGE ( 'NONE', *, *, #28959, .F. ) ;
#13985 = FACE_OUTER_BOUND ( 'NONE', #13334, .T. ) ;
#13986 = VERTEX_POINT ( 'NONE', #24325 ) ;
#13987 = CIRCLE ( 'NONE', #13196, 31.99999999999999289 ) ;
#13988 = CIRCLE ( 'NONE', #39796, 77.49899999999999523 ) ;
#13989 = FACE_OUTER_BOUND ( 'NONE', #19553, .T. ) ;
#13990 = VERTEX_POINT ( 'NONE', #39756 ) ;
#13991 = VECTOR ( 'NONE', #22369, 1000.000000000000000 ) ;
#13992 = DIRECTION ( 'NONE',  ( -1.000000000000000000, -0.000000000000000000, 0.000000000000000000 ) ) ;
#13993 = CARTESIAN_POINT ( 'NONE',  ( 11.99999999999999822, 0.000000000000000000, 0.000000000000000000 ) ) ;
#13994 = CARTESIAN_POINT ( 'NONE',  ( 103.9230484541331947, -179.9999999999990337, -5.500000000000000000 ) ) ;
#13995 = EDGE_CURVE ( 'NONE', #25106, #43867, #7252, .T. ) ;
#13996 = CARTESIAN_POINT ( 'NONE',  ( 11.99999999999999822, 0.000000000000000000, 0.000000000000000000 ) ) ;
#13997 = DIRECTION ( 'NONE',  ( -1.000000000000000000, 0.000000000000000000, -0.000000000000000000 ) ) ;
#13998 = ORIENTED_EDGE ( 'NONE', *, *, #12220, .T. ) ;
#13999 = CARTESIAN_POINT ( 'NONE',  ( 0.000000000000000000, 0.000000000000000000, 53.20000000000001705 ) ) ;
#14000 = ORIENTED_EDGE ( 'NONE', *, *, #30395, .F. ) ;
#14001 = ORIENTED_EDGE ( 'NONE', *, *, #3435, .T. ) ;
#14002 = CARTESIAN_POINT ( 'NONE',  ( 10.00000000000000000, 37.01155633439068282, -6.555932627142014191 ) ) ;
#14003 = DIRECTION ( 'NONE',  ( -1.000000000000000000, 0.000000000000000000, -0.000000000000000000 ) ) ;
#14004 = ORIENTED_EDGE ( 'NONE', *, *, #46551, .T. ) ;
#14005 = AXIS2_PLACEMENT_3D ( 'NONE', #17086, #46725, #5851 ) ;
#14006 = CARTESIAN_POINT ( 'NONE',  ( 10.00000000000000000, -59.03961581697367933, -46.53671651294010303 ) ) ;
#14007 = FACE_OUTER_BOUND ( 'NONE', #28637, .T. ) ;
#14008 = DIRECTION ( 'NONE',  ( -0.6862798483830533369, -0.7273375899149812085, 0.000000000000000000 ) ) ;
#14009 = ORIENTED_EDGE ( 'NONE', *, *, #30120, .T. ) ;
#14010 = PRODUCT_DEFINITION_SHAPE ( 'NONE', 'NONE',  #16380 ) ;
#14011 = CARTESIAN_POINT ( 'NONE',  ( 0.000000000000000000, 33.79645857604513992, 16.45098606841138178 ) ) ;
#14012 = DIRECTION ( 'NONE',  ( -1.000000000000000000, 0.000000000000000000, 0.000000000000000000 ) ) ;
#14013 = STYLED_ITEM ( 'NONE', ( #9504 ), #605 ) ;
#14014 = CARTESIAN_POINT ( 'NONE',  ( -0.9515373497862389396, -96.47140937769621871, -2.500000000000000000 ) ) ;
#14015 = ORIENTED_EDGE ( 'NONE', *, *, #27478, .F. ) ;
#14016 = DIRECTION ( 'NONE',  ( -1.000000000000000000, 0.000000000000000000, -0.000000000000000000 ) ) ;
#14017 = DIRECTION ( 'NONE',  ( 1.000000000000000000, 0.000000000000000000, 0.000000000000000000 ) ) ;
#14018 = CARTESIAN_POINT ( 'NONE',  ( 0.000000000000000000, 0.000000000000000000, 0.000000000000000000 ) ) ;
#14019 = DIRECTION ( 'NONE',  ( 0.000000000000000000, -0.9238795325112821866, -0.3826834323651006065 ) ) ;
#14020 = FACE_OUTER_BOUND ( 'NONE', #12676, .T. ) ;
#14021 = CARTESIAN_POINT ( 'NONE',  ( 10.00000000000000000, -36.72794159290288718, 65.59268652807197952 ) ) ;
#14022 = FACE_OUTER_BOUND ( 'NONE', #17589, .T. ) ;
#14023 = VERTEX_POINT ( 'NONE', #21125 ) ;
#14024 = ORIENTED_EDGE ( 'NONE', *, *, #15541, .F. ) ;
#14025 = CIRCLE ( 'NONE', #26541, 77.49900000000000944 ) ;
#14026 = EDGE_CURVE ( 'NONE', #5563, #28753, #42937, .T. ) ;
#14027 = CARTESIAN_POINT ( 'NONE',  ( 11.99999999999999822, 14.67089635893713684, 73.72996012237443608 ) ) ;
#14028 = CIRCLE ( 'NONE', #12491, 31.99999999999999645 ) ;
#14029 = EDGE_LOOP ( 'NONE', ( #11540, #41423, #43828, #6601 ) ) ;
#14030 = CARTESIAN_POINT ( 'NONE',  ( 12.69589495141918611, -96.69089767102708777, -5.500000000000000000 ) ) ;
#14032 = EDGE_CURVE ( 'NONE', #10055, #12035, #8052, .T. ) ;
#14031 = AXIS2_PLACEMENT_3D ( 'NONE', #28787, #36839, #31996 ) ;
#14033 = DIRECTION ( 'NONE',  ( -1.000000000000000000, 0.000000000000000000, -0.000000000000000000 ) ) ;
#14034 = EDGE_CURVE ( 'NONE', #23562, #18326, #9157, .T. ) ;
#14035 = ORIENTED_EDGE ( 'NONE', *, *, #15434, .T. ) ;
#14036 = AXIS2_PLACEMENT_3D ( 'NONE', #4257, #19170, #15743 ) ;
#14037 = EDGE_LOOP ( 'NONE', ( #11704, #5366, #25167, #15778 ) ) ;
#14038 = DIRECTION ( 'NONE',  ( -1.000000000000000000, 0.000000000000000000, -0.000000000000000000 ) ) ;
#14039 = VERTEX_POINT ( 'NONE', #36058 ) ;
#14040 = EDGE_CURVE ( 'NONE', #16500, #24955, #24091, .T. ) ;
#14041 = ADVANCED_FACE ( 'NONE', ( #17206 ), #39256, .T. ) ;
#14042 = DIRECTION ( 'NONE',  ( 0.000000000000000000, 0.000000000000000000, -1.000000000000000000 ) ) ;
#14043 = ORIENTED_EDGE ( 'NONE', *, *, #9055, .T. ) ;
#14044 = EDGE_CURVE ( 'NONE', #15799, #3669, #47083, .T. ) ;
#14045 = DIRECTION ( 'NONE',  ( -1.000000000000000000, 0.000000000000000000, 0.000000000000000000 ) ) ;
#14046 = DIRECTION ( 'NONE',  ( -1.000000000000000000, 0.000000000000000000, -0.000000000000000000 ) ) ;
#14047 = ORIENTED_EDGE ( 'NONE', *, *, #45937, .F. ) ;
#14048 = DIRECTION ( 'NONE',  ( 1.000000000000000000, 0.000000000000000000, -0.000000000000000000 ) ) ;
#14049 = ORIENTED_EDGE ( 'NONE', *, *, #9174, .T. ) ;
#14050 = DIRECTION ( 'NONE',  ( 0.000000000000000000, -0.3826834323650772363, -0.9238795325112919565 ) ) ;
#14051 = DIRECTION ( 'NONE',  ( 0.000000000000000000, 0.000000000000000000, -1.000000000000000000 ) ) ;
#14052 = CYLINDRICAL_SURFACE ( 'NONE', #45456, 16.00000000000000000 ) ;
#14053 = EDGE_CURVE ( 'NONE', #36450, #37662, #25224, .T. ) ;
#14054 = VECTOR ( 'NONE', #23230, 1000.000000000000114 ) ;
#14055 = ORIENTED_EDGE ( 'NONE', *, *, #1829, .F. ) ;
#14056 = CIRCLE ( 'NONE', #2346, 37.49900000000001654 ) ;
#14057 = DIRECTION ( 'NONE',  ( -1.000000000000000000, 0.000000000000000000, 0.000000000000000000 ) ) ;
#14058 = ORIENTED_EDGE ( 'NONE', *, *, #28283, .F. ) ;
#14059 = ORIENTED_EDGE ( 'NONE', *, *, #6188, .F. ) ;
#14060 = LINE ( 'NONE', #43681, #41094 ) ;
#14061 = AXIS2_PLACEMENT_3D ( 'NONE', #3800, #14594, #33423 ) ;
#14062 = DIRECTION ( 'NONE',  ( -0.000000000000000000, -0.000000000000000000, 1.000000000000000000 ) ) ;
#14063 = DIRECTION ( 'NONE',  ( -1.000000000000000000, -0.000000000000000000, -0.000000000000000000 ) ) ;
#14064 = CARTESIAN_POINT ( 'NONE',  ( 10.00000000000000000, -0.8261519478436571973, 77.49459641780886443 ) ) ;
#14065 = ORIENTED_EDGE ( 'NONE', *, *, #36734, .T. ) ;
#14066 = CARTESIAN_POINT ( 'NONE',  ( 11.59999999999999964, -0.8299999999999999600, 0.000000000000000000 ) ) ;
#14067 = CARTESIAN_POINT ( 'NONE',  ( 10.00000000000000000, -68.26794271651239399, -31.47745569255214093 ) ) ;
#14068 = MECHANICAL_DESIGN_GEOMETRIC_PRESENTATION_REPRESENTATION (  '', ( #31273 ), #22652 ) ;
#14069 = DIRECTION ( 'NONE',  ( 1.000000000000000000, 0.000000000000000000, 0.000000000000000000 ) ) ;
#14070 = DIRECTION ( 'NONE',  ( -1.000000000000000000, 0.000000000000000000, 0.000000000000000000 ) ) ;
#14071 = DIRECTION ( 'NONE',  ( 0.000000000000000000, 0.000000000000000000, -1.000000000000000000 ) ) ;
#14072 = DIRECTION ( 'NONE',  ( 0.000000000000000000, 0.9945218953682730678, -0.1045284632676570929 ) ) ;
#14073 = VERTEX_POINT ( 'NONE', #47331 ) ;
#14074 = CIRCLE ( 'NONE', #21077, 82.00000000000000000 ) ;
#14075 = ORIENTED_EDGE ( 'NONE', *, *, #5257, .T. ) ;
#14076 = DIRECTION ( 'NONE',  ( -0.000000000000000000, -0.000000000000000000, 1.000000000000000000 ) ) ;
#14077 = DIRECTION ( 'NONE',  ( 0.000000000000000000, -0.07845909572785221553, 0.9969173337331274087 ) ) ;
#14078 = CARTESIAN_POINT ( 'NONE',  ( 11.99999999999999822, 68.55367621811141987, 44.99326035066078333 ) ) ;
#14079 = CARTESIAN_POINT ( 'NONE',  ( 50.00005079999999680, 0.000000000000000000, 12.50000000000000000 ) ) ;
#14080 = CARTESIAN_POINT ( 'NONE',  ( 10.00000000000000000, -16.45098606841149902, 33.79645857604508308 ) ) ;
#14081 = DIRECTION ( 'NONE',  ( -1.000000000000000000, -0.000000000000000000, -0.000000000000000000 ) ) ;
#14082 = ORIENTED_EDGE ( 'NONE', *, *, #8552, .F. ) ;
#14083 = FACE_OUTER_BOUND ( 'NONE', #39569, .T. ) ;
#14084 = EDGE_CURVE ( 'NONE', #48350, #20992, #35337, .T. ) ;
#14085 = EDGE_CURVE ( 'NONE', #10568, #40057, #10120, .T. ) ;
#14086 = DIRECTION ( 'NONE',  ( -1.000000000000000000, 0.000000000000000000, -0.000000000000000000 ) ) ;
#14087 = EDGE_CURVE ( 'NONE', #46808, #45623, #33030, .T. ) ;
#14088 = ORIENTED_EDGE ( 'NONE', *, *, #16762, .T. ) ;
#14089 = ORIENTED_EDGE ( 'NONE', *, *, #44801, .F. ) ;
#14090 = AXIS2_PLACEMENT_3D ( 'NONE', #12374, #5023, #34874 ) ;
#14091 = EDGE_CURVE ( 'NONE', #4178, #43952, #30707, .T. ) ;
#14092 = ORIENTED_EDGE ( 'NONE', *, *, #16713, .F. ) ;
#14093 = AXIS2_PLACEMENT_3D ( 'NONE', #32584, #10302, #40427 ) ;
#14094 = EDGE_CURVE ( 'NONE', #25033, #23062, #16981, .T. ) ;
#14095 = ORIENTED_EDGE ( 'NONE', *, *, #16700, .F. ) ;
#14096 = AXIS2_PLACEMENT_3D ( 'NONE', #27659, #5385, #46510 ) ;
#14097 = DIRECTION ( 'NONE',  ( -1.000000000000000000, 0.000000000000000000, 0.000000000000000000 ) ) ;
#14098 = ORIENTED_EDGE ( 'NONE', *, *, #24875, .T. ) ;
#14099 = VECTOR ( 'NONE', #6254, 1000.000000000000000 ) ;
#14100 = AXIS2_PLACEMENT_3D ( 'NONE', #40988, #41230, #45136 ) ;
#14101 = VERTEX_POINT ( 'NONE', #47788 ) ;
#14102 = CARTESIAN_POINT ( 'NONE',  ( -5.420674214417706693, -142.8662697233533265, -2.500000000000000000 ) ) ;
#14103 = CIRCLE ( 'NONE', #39895, 21.00000000000000000 ) ;
#14104 = EDGE_CURVE ( 'NONE', #19386, #42217, #995, .T. ) ;
#14105 = DIRECTION ( 'NONE',  ( -1.000000000000000000, -0.000000000000000000, -0.000000000000000000 ) ) ;
#14106 = DIRECTION ( 'NONE',  ( 0.000000000000000000, -0.3826834323650970537, 0.9238795325112838519 ) ) ;
#14107 = ORIENTED_EDGE ( 'NONE', *, *, #47145, .T. ) ;
#14108 = CARTESIAN_POINT ( 'NONE',  ( -4.653126046682595884, -146.1313684676804314, 5.500000000000000000 ) ) ;
#14109 = VERTEX_POINT ( 'NONE', #25760 ) ;
#14110 = ORIENTED_EDGE ( 'NONE', *, *, #38053, .F. ) ;
#14111 = ORIENTED_EDGE ( 'NONE', *, *, #15588, .F. ) ;
#14112 = CARTESIAN_POINT ( 'NONE',  ( 2.874421927457452952, -143.3717286177755739, -5.500000000000000000 ) ) ;
#14113 = DIRECTION ( 'NONE',  ( -1.000000000000000000, -0.000000000000000000, 0.000000000000000000 ) ) ;
#14114 = ADVANCED_FACE ( 'NONE', ( #32632 ), #36307, .F. ) ;
#14115 = CARTESIAN_POINT ( 'NONE',  ( 50.00005079999999680, 0.000000000000000000, 0.000000000000000000 ) ) ;
#14116 = ORIENTED_EDGE ( 'NONE', *, *, #21216, .T. ) ;
#14117 = ORIENTED_EDGE ( 'NONE', *, *, #41314, .T. ) ;
#14118 = ORIENTED_EDGE ( 'NONE', *, *, #20046, .T. ) ;
#14119 = CARTESIAN_POINT ( 'NONE',  ( -10.00000000000000000, 0.000000000000000000, 0.000000000000000000 ) ) ;
#14120 = ORIENTED_EDGE ( 'NONE', *, *, #17340, .F. ) ;
#14121 = CARTESIAN_POINT ( 'NONE',  ( 5.204170427930421283E-15, 0.000000000000000000, -12.79999999999999893 ) ) ;
#14122 = CARTESIAN_POINT ( 'NONE',  ( 12.00000000000000000, -22.67460108101774452, 6.353146135318220367 ) ) ;
#14123 = DIRECTION ( 'NONE',  ( -1.000000000000000000, -0.000000000000000000, -0.000000000000000000 ) ) ;
#14124 = VERTEX_POINT ( 'NONE', #36546 ) ;
#14125 = DIRECTION ( 'NONE',  ( -1.000000000000000000, -0.000000000000000000, 0.000000000000000000 ) ) ;
#14126 = FACE_OUTER_BOUND ( 'NONE', #19352, .T. ) ;
#14127 = CARTESIAN_POINT ( 'NONE',  ( 0.000000000000000000, -59.03342792756231461, -46.54456581323868392 ) ) ;
#14128 = CARTESIAN_POINT ( 'NONE',  ( 5.204170427930421283E-15, 1.567547902908612184E-15, 12.79999999999999893 ) ) ;
#14129 = AXIS2_PLACEMENT_3D ( 'NONE', #46864, #20187, #35108 ) ;
#14130 = EDGE_CURVE ( 'NONE', #40856, #47874, #14766, .T. ) ;
#14131 = CARTESIAN_POINT ( 'NONE',  ( 10.00000000000000000, 26.08949754953062694, -27.05870788708203989 ) ) ;
#14132 = ORIENTED_EDGE ( 'NONE', *, *, #11064, .F. ) ;
#14133 = AXIS2_PLACEMENT_3D ( 'NONE', #37892, #26398, #19280 ) ;
#14134 = CYLINDRICAL_SURFACE ( 'NONE', #17861, 32.00000000000000000 ) ;
#14135 = CIRCLE ( 'NONE', #16475, 37.49900000000000944 ) ;
#14136 = AXIS2_PLACEMENT_3D ( 'NONE', #682, #37893, #3374 ) ;
#14137 = LINE ( 'NONE', #10464, #30849 ) ;
#14138 = CARTESIAN_POINT ( 'NONE',  ( 0.000000000000000000, -55.20638768913797634, 51.02545421589302777 ) ) ;
#14139 = DIRECTION ( 'NONE',  ( 0.000000000000000000, 0.000000000000000000, 1.000000000000000000 ) ) ;
#14140 = AXIS2_PLACEMENT_3D ( 'NONE', #19110, #30149, #45071 ) ;
#14141 = DIRECTION ( 'NONE',  ( -1.000000000000000000, 0.000000000000000000, -0.000000000000000000 ) ) ;
#14142 = CIRCLE ( 'NONE', #31346, 77.49899999999999523 ) ;
#14143 = CYLINDRICAL_SURFACE ( 'NONE', #24827, 16.00000000000000000 ) ;
#14144 = EDGE_CURVE ( 'NONE', #10381, #25961, #40476, .T. ) ;
#14145 = LINE ( 'NONE', #30292, #26323 ) ;
#14146 = CARTESIAN_POINT ( 'NONE',  ( -22.53294031248082163, -134.0273518838794757, 5.500000000000000000 ) ) ;
#14147 = CARTESIAN_POINT ( 'NONE',  ( 0.000000000000000000, 73.95703589264006439, -23.16143007188350822 ) ) ;
#14148 = APPLICATION_CONTEXT ( 'automotive_design' ) ;
#14149 = EDGE_CURVE ( 'NONE', #12471, #29523, #29684, .T. ) ;
#14150 = LINE ( 'NONE', #37385, #2642 ) ;
#14151 = EDGE_CURVE ( 'NONE', #15029, #38875, #17405, .T. ) ;
#14152 =( LENGTH_UNIT ( ) NAMED_UNIT ( * ) SI_UNIT ( .MILLI., .METRE. ) );
#14153 = ADVANCED_FACE ( 'NONE', ( #40700 ), #11086, .T. ) ;
#14154 = VERTEX_POINT ( 'NONE', #40953 ) ;
#14155 = VERTEX_POINT ( 'NONE', #44379 ) ;
#14156 = EDGE_CURVE ( 'NONE', #8981, #16167, #1024, .T. ) ;
#14157 = CARTESIAN_POINT ( 'NONE',  ( -10.00000000000000000, 0.000000000000000000, 0.000000000000000000 ) ) ;
#14158 = LINE ( 'NONE', #14650, #15969 ) ;
#14159 = ORIENTED_EDGE ( 'NONE', *, *, #34146, .T. ) ;
#14160 = AXIS2_PLACEMENT_3D ( 'NONE', #535, #5412, #34287 ) ;
#14161 = VECTOR ( 'NONE', #20421, 1000.000000000000000 ) ;
#14162 = DIRECTION ( 'NONE',  ( 0.000000000000000000, 0.7071067811865487940, -0.7071067811865462405 ) ) ;
#14163 = AXIS2_PLACEMENT_3D ( 'NONE', #43564, #10257, #32073 ) ;
#14164 = CIRCLE ( 'NONE', #18866, 82.00000000000000000 ) ;
#14165 = ORIENTED_EDGE ( 'NONE', *, *, #1054, .T. ) ;
#14166 = ORIENTED_EDGE ( 'NONE', *, *, #3364, .T. ) ;
#14167 = ORIENTED_EDGE ( 'NONE', *, *, #7125, .T. ) ;
#14168 = VECTOR ( 'NONE', #24725, 1000.000000000000000 ) ;
#14169 = CARTESIAN_POINT ( 'NONE',  ( 22.94323693612312809, -114.6983135802921083, 5.500000000000000000 ) ) ;
#14170 = VERTEX_POINT ( 'NONE', #37024 ) ;
#14171 = DIRECTION ( 'NONE',  ( 0.000000000000000000, -0.7071067811865389130, -0.7071067811865563435 ) ) ;
#14172 = ORIENTED_EDGE ( 'NONE', *, *, #35172, .T. ) ;
#14173 = LINE ( 'NONE', #2660, #29083 ) ;
#14174 = AXIS2_PLACEMENT_3D ( 'NONE', #46515, #39160, #20543 ) ;
#14175 = FACE_OUTER_BOUND ( 'NONE', #31141, .T. ) ;
#14176 = DIRECTION ( 'NONE',  ( 0.000000000000000000, 0.000000000000000000, 1.000000000000000000 ) ) ;
#14177 = ORIENTED_EDGE ( 'NONE', *, *, #8716, .F. ) ;
#14178 = ORIENTED_EDGE ( 'NONE', *, *, #21619, .T. ) ;
#14179 = CARTESIAN_POINT ( 'NONE',  ( 5.999999999999999112, -59.75363087400035056, -56.15606465355020305 ) ) ;
#14180 = STYLED_ITEM ( 'NONE', ( #20512 ), #3244 ) ;
#14181 = DIRECTION ( 'NONE',  ( 0.000000000000000000, -0.8090169943749426773, 0.5877852522924797984 ) ) ;
#14182 = ORIENTED_EDGE ( 'NONE', *, *, #32861, .T. ) ;
#14183 = EDGE_LOOP ( 'NONE', ( #33052, #5107, #17798, #14118 ) ) ;
#14184 = DIRECTION ( 'NONE',  ( -1.000000000000000000, -0.000000000000000000, -0.000000000000000000 ) ) ;
#14185 = DIRECTION ( 'NONE',  ( -1.000000000000000000, -0.000000000000000000, 0.000000000000000000 ) ) ;
#14186 = ORIENTED_EDGE ( 'NONE', *, *, #40834, .F. ) ;
#14187 = ORIENTED_EDGE ( 'NONE', *, *, #15197, .T. ) ;
#14188 = CARTESIAN_POINT ( 'NONE',  ( 0.000000000000000000, 62.50884508063427347, 41.76106447765511831 ) ) ;
#14189 = CYLINDRICAL_SURFACE ( 'NONE', #23532, 37.49900000000000233 ) ;
#14190 = DIRECTION ( 'NONE',  ( -1.000000000000000000, -0.000000000000000000, -0.000000000000000000 ) ) ;
#14191 = CARTESIAN_POINT ( 'NONE',  ( 10.00000000000000000, 10.96151621346540317, -35.95386929396244113 ) ) ;
#14193 = CIRCLE ( 'NONE', #20440, 37.49900000000000944 ) ;
#14192 = DIRECTION ( 'NONE',  ( -1.000000000000000000, 0.000000000000000000, -0.000000000000000000 ) ) ;
#14194 = ADVANCED_FACE ( 'NONE', ( #40234 ), #26004, .T. ) ;
#14195 = AXIS2_PLACEMENT_3D ( 'NONE', #23087, #19168, #3516 ) ;
#14196 = FACE_OUTER_BOUND ( 'NONE', #2675, .T. ) ;
#14197 = DIRECTION ( 'NONE',  ( -0.000000000000000000, -0.000000000000000000, -1.000000000000000000 ) ) ;
#14198 = EDGE_CURVE ( 'NONE', #18852, #9070, #38570, .T. ) ;
#14199 = AXIS2_PLACEMENT_3D ( 'NONE', #18125, #33066, #36976 ) ;
#14200 = LINE ( 'NONE', #28403, #18190 ) ;
#14201 = CARTESIAN_POINT ( 'NONE',  ( 5.000000000000000000, -59.75363087400035056, -56.15606465355021015 ) ) ;
#14202 = AXIS2_PLACEMENT_3D ( 'NONE', #46160, #5288, #46884 ) ;
#14203 = EDGE_CURVE ( 'NONE', #38112, #894, #3738, .T. ) ;
#14204 = CARTESIAN_POINT ( 'NONE',  ( 0.000000000000000000, 0.000000000000000000, 0.000000000000000000 ) ) ;
#14205 = DIRECTION ( 'NONE',  ( -1.000000000000000000, -0.000000000000000000, 0.000000000000000000 ) ) ;
#14206 = ORIENTED_EDGE ( 'NONE', *, *, #11424, .F. ) ;
#14207 = ORIENTED_EDGE ( 'NONE', *, *, #35521, .F. ) ;
#14208 = EDGE_CURVE ( 'NONE', #14101, #7679, #36776, .T. ) ;
#14209 = ORIENTED_EDGE ( 'NONE', *, *, #20727, .F. ) ;
#14210 = DIRECTION ( 'NONE',  ( -1.000000000000000000, -0.000000000000000000, -0.000000000000000000 ) ) ;
#14211 = ADVANCED_FACE ( 'NONE', ( #33595 ), #56, .F. ) ;
#14212 = AXIS2_PLACEMENT_3D ( 'NONE', #7368, #3194, #32814 ) ;
#14213 = EDGE_CURVE ( 'NONE', #22290, #35782, #20594, .T. ) ;
#14214 = CARTESIAN_POINT ( 'NONE',  ( 0.000000000000000000, -35.53030884539094103, 12.26510123303246935 ) ) ;
#14215 = ORIENTED_EDGE ( 'NONE', *, *, #46299, .F. ) ;
#14216 = ORIENTED_EDGE ( 'NONE', *, *, #32634, .F. ) ;
#14217 = CARTESIAN_POINT ( 'NONE',  ( 10.00000000000000000, 10.74501242461282757, 35.92658777277515014 ) ) ;
#14218 = ORIENTED_EDGE ( 'NONE', *, *, #10017, .T. ) ;
#14219 = CYLINDRICAL_SURFACE ( 'NONE', #10471, 82.00000000000000000 ) ;
#14220 = ORIENTED_EDGE ( 'NONE', *, *, #11006, .T. ) ;
#14221 = DIRECTION ( 'NONE',  ( -0.9580045777625452175, -0.2867529058022035837, 0.000000000000000000 ) ) ;
#14222 = CARTESIAN_POINT ( 'NONE',  ( -7.469491406282094736, 4.756046723998911929, 52.00000000000002132 ) ) ;
#14223 = LINE ( 'NONE', #17883, #2378 ) ;
#14224 = VERTEX_POINT ( 'NONE', #25523 ) ;
#14225 = DIRECTION ( 'NONE',  ( 0.000000000000000000, 0.000000000000000000, 1.000000000000000000 ) ) ;
#14226 = CIRCLE ( 'NONE', #4875, 37.49900000000000233 ) ;
#14227 = ORIENTED_EDGE ( 'NONE', *, *, #29058, .T. ) ;
#14228 = DIRECTION ( 'NONE',  ( 0.000000000000000000, -0.8910065241883626808, -0.4539904997395570740 ) ) ;
#14229 = ORIENTED_EDGE ( 'NONE', *, *, #555, .T. ) ;
#14230 = CYLINDRICAL_SURFACE ( 'NONE', #12666, 42.00000000000000000 ) ;
#14231 = AXIS2_PLACEMENT_3D ( 'NONE', #34643, #30754, #15354 ) ;
#14232 = ORIENTED_EDGE ( 'NONE', *, *, #42891, .F. ) ;
#14233 = CARTESIAN_POINT ( 'NONE',  ( 0.000000000000000000, -68.27212725128254078, -31.46837873495049465 ) ) ;
#14234 = CARTESIAN_POINT ( 'NONE',  ( -21.33958957442910886, -129.9559990355020034, -5.500000000000000000 ) ) ;
#14235 = ADVANCED_FACE ( 'NONE', ( #21367 ), #44134, .F. ) ;
#14236 = DIRECTION ( 'NONE',  ( -1.000000000000000000, -0.000000000000000000, -0.000000000000000000 ) ) ;
#14237 = EDGE_CURVE ( 'NONE', #7731, #34659, #21366, .T. ) ;
#14238 = DIRECTION ( 'NONE',  ( -1.000000000000000000, -0.000000000000000000, 0.000000000000000000 ) ) ;
#14239 = VERTEX_POINT ( 'NONE', #1021 ) ;
#14240 = DIRECTION ( 'NONE',  ( -1.000000000000000000, -0.000000000000000000, 0.000000000000000000 ) ) ;
#14241 = ORIENTED_EDGE ( 'NONE', *, *, #27098, .F. ) ;
#14242 = ORIENTED_EDGE ( 'NONE', *, *, #21251, .F. ) ;
#14243 = DIRECTION ( 'NONE',  ( -1.000000000000000000, -0.000000000000000000, -0.000000000000000000 ) ) ;
#14244 = DIRECTION ( 'NONE',  ( -1.000000000000000000, -0.000000000000000000, 0.000000000000000000 ) ) ;
#14245 = ORIENTED_EDGE ( 'NONE', *, *, #19334, .T. ) ;
#14246 = AXIS2_PLACEMENT_3D ( 'NONE', #45731, #11229, #40841 ) ;
#14247 = EDGE_CURVE ( 'NONE', #5941, #9046, #15722, .T. ) ;
#14248 = DIRECTION ( 'NONE',  ( 0.000000000000000000, -0.9969173337331271867, -0.07845909572785568498 ) ) ;
#14249 = DIRECTION ( 'NONE',  ( 1.000000000000000000, 0.000000000000000000, -0.000000000000000000 ) ) ;
#14250 = CARTESIAN_POINT ( 'NONE',  ( -26.29030328629083968, -123.6496510949466341, 5.500000000000000000 ) ) ;
#14251 = ORIENTED_EDGE ( 'NONE', *, *, #29680, .F. ) ;
#14252 = ADVANCED_FACE ( 'NONE', ( #34544 ), #783, .T. ) ;
#14253 = CARTESIAN_POINT ( 'NONE',  ( 10.00000000000000000, 0.8261519478441983200, -77.49459641780885022 ) ) ;
#14254 = CARTESIAN_POINT ( 'NONE',  ( 11.99999999999999822, -77.32052557432845674, 5.256550761632577284 ) ) ;
#14255 = CARTESIAN_POINT ( 'NONE',  ( -114.1267819554185365, -82.91796067500661138, -5.500000000000000000 ) ) ;
#14256 = VERTEX_POINT ( 'NONE', #19860 ) ;
#14257 = DIRECTION ( 'NONE',  ( 0.000000000000000000, 0.000000000000000000, -1.000000000000000000 ) ) ;
#14258 = CARTESIAN_POINT ( 'NONE',  ( 10.00000000000000000, 0.000000000000000000, 77.49899999999999523 ) ) ;
#14259 = CYLINDRICAL_SURFACE ( 'NONE', #6026, 82.00000000000000000 ) ;
#14260 = CARTESIAN_POINT ( 'NONE',  ( 0.000000000000000000, -35.38097989696503021, -12.42422080174676147 ) ) ;
#14261 = DIRECTION ( 'NONE',  ( -0.000000000000000000, 0.5000000000000039968, -0.8660254037844363761 ) ) ;
#14262 = CARTESIAN_POINT ( 'NONE',  ( -10.00000000000000000, 0.000000000000000000, 0.000000000000000000 ) ) ;
#14263 = DIRECTION ( 'NONE',  ( -1.000000000000000000, -0.000000000000000000, -0.000000000000000000 ) ) ;
#14264 = EDGE_CURVE ( 'NONE', #7751, #1711, #19785, .T. ) ;
#14265 = CYLINDRICAL_SURFACE ( 'NONE', #13939, 82.00000000000000000 ) ;
#14266 = EDGE_CURVE ( 'NONE', #26114, #44403, #40146, .T. ) ;
#14267 = VERTEX_POINT ( 'NONE', #15255 ) ;
#14268 = ADVANCED_FACE ( 'NONE', ( #8137 ), #19381, .T. ) ;
#14269 = CIRCLE ( 'NONE', #11930, 31.99999999999999289 ) ;
#14270 = ORIENTED_EDGE ( 'NONE', *, *, #42992, .F. ) ;
#14271 = DIRECTION ( 'NONE',  ( -1.000000000000000000, 0.000000000000000000, 0.000000000000000000 ) ) ;
#14272 = ORIENTED_EDGE ( 'NONE', *, *, #34875, .F. ) ;
#14273 = CARTESIAN_POINT ( 'NONE',  ( 4.999999999999999112, 21.40280677340371795, 36.13751322684426270 ) ) ;
#14274 = DIRECTION ( 'NONE',  ( 0.000000000000000000, 0.000000000000000000, 1.000000000000000000 ) ) ;
#14275 = CARTESIAN_POINT ( 'NONE',  ( 11.41210121379328335, -99.40233154247455616, 5.500000000000000000 ) ) ;
#14276 = AXIS2_PLACEMENT_3D ( 'NONE', #17189, #12817, #14440 ) ;
#14277 = ORIENTED_EDGE ( 'NONE', *, *, #41080, .T. ) ;
#14278 = EDGE_CURVE ( 'NONE', #38804, #47328, #41715, .T. ) ;
#14279 = VECTOR ( 'NONE', #6020, 1000.000000000000000 ) ;
#14280 = VECTOR ( 'NONE', #6751, 1000.000000000000114 ) ;
#14281 = DIRECTION ( 'NONE',  ( 0.000000000000000000, -0.8090169943749508930, 0.5877852522924683631 ) ) ;
#14282 = ORIENTED_EDGE ( 'NONE', *, *, #4482, .T. ) ;
#14283 = CARTESIAN_POINT ( 'NONE',  ( 12.00000000000000000, -0.9646360437372099028, 23.52805723605590771 ) ) ;
#14284 = ORIENTED_EDGE ( 'NONE', *, *, #34971, .F. ) ;
#14285 = DIRECTION ( 'NONE',  ( -1.000000000000000000, 0.000000000000000000, 0.000000000000000000 ) ) ;
#14286 = DIRECTION ( 'NONE',  ( 0.000000000000000000, 0.000000000000000000, 1.000000000000000000 ) ) ;
#14287 = VERTEX_POINT ( 'NONE', #37510 ) ;
#14288 = CARTESIAN_POINT ( 'NONE',  ( 0.000000000000000000, 17.67226234102874116, -33.17418723428288274 ) ) ;
#14289 = AXIS2_PLACEMENT_3D ( 'NONE', #35278, #2011, #1754 ) ;
#14290 = VERTEX_POINT ( 'NONE', #12070 ) ;
#14291 = CYLINDRICAL_SURFACE ( 'NONE', #11629, 31.99999999999999289 ) ;
#14292 = FACE_BOUND ( 'NONE', #35647, .T. ) ;
#14293 = CYLINDRICAL_SURFACE ( 'NONE', #34478, 82.00000000000000000 ) ;
#14294 = AXIS2_PLACEMENT_3D ( 'NONE', #12053, #8368, #4929 ) ;
#14295 = AXIS2_PLACEMENT_3D ( 'NONE', #26962, #8577, #7859 ) ;
#14296 = ADVANCED_FACE ( 'NONE', ( #12308 ), #34074, .F. ) ;
#14297 = ORIENTED_EDGE ( 'NONE', *, *, #42276, .T. ) ;
#14298 = DIRECTION ( 'NONE',  ( -1.000000000000000000, 0.000000000000000000, 0.000000000000000000 ) ) ;
#14299 = VERTEX_POINT ( 'NONE', #15485 ) ;
#14300 = ORIENTED_EDGE ( 'NONE', *, *, #46052, .T. ) ;
#14301 = DIRECTION ( 'NONE',  ( 0.000000000000000000, 0.000000000000000000, 1.000000000000000000 ) ) ;
#14302 = EDGE_CURVE ( 'NONE', #4753, #17448, #39380, .T. ) ;
#14303 = DIRECTION ( 'NONE',  ( -0.000000000000000000, -0.000000000000000000, -1.000000000000000000 ) ) ;
#14304 = AXIS2_PLACEMENT_3D ( 'NONE', #24178, #35182, #27609 ) ;
#14305 = FACE_OUTER_BOUND ( 'NONE', #18613, .T. ) ;
#14306 = DIRECTION ( 'NONE',  ( -1.000000000000000000, 0.000000000000000000, 0.000000000000000000 ) ) ;
#14307 = EDGE_LOOP ( 'NONE', ( #24996, #36068, #20130, #30734 ) ) ;
#14308 = PLANE ( 'NONE',  #47180 ) ;
#14309 = ADVANCED_FACE ( 'NONE', ( #42147 ), #8379, .T. ) ;
#14310 = CIRCLE ( 'NONE', #4152, 31.99999999999998579 ) ;
#14311 = CARTESIAN_POINT ( 'NONE',  ( 0.000000000000000000, -120.0000000000000000, 102.9091629284897493 ) ) ;
#14312 = DIRECTION ( 'NONE',  ( 0.000000000000000000, 0.9510565162951521989, 0.3090169943749517256 ) ) ;
#14313 = FACE_OUTER_BOUND ( 'NONE', #1747, .T. ) ;
#14314 = CYLINDRICAL_SURFACE ( 'NONE', #9042, 16.00000000000000000 ) ;
#14315 = EDGE_LOOP ( 'NONE', ( #20847, #8853, #46143, #7479 ) ) ;
#14316 = CIRCLE ( 'NONE', #45573, 11.59999999999999964 ) ;
#14317 = FACE_OUTER_BOUND ( 'NONE', #24570, .T. ) ;
#14318 = CYLINDRICAL_SURFACE ( 'NONE', #1725, 31.99999999999999289 ) ;
#14319 = CARTESIAN_POINT ( 'NONE',  ( 0.000000000000000000, 10.41901085202078292, 40.68715046381932865 ) ) ;
#14320 = EDGE_CURVE ( 'NONE', #15723, #44567, #47948, .T. ) ;
#14321 = EDGE_CURVE ( 'NONE', #14957, #17765, #19021, .T. ) ;
#14322 = LINE ( 'NONE', #18221, #12979 ) ;
#14323 = DIRECTION ( 'NONE',  ( 0.000000000000000000, 0.000000000000000000, 1.000000000000000000 ) ) ;
#14324 = DIRECTION ( 'NONE',  ( -1.000000000000000000, 0.000000000000000000, 0.000000000000000000 ) ) ;
#14325 = EDGE_LOOP ( 'NONE', ( #20378, #39933 ) ) ;
#14326 = DIRECTION ( 'NONE',  ( 0.000000000000000000, 0.000000000000000000, 1.000000000000000000 ) ) ;
#14327 = AXIS2_PLACEMENT_3D ( 'NONE', #16927, #21063, #32104 ) ;
#14328 = DIRECTION ( 'NONE',  ( 0.000000000000000000, 0.000000000000000000, 1.000000000000000000 ) ) ;
#14329 = ORIENTED_EDGE ( 'NONE', *, *, #18240, .T. ) ;
#14330 = ORIENTED_EDGE ( 'NONE', *, *, #15794, .T. ) ;
#14331 = AXIS2_PLACEMENT_3D ( 'NONE', #45759, #12237, #8534 ) ;
#14332 = EDGE_CURVE ( 'NONE', #11988, #30740, #38241, .T. ) ;
#14333 = VERTEX_POINT ( 'NONE', #11811 ) ;
#14334 = ORIENTED_EDGE ( 'NONE', *, *, #30781, .F. ) ;
#14335 = VECTOR ( 'NONE', #7513, 1000.000000000000000 ) ;
#14336 = VECTOR ( 'NONE', #7126, 1000.000000000000000 ) ;
#14337 = CIRCLE ( 'NONE', #21384, 16.00000000000000000 ) ;
#14338 = CIRCLE ( 'NONE', #17438, 15.99999999999999822 ) ;
#14339 = CYLINDRICAL_SURFACE ( 'NONE', #43726, 82.00000000000000000 ) ;
#14340 = ORIENTED_EDGE ( 'NONE', *, *, #5937, .F. ) ;
#14341 = VECTOR ( 'NONE', #42496, 1000.000000000000000 ) ;
#14342 = ORIENTED_EDGE ( 'NONE', *, *, #1776, .F. ) ;
#14343 = AXIS2_PLACEMENT_3D ( 'NONE', #27476, #41437, #5205 ) ;
#14344 = DIRECTION ( 'NONE',  ( -1.000000000000000000, -0.000000000000000000, -0.000000000000000000 ) ) ;
#14345 = AXIS2_PLACEMENT_3D ( 'NONE', #11787, #8107, #18403 ) ;
#14346 = CYLINDRICAL_SURFACE ( 'NONE', #27343, 31.99999999999998579 ) ;
#14347 = AXIS2_PLACEMENT_3D ( 'NONE', #37274, #32862, #39989 ) ;
#14349 = ORIENTED_EDGE ( 'NONE', *, *, #16829, .T. ) ;
#14348 = DIRECTION ( 'NONE',  ( -1.000000000000000000, -0.000000000000000000, -0.000000000000000000 ) ) ;
#14350 = ORIENTED_EDGE ( 'NONE', *, *, #16758, .F. ) ;
#14351 = CARTESIAN_POINT ( 'NONE',  ( 10.00000000000000000, 0.000000000000000000, 0.000000000000000000 ) ) ;
#14352 = ORIENTED_EDGE ( 'NONE', *, *, #33644, .T. ) ;
#14353 = ORIENTED_EDGE ( 'NONE', *, *, #26417, .F. ) ;
#14354 = VECTOR ( 'NONE', #30360, 1000.000000000000000 ) ;
#14355 = DIRECTION ( 'NONE',  ( 0.000000000000000000, 0.000000000000000000, 1.000000000000000000 ) ) ;
#14356 = DIRECTION ( 'NONE',  ( 0.000000000000000000, 0.000000000000000000, 1.000000000000000000 ) ) ;
#14357 = CARTESIAN_POINT ( 'NONE',  ( 11.99999999999999822, 0.000000000000000000, 0.000000000000000000 ) ) ;
#14358 = VERTEX_POINT ( 'NONE', #26739 ) ;
#14359 = ORIENTED_EDGE ( 'NONE', *, *, #34114, .F. ) ;
#14360 = CARTESIAN_POINT ( 'NONE',  ( 10.00000000000000000, -37.22597642581161637, 5.202137450156258502 ) ) ;
#14361 = EDGE_LOOP ( 'NONE', ( #47044, #6334, #33842, #6309 ) ) ;
#14362 = CARTESIAN_POINT ( 'NONE',  ( 11.99999999999999822, 0.000000000000000000, 0.000000000000000000 ) ) ;
#14363 = EDGE_CURVE ( 'NONE', #39708, #29904, #16220, .T. ) ;
#14364 = DIRECTION ( 'NONE',  ( -1.000000000000000000, 0.000000000000000000, -0.000000000000000000 ) ) ;
#14365 = FACE_BOUND ( 'NONE', #11487, .T. ) ;
#14366 = ORIENTED_EDGE ( 'NONE', *, *, #26167, .F. ) ;
#14367 = DIRECTION ( 'NONE',  ( -1.000000000000000000, 0.000000000000000000, 0.000000000000000000 ) ) ;
#14368 = DIRECTION ( 'NONE',  ( -1.000000000000000000, 0.000000000000000000, 0.000000000000000000 ) ) ;
#14369 = EDGE_CURVE ( 'NONE', #20061, #8653, #23066, .T. ) ;
#14370 = EDGE_CURVE ( 'NONE', #32554, #42774, #301, .T. ) ;
#14371 = CARTESIAN_POINT ( 'NONE',  ( 0.000000000000000000, 0.000000000000000000, 0.000000000000000000 ) ) ;
#14372 = CIRCLE ( 'NONE', #20612, 77.49899999999999523 ) ;
#14373 = DIRECTION ( 'NONE',  ( 0.000000000000000000, 0.7431448254773862505, 0.6691306063588671194 ) ) ;
#14374 = LINE ( 'NONE', #40799, #34525 ) ;
#14375 = CIRCLE ( 'NONE', #12045, 37.49900000000000233 ) ;
#14376 = ORIENTED_EDGE ( 'NONE', *, *, #16601, .F. ) ;
#14377 = ADVANCED_FACE ( 'NONE', ( #12777 ), #42882, .F. ) ;
#14378 = CARTESIAN_POINT ( 'NONE',  ( 15.00000000000000000, 5.835314593368470248, -22.81335362449854642 ) ) ;
#14379 = AXIS2_PLACEMENT_3D ( 'NONE', #29481, #18207, #33396 ) ;
#14380 = AXIS2_PLACEMENT_3D ( 'NONE', #143, #1115, #15811 ) ;
#14381 = VECTOR ( 'NONE', #12355, 1000.000000000000000 ) ;
#14382 = CARTESIAN_POINT ( 'NONE',  ( 11.99999999999999822, 74.65491531819118620, -8.830959090342659579 ) ) ;
#14383 = DIRECTION ( 'NONE',  ( -1.000000000000000000, 0.000000000000000000, -0.000000000000000000 ) ) ;
#14384 = CARTESIAN_POINT ( 'NONE',  ( -10.00000000000000000, 0.000000000000000000, 0.000000000000000000 ) ) ;
#14385 = EDGE_CURVE ( 'NONE', #15224, #7609, #27638, .T. ) ;
#14386 = DIRECTION ( 'NONE',  ( -1.000000000000000000, 0.000000000000000000, 0.000000000000000000 ) ) ;
#14387 = CARTESIAN_POINT ( 'NONE',  ( 12.00000000000000000, 20.85821328998741109, -10.92862929874522671 ) ) ;
#14388 = AXIS2_PLACEMENT_3D ( 'NONE', #37462, #11033, #45960 ) ;
#14389 = CIRCLE ( 'NONE', #47977, 82.00000000000000000 ) ;
#14390 = LINE ( 'NONE', #18287, #18489 ) ;
#14391 = CARTESIAN_POINT ( 'NONE',  ( 0.000000000000000000, 0.000000000000000000, 0.000000000000000000 ) ) ;
#14392 = EDGE_CURVE ( 'NONE', #36067, #12155, #23714, .T. ) ;
#14393 = AXIS2_PLACEMENT_3D ( 'NONE', #22025, #17870, #44313 ) ;
#14394 = DIRECTION ( 'NONE',  ( 0.000000000000000000, 0.000000000000000000, 1.000000000000000000 ) ) ;
#14395 = DIRECTION ( 'NONE',  ( -1.000000000000000000, 0.000000000000000000, 0.000000000000000000 ) ) ;
#14396 = VECTOR ( 'NONE', #43376, 1000.000000000000000 ) ;
#14397 = EDGE_LOOP ( 'NONE', ( #19749, #42831, #44348, #25186 ) ) ;
#14398 = ORIENTED_EDGE ( 'NONE', *, *, #27290, .T. ) ;
#14399 = ORIENTED_EDGE ( 'NONE', *, *, #17456, .T. ) ;
#14400 = EDGE_CURVE ( 'NONE', #18807, #39592, #39329, .T. ) ;
#14401 = DIRECTION ( 'NONE',  ( -1.000000000000000000, 0.000000000000000000, 0.000000000000000000 ) ) ;
#14402 = DIRECTION ( 'NONE',  ( 0.000000000000000000, 0.8090169943749486725, -0.5877852522924713607 ) ) ;
#14403 = ORIENTED_EDGE ( 'NONE', *, *, #39262, .F. ) ;
#14404 = VERTEX_POINT ( 'NONE', #17152 ) ;
#14405 = EDGE_CURVE ( 'NONE', #26988, #30390, #28422, .T. ) ;
#14406 = CIRCLE ( 'NONE', #30059, 31.99999999999998579 ) ;
#14407 = DIRECTION ( 'NONE',  ( -1.000000000000000000, -0.000000000000000000, 0.000000000000000000 ) ) ;
#14408 = CIRCLE ( 'NONE', #36274, 77.49899999999999523 ) ;
#14409 = EDGE_LOOP ( 'NONE', ( #6690, #34277, #23572, #44193 ) ) ;
#14410 = AXIS2_PLACEMENT_3D ( 'NONE', #45345, #11364, #4006 ) ;
#14411 = PRODUCT_DEFINITION_SHAPE ( 'NONE', 'NONE',  #48456 ) ;
#14412 = CARTESIAN_POINT ( 'NONE',  ( 11.99999999999999822, -69.42325613327466272, 34.44570377933573724 ) ) ;
#14413 = VECTOR ( 'NONE', #16672, 999.9999999999998863 ) ;
#14414 = ORIENTED_EDGE ( 'NONE', *, *, #28127, .T. ) ;
#14415 = DIRECTION ( 'NONE',  ( 1.000000000000000000, -0.000000000000000000, -0.000000000000000000 ) ) ;
#14416 = VERTEX_POINT ( 'NONE', #35769 ) ;
#14417 = AXIS2_PLACEMENT_3D ( 'NONE', #2166, #28819, #17081 ) ;
#14418 = EDGE_CURVE ( 'NONE', #4565, #33667, #10429, .T. ) ;
#14419 = CARTESIAN_POINT ( 'NONE',  ( 5.000000000000002665, 79.10210256391398786, -21.60688246758503084 ) ) ;
#14420 = VECTOR ( 'NONE', #36659, 1000.000000000000000 ) ;
#14421 = EDGE_CURVE ( 'NONE', #38747, #22486, #4947, .T. ) ;
#14422 = CARTESIAN_POINT ( 'NONE',  ( 0.000000000000000000, -68.55367621811174672, 44.99326035066030727 ) ) ;
#14423 = CARTESIAN_POINT ( 'NONE',  ( 6.509281303079589520, -14.89695620656361008, 0.000000000000000000 ) ) ;
#14425 = VERTEX_POINT ( 'NONE', #23788 ) ;
#14424 = AXIS2_PLACEMENT_3D ( 'NONE', #42016, #31739, #27086 ) ;
#14426 = EDGE_CURVE ( 'NONE', #27843, #26622, #31638, .T. ) ;
#14427 = VERTEX_POINT ( 'NONE', #31882 ) ;
#14428 = CARTESIAN_POINT ( 'NONE',  ( 0.000000000000000000, 14.60985201121729737, -18.46759930825687945 ) ) ;
#14429 = DIRECTION ( 'NONE',  ( 0.000000000000000000, -0.9969173337331287410, 0.07845909572783495156 ) ) ;
#14430 = ORIENTED_EDGE ( 'NONE', *, *, #33524, .F. ) ;
#14431 = EDGE_LOOP ( 'NONE', ( #2561, #37899, #6640, #24783 ) ) ;
#14432 = EDGE_CURVE ( 'NONE', #20645, #18777, #29199, .T. ) ;
#14433 = DIRECTION ( 'NONE',  ( -1.000000000000000000, 0.000000000000000000, 0.000000000000000000 ) ) ;
#14434 = DIRECTION ( 'NONE',  ( -1.000000000000000000, -0.000000000000000000, -0.000000000000000000 ) ) ;
#14435 = ORIENTED_EDGE ( 'NONE', *, *, #5634, .T. ) ;
#14436 = VERTEX_POINT ( 'NONE', #13490 ) ;
#14437 = CARTESIAN_POINT ( 'NONE',  ( 0.000000000000000000, -6.903761155837252694, -77.19088730480530103 ) ) ;
#14438 = LINE ( 'NONE', #8525, #2105 ) ;
#14439 = DIRECTION ( 'NONE',  ( -1.000000000000000000, 0.000000000000000000, 0.000000000000000000 ) ) ;
#14440 = DIRECTION ( 'NONE',  ( 0.000000000000000000, -0.9723699203976789995, 0.2334453638558956212 ) ) ;
#14441 = DIRECTION ( 'NONE',  ( 1.000000000000000000, 0.000000000000000000, 0.000000000000000000 ) ) ;
#14442 = CARTESIAN_POINT ( 'NONE',  ( 10.00000000000000000, 0.000000000000000000, 0.000000000000000000 ) ) ;
#14443 = AXIS2_PLACEMENT_3D ( 'NONE', #17309, #24905, #39847 ) ;
#14444 = LINE ( 'NONE', #36225, #37209 ) ;
#14445 = CARTESIAN_POINT ( 'NONE',  ( 0.000000000000000000, -27.75498641678764855, 31.52238457039590358 ) ) ;
#14446 = VERTEX_POINT ( 'NONE', #20116 ) ;
#14447 = VECTOR ( 'NONE', #27296, 1000.000000000000000 ) ;
#14448 = AXIS2_PLACEMENT_3D ( 'NONE', #1014, #29921, #22818 ) ;
#14449 = CARTESIAN_POINT ( 'NONE',  ( 0.000000000000000000, 0.000000000000000000, 0.000000000000000000 ) ) ;
#14450 = DIRECTION ( 'NONE',  ( -1.000000000000000000, 0.000000000000000000, 0.000000000000000000 ) ) ;
#14451 = DIRECTION ( 'NONE',  ( -0.000000000000000000, -0.000000000000000000, -1.000000000000000000 ) ) ;
#14452 = ORIENTED_EDGE ( 'NONE', *, *, #12767, .T. ) ;
#14453 = ORIENTED_EDGE ( 'NONE', *, *, #18827, .F. ) ;
#14454 = ORIENTED_EDGE ( 'NONE', *, *, #29735, .T. ) ;
#14455 = VECTOR ( 'NONE', #33603, 1000.000000000000000 ) ;
#14456 = AXIS2_PLACEMENT_3D ( 'NONE', #29734, #3550, #18710 ) ;
#14457 = UNCERTAINTY_MEASURE_WITH_UNIT (LENGTH_MEASURE( 1.000000000000000082E-05 ), #13192, 'distance_accuracy_value', 'NONE');
#14458 = AXIS2_PLACEMENT_3D ( 'NONE', #11915, #11674, #26838 ) ;
#14459 = DIRECTION ( 'NONE',  ( -1.000000000000000000, 0.000000000000000000, -0.000000000000000000 ) ) ;
#14460 = AXIS2_PLACEMENT_3D ( 'NONE', #29162, #25726, #44581 ) ;
#14461 = CARTESIAN_POINT ( 'NONE',  ( -25.50183398199384754, -112.6408924756582053, -5.500000000000000000 ) ) ;
#14462 = AXIS2_PLACEMENT_3D ( 'NONE', #34896, #16305, #8952 ) ;
#14463 = ORIENTED_EDGE ( 'NONE', *, *, #38472, .T. ) ;
#14464 = EDGE_CURVE ( 'NONE', #1147, #19053, #24484, .T. ) ;
#14465 = DIRECTION ( 'NONE',  ( -1.000000000000000000, -0.000000000000000000, 0.000000000000000000 ) ) ;
#14466 = ORIENTED_EDGE ( 'NONE', *, *, #28280, .T. ) ;
#14467 = LINE ( 'NONE', #40890, #33108 ) ;
#14468 = ORIENTED_EDGE ( 'NONE', *, *, #26594, .F. ) ;
#14469 = AXIS2_PLACEMENT_3D ( 'NONE', #23234, #27900, #9267 ) ;
#14470 = ORIENTED_EDGE ( 'NONE', *, *, #7529, .F. ) ;
#14471 = FACE_OUTER_BOUND ( 'NONE', #375, .T. ) ;
#14472 = VECTOR ( 'NONE', #12110, 1000.000000000000000 ) ;
#14473 = CARTESIAN_POINT ( 'NONE',  ( -16.06301359042743115, -102.7814171781257357, 5.500000000000000000 ) ) ;
#14474 = ORIENTED_EDGE ( 'NONE', *, *, #2960, .T. ) ;
#14475 = EDGE_CURVE ( 'NONE', #34767, #9901, #8087, .T. ) ;
#14476 = CIRCLE ( 'NONE', #12915, 37.49900000000000944 ) ;
#14477 = DIRECTION ( 'NONE',  ( 0.000000000000000000, 0.000000000000000000, 1.000000000000000000 ) ) ;
#14478 = ORIENTED_EDGE ( 'NONE', *, *, #19317, .T. ) ;
#14479 = DIRECTION ( 'NONE',  ( 0.000000000000000000, 0.000000000000000000, 1.000000000000000000 ) ) ;
#14480 = EDGE_CURVE ( 'NONE', #3370, #16986, #6157, .T. ) ;
#14481 = CARTESIAN_POINT ( 'NONE',  ( 0.000000000000000000, -18.13022148937243472, -15.02647892043568767 ) ) ;
#14482 = ORIENTED_EDGE ( 'NONE', *, *, #43818, .T. ) ;
#14483 = DIRECTION ( 'NONE',  ( -1.000000000000000000, -0.000000000000000000, -0.000000000000000000 ) ) ;
#14484 = CYLINDRICAL_SURFACE ( 'NONE', #13785, 31.99999999999998579 ) ;
#14486 = EDGE_LOOP ( 'NONE', ( #27283, #11310, #10698, #3859 ) ) ;
#14485 = CARTESIAN_POINT ( 'NONE',  ( 10.00000000000000000, -17.80606268964563554, 33.00180498840040855 ) ) ;
#14487 = DIRECTION ( 'NONE',  ( 0.000000000000000000, 0.000000000000000000, 1.000000000000000000 ) ) ;
#14488 = CIRCLE ( 'NONE', #5869, 12.49999999999999645 ) ;
#14489 = CIRCLE ( 'NONE', #41858, 16.00000000000000000 ) ;
#14490 = VERTEX_POINT ( 'NONE', #27961 ) ;
#14491 = DIRECTION ( 'NONE',  ( 0.000000000000000000, -0.8910065241883722287, 0.4539904997395383113 ) ) ;
#14492 = ORIENTED_EDGE ( 'NONE', *, *, #12348, .T. ) ;
#14493 = VERTEX_POINT ( 'NONE', #31394 ) ;
#14494 = ADVANCED_FACE ( 'NONE', ( #43116 ), #9335, .T. ) ;
#14495 = DIRECTION ( 'NONE',  ( -1.000000000000000000, -0.000000000000000000, -0.000000000000000000 ) ) ;
#14496 = DIRECTION ( 'NONE',  ( -1.000000000000000000, -0.000000000000000000, -0.000000000000000000 ) ) ;
#14497 = ORIENTED_EDGE ( 'NONE', *, *, #40543, .T. ) ;
#14498 = CYLINDRICAL_SURFACE ( 'NONE', #22197, 77.49899999999999523 ) ;
#14499 = AXIS2_PLACEMENT_3D ( 'NONE', #29593, #22259, #25665 ) ;
#14500 = EDGE_CURVE ( 'NONE', #39232, #20737, #40905, .T. ) ;
#14501 = DIRECTION ( 'NONE',  ( 0.000000000000000000, 0.07845909572783790753, 0.9969173337331285190 ) ) ;
#14502 = DIRECTION ( 'NONE',  ( 0.000000000000000000, 0.000000000000000000, -1.000000000000000000 ) ) ;
#14503 = ORIENTED_EDGE ( 'NONE', *, *, #9176, .T. ) ;
#14504 = FACE_OUTER_BOUND ( 'NONE', #29345, .T. ) ;
#14505 = VECTOR ( 'NONE', #13702, 1000.000000000000000 ) ;
#14506 = FACE_OUTER_BOUND ( 'NONE', #32158, .T. ) ;
#14507 = DIRECTION ( 'NONE',  ( -1.000000000000000000, 0.000000000000000000, -0.000000000000000000 ) ) ;
#14508 = ORIENTED_EDGE ( 'NONE', *, *, #37693, .T. ) ;
#14509 = FACE_OUTER_BOUND ( 'NONE', #39628, .T. ) ;
#14510 = DIRECTION ( 'NONE',  ( -0.08130631524010117905, 0.9966891607226784355, 0.000000000000000000 ) ) ;
#14511 = CARTESIAN_POINT ( 'NONE',  ( 10.00000000000000000, 27.13269053701096922, 25.88420570971410228 ) ) ;
#14512 = DIRECTION ( 'NONE',  ( -1.000000000000000000, 0.000000000000000000, -0.000000000000000000 ) ) ;
#14513 = AXIS2_PLACEMENT_3D ( 'NONE', #28829, #36168, #21235 ) ;
#14514 = DIRECTION ( 'NONE',  ( -1.000000000000000000, -0.000000000000000000, 0.000000000000000000 ) ) ;
#14515 = DIRECTION ( 'NONE',  ( 0.000000000000000000, 0.000000000000000000, 1.000000000000000000 ) ) ;
#14516 = PLANE ( 'NONE',  #43627 ) ;
#14517 = DIRECTION ( 'NONE',  ( 0.000000000000000000, 0.000000000000000000, 1.000000000000000000 ) ) ;
#14518 = ORIENTED_EDGE ( 'NONE', *, *, #4151, .T. ) ;
#14519 = EDGE_CURVE ( 'NONE', #47251, #1792, #17386, .T. ) ;
#14520 = ORIENTED_EDGE ( 'NONE', *, *, #13496, .F. ) ;
#14521 = AXIS2_PLACEMENT_3D ( 'NONE', #13474, #9318, #27694 ) ;
#14522 = CARTESIAN_POINT ( 'NONE',  ( 0.000000000000000000, 62.50329211542435104, 41.76937507738811917 ) ) ;
#14523 = ORIENTED_EDGE ( 'NONE', *, *, #3242, .F. ) ;
#14524 = DIRECTION ( 'NONE',  ( 0.000000000000000000, 0.000000000000000000, -1.000000000000000000 ) ) ;
#14525 = CARTESIAN_POINT ( 'NONE',  ( -120.0000000000000000, -119.9999999999999858, 36.50000000000000711 ) ) ;
#14526 = DIRECTION ( 'NONE',  ( 0.1736481776669309418, 0.9848077530122080203, -0.000000000000000000 ) ) ;
#14527 = EDGE_LOOP ( 'NONE', ( #6876, #6107, #23873, #21487 ) ) ;
#14528 = EDGE_CURVE ( 'NONE', #48218, #48350, #3396, .T. ) ;
#14529 = AXIS2_PLACEMENT_3D ( 'NONE', #40593, #14661, #6830 ) ;
#14530 = EDGE_CURVE ( 'NONE', #27089, #11938, #43293, .T. ) ;
#14531 = CARTESIAN_POINT ( 'NONE',  ( 0.000000000000000000, 75.11764819372149304, -2.946379043146603482 ) ) ;
#14532 = VECTOR ( 'NONE', #5775, 1000.000000000000000 ) ;
#14533 = ORIENTED_EDGE ( 'NONE', *, *, #13064, .T. ) ;
#14534 = EDGE_LOOP ( 'NONE', ( #41659, #28841, #12368, #4058 ) ) ;
#14535 = EDGE_CURVE ( 'NONE', #26532, #31490, #42391, .T. ) ;
#14536 = VECTOR ( 'NONE', #15999, 1000.000000000000000 ) ;
#14537 = DIRECTION ( 'NONE',  ( -1.000000000000000000, 0.000000000000000000, 0.000000000000000000 ) ) ;
#14538 = VECTOR ( 'NONE', #37327, 1000.000000000000000 ) ;
#14539 = DIRECTION ( 'NONE',  ( 0.000000000000000000, 0.000000000000000000, 1.000000000000000000 ) ) ;
#14540 = DIRECTION ( 'NONE',  ( 0.5687579148473752566, -0.8225049752423786442, 0.000000000000000000 ) ) ;
#14541 = ORIENTED_EDGE ( 'NONE', *, *, #18381, .T. ) ;
#14542 = LINE ( 'NONE', #40006, #30151 ) ;
#14543 = VECTOR ( 'NONE', #5754, 1000.000000000000000 ) ;
#14544 = EDGE_LOOP ( 'NONE', ( #1965, #34852, #35760, #38429 ) ) ;
#14545 = ADVANCED_FACE ( 'NONE', ( #40412 ), #40168, .T. ) ;
#14546 = VECTOR ( 'NONE', #44424, 1000.000000000000000 ) ;
#14547 = ORIENTED_EDGE ( 'NONE', *, *, #32647, .T. ) ;
#14548 = ORIENTED_EDGE ( 'NONE', *, *, #1708, .F. ) ;
#14549 = EDGE_CURVE ( 'NONE', #8400, #12094, #3676, .T. ) ;
#14550 = EDGE_CURVE ( 'NONE', #38166, #44442, #18108, .T. ) ;
#14551 = DIRECTION ( 'NONE',  ( 0.000000000000000000, 0.000000000000000000, 1.000000000000000000 ) ) ;
#14552 = DIRECTION ( 'NONE',  ( -1.000000000000000000, -0.000000000000000000, -0.000000000000000000 ) ) ;
#14553 = DIRECTION ( 'NONE',  ( -1.000000000000000000, 0.000000000000000000, -0.000000000000000000 ) ) ;
#14554 = CYLINDRICAL_SURFACE ( 'NONE', #36700, 37.49900000000000233 ) ;
#14555 = VERTEX_POINT ( 'NONE', #6632 ) ;
#14556 = DIRECTION ( 'NONE',  ( 0.000000000000000000, 0.2334453638558989796, 0.9723699203976782224 ) ) ;
#14557 = ORIENTED_EDGE ( 'NONE', *, *, #40876, .F. ) ;
#14558 = ORIENTED_EDGE ( 'NONE', *, *, #29185, .F. ) ;
#14559 = CARTESIAN_POINT ( 'NONE',  ( 0.000000000000000000, -36.73666225445940370, 65.58780272294062286 ) ) ;
#14560 = CARTESIAN_POINT ( 'NONE',  ( -1.250000000000002442, -12.36245420541525242, -1.199999999999999956 ) ) ;
#14561 = ADVANCED_FACE ( 'NONE', ( #40881 ), #29129, .T. ) ;
#14562 = DIRECTION ( 'NONE',  ( 0.000000000000000000, 0.6494480483301849905, -0.7604059656000299317 ) ) ;
#14563 = CARTESIAN_POINT ( 'NONE',  ( 11.99999999999999822, -71.21200624218823805, 40.65526001592589722 ) ) ;
#14564 = VERTEX_POINT ( 'NONE', #32574 ) ;
#14565 = LINE ( 'NONE', #29713, #33889 ) ;
#14566 = CYLINDRICAL_SURFACE ( 'NONE', #22899, 37.49900000000000233 ) ;
#14567 = CARTESIAN_POINT ( 'NONE',  ( -3.000000000000000000, 22.07842321921492612, -8.187992925817130896 ) ) ;
#14568 = CARTESIAN_POINT ( 'NONE',  ( 0.000000000000000000, -39.47590169984898267, 71.87247863392400404 ) ) ;
#14569 = CARTESIAN_POINT ( 'NONE',  ( 0.000000000000000000, 0.000000000000000000, 0.000000000000000000 ) ) ;
#14570 = CIRCLE ( 'NONE', #41932, 16.00000000000000000 ) ;
#14571 = ORIENTED_EDGE ( 'NONE', *, *, #36714, .F. ) ;
#14572 = CARTESIAN_POINT ( 'NONE',  ( 12.00000000000000000, -23.29833615347104470, 3.418703333116808629 ) ) ;
#14573 = DIRECTION ( 'NONE',  ( -1.000000000000000000, 0.000000000000000000, 0.000000000000000000 ) ) ;
#14574 = EDGE_CURVE ( 'NONE', #44487, #30240, #47973, .T. ) ;
#14575 = VECTOR ( 'NONE', #3222, 1000.000000000000000 ) ;
#14576 = DIRECTION ( 'NONE',  ( -1.000000000000000000, -0.000000000000000000, 0.000000000000000000 ) ) ;
#14577 = DIRECTION ( 'NONE',  ( -1.000000000000000000, -0.000000000000000000, 0.000000000000000000 ) ) ;
#14578 = DIRECTION ( 'NONE',  ( -0.7585478161175723821, -0.6516173805718057377, 0.000000000000000000 ) ) ;
#14579 = CYLINDRICAL_SURFACE ( 'NONE', #45115, 32.00000000000000000 ) ;
#14580 = CYLINDRICAL_SURFACE ( 'NONE', #23772, 77.49899999999999523 ) ;
#14581 = CIRCLE ( 'NONE', #39604, 77.49899999999999523 ) ;
#14582 = ORIENTED_EDGE ( 'NONE', *, *, #4386, .T. ) ;
#14583 = DIRECTION ( 'NONE',  ( -0.8774505977381978905, -0.4796670183876304283, 0.000000000000000000 ) ) ;
#14584 = VECTOR ( 'NONE', #10834, 1000.000000000000000 ) ;
#14585 = VECTOR ( 'NONE', #29154, 1000.000000000000000 ) ;
#14586 = DIRECTION ( 'NONE',  ( 0.000000000000000000, 0.000000000000000000, 1.000000000000000000 ) ) ;
#14587 = VERTEX_POINT ( 'NONE', #39926 ) ;
#14588 = VERTEX_POINT ( 'NONE', #2946 ) ;
#14589 = ADVANCED_FACE ( 'NONE', ( #28669 ), #36711, .T. ) ;
#14590 = CIRCLE ( 'NONE', #5969, 77.49899999999999523 ) ;
#14591 = EDGE_CURVE ( 'NONE', #24320, #28070, #36948, .T. ) ;
#14592 = EDGE_CURVE ( 'NONE', #37265, #962, #22169, .T. ) ;
#14593 = VERTEX_POINT ( 'NONE', #14461 ) ;
#14594 = DIRECTION ( 'NONE',  ( -1.000000000000000000, -0.000000000000000000, 0.000000000000000000 ) ) ;
#14595 = VERTEX_POINT ( 'NONE', #18362 ) ;
#14596 = EDGE_CURVE ( 'NONE', #43657, #39094, #10787, .T. ) ;
#14597 = ORIENTED_EDGE ( 'NONE', *, *, #24819, .T. ) ;
#14598 = CIRCLE ( 'NONE', #20848, 77.49899999999999523 ) ;
#14599 = CARTESIAN_POINT ( 'NONE',  ( 12.00000000000000000, 5.835314593368777558, 22.81335362449846471 ) ) ;
#14600 = CYLINDRICAL_SURFACE ( 'NONE', #25755, 32.00000000000000000 ) ;
#14601 = DIRECTION ( 'NONE',  ( -1.000000000000000000, -0.000000000000000000, 0.000000000000000000 ) ) ;
#14602 = ORIENTED_EDGE ( 'NONE', *, *, #44353, .T. ) ;
#14603 = AXIS2_PLACEMENT_3D ( 'NONE', #38460, #31373, #38719 ) ;
#14604 = CARTESIAN_POINT ( 'NONE',  ( 0.000000000000000000, 28.89263327155850192, -71.91182617369156560 ) ) ;
#14605 = ORIENTED_EDGE ( 'NONE', *, *, #38698, .T. ) ;
#14606 = ORIENTED_EDGE ( 'NONE', *, *, #8602, .T. ) ;
#14607 = ORIENTED_EDGE ( 'NONE', *, *, #37157, .F. ) ;
#14608 = EDGE_CURVE ( 'NONE', #1470, #42776, #25939, .T. ) ;
#14609 = EDGE_CURVE ( 'NONE', #39158, #37621, #31595, .T. ) ;
#14610 = LINE ( 'NONE', #6529, #2984 ) ;
#14611 = LINE ( 'NONE', #10922, #35221 ) ;
#14612 = DIRECTION ( 'NONE',  ( 0.000000000000000000, 0.5877852522924780221, 0.8090169943749438985 ) ) ;
#14613 = ORIENTED_EDGE ( 'NONE', *, *, #35588, .T. ) ;
#14614 = AXIS2_PLACEMENT_3D ( 'NONE', #17080, #39622, #6084 ) ;
#14615 = ORIENTED_EDGE ( 'NONE', *, *, #15612, .T. ) ;
#14616 = DIRECTION ( 'NONE',  ( -0.4796670183876317051, 0.8774505977381971134, 0.000000000000000000 ) ) ;
#14617 = VERTEX_POINT ( 'NONE', #33294 ) ;
#14618 = CARTESIAN_POINT ( 'NONE',  ( 11.99999999999999822, -74.74816331893454446, 33.71516098798715433 ) ) ;
#14619 = FACE_OUTER_BOUND ( 'NONE', #31455, .T. ) ;
#14620 = CARTESIAN_POINT ( 'NONE',  ( 0.000000000000000000, 14.60985201121704513, 18.46759930825707841 ) ) ;
#14621 = DIRECTION ( 'NONE',  ( -1.000000000000000000, 0.000000000000000000, 0.000000000000000000 ) ) ;
#14622 = DIRECTION ( 'NONE',  ( 1.000000000000000000, 0.000000000000000000, -0.000000000000000000 ) ) ;
#14623 = DIRECTION ( 'NONE',  ( -0.2306669878475637314, -0.9730327541852493711, 0.000000000000000000 ) ) ;
#14624 = DIRECTION ( 'NONE',  ( -1.000000000000000000, -0.000000000000000000, 0.000000000000000000 ) ) ;
#14626 = EDGE_CURVE ( 'NONE', #6523, #39094, #46433, .T. ) ;
#14625 = CARTESIAN_POINT ( 'NONE',  ( 10.00000000000000000, 46.21855187248629449, 62.20884554314036308 ) ) ;
#14627 = AXIS2_PLACEMENT_3D ( 'NONE', #9500, #21958, #25147 ) ;
#14628 = DIRECTION ( 'NONE',  ( 1.000000000000000000, -0.000000000000000000, 0.000000000000000000 ) ) ;
#14629 = VERTEX_POINT ( 'NONE', #44546 ) ;
#14630 = PLANE ( 'NONE',  #21777 ) ;
#14631 = ORIENTED_EDGE ( 'NONE', *, *, #27827, .T. ) ;
#14632 = DIRECTION ( 'NONE',  ( -1.000000000000000000, 0.000000000000000000, -0.000000000000000000 ) ) ;
#14633 = ORIENTED_EDGE ( 'NONE', *, *, #29606, .T. ) ;
#14634 = CARTESIAN_POINT ( 'NONE',  ( 0.000000000000000000, -65.64334221924939072, 41.19522573413710376 ) ) ;
#14635 = DIRECTION ( 'NONE',  ( 1.000000000000000000, 0.000000000000000000, -0.000000000000000000 ) ) ;
#14636 = CARTESIAN_POINT ( 'NONE',  ( 0.000000000000000000, -12.93880638057260590, -76.41127070299285151 ) ) ;
#14637 = DIRECTION ( 'NONE',  ( 0.000000000000000000, -0.8090169943749403458, -0.5877852522924830181 ) ) ;
#14638 = AXIS2_PLACEMENT_3D ( 'NONE', #28752, #13105, #2092 ) ;
#14639 = CARTESIAN_POINT ( 'NONE',  ( -12.50000000000000000, -132.5000000000000000, 40.00000000000000000 ) ) ;
#14640 = PLANE ( 'NONE',  #2655 ) ;
#14641 = CIRCLE ( 'NONE', #6808, 37.49900000000000233 ) ;
#14642 = CARTESIAN_POINT ( 'NONE',  ( 10.00000000000000000, -37.16516213103273714, -4.992566952385376844 ) ) ;
#14643 = DIRECTION ( 'NONE',  ( -1.000000000000000000, -0.000000000000000000, -0.000000000000000000 ) ) ;
#14644 = EDGE_LOOP ( 'NONE', ( #37480, #15840, #3889, #17039 ) ) ;
#14645 = ORIENTED_EDGE ( 'NONE', *, *, #1047, .F. ) ;
#14646 = AXIS2_PLACEMENT_3D ( 'NONE', #32844, #44119, #2993 ) ;
#14647 = VERTEX_POINT ( 'NONE', #11022 ) ;
#14648 = EDGE_CURVE ( 'NONE', #42467, #25752, #25206, .T. ) ;
#14649 = FACE_OUTER_BOUND ( 'NONE', #4069, .T. ) ;
#14650 = CARTESIAN_POINT ( 'NONE',  ( 22.51310757741980240, -113.2613067136482101, 2.500000000000000000 ) ) ;
#14651 = ORIENTED_EDGE ( 'NONE', *, *, #15917, .F. ) ;
#14652 = ORIENTED_EDGE ( 'NONE', *, *, #38698, .F. ) ;
#14653 = EDGE_CURVE ( 'NONE', #37233, #30791, #26902, .T. ) ;
#14654 = DIRECTION ( 'NONE',  ( -1.000000000000000000, -0.000000000000000000, 0.000000000000000000 ) ) ;
#14655 = VERTEX_POINT ( 'NONE', #17640 ) ;
#14656 = ORIENTED_EDGE ( 'NONE', *, *, #44544, .T. ) ;
#14657 = EDGE_CURVE ( 'NONE', #22595, #9308, #21302, .T. ) ;
#14658 = EDGE_CURVE ( 'NONE', #46491, #11716, #37823, .T. ) ;
#14659 = AXIS2_PLACEMENT_3D ( 'NONE', #40918, #21816, #10580 ) ;
#14660 = PLANE ( 'NONE',  #30549 ) ;
#14661 = DIRECTION ( 'NONE',  ( -1.000000000000000000, 0.000000000000000000, 0.000000000000000000 ) ) ;
#14662 = ADVANCED_FACE ( 'NONE', ( #41863 ), #30588, .T. ) ;
#14663 = ORIENTED_EDGE ( 'NONE', *, *, #32715, .F. ) ;
#14664 = VERTEX_POINT ( 'NONE', #18831 ) ;
#14665 = DIRECTION ( 'NONE',  ( 0.000000000000000000, 0.000000000000000000, -1.000000000000000000 ) ) ;
#14666 = AXIS2_PLACEMENT_3D ( 'NONE', #45689, #8711, #45214 ) ;
#14667 = DIRECTION ( 'NONE',  ( 0.000000000000000000, -0.7071067811865536790, 0.7071067811865414665 ) ) ;
#14668 = DIRECTION ( 'NONE',  ( 1.000000000000000000, -0.000000000000000000, -0.000000000000000000 ) ) ;
#14669 = ORIENTED_EDGE ( 'NONE', *, *, #39973, .F. ) ;
#14670 = EDGE_LOOP ( 'NONE', ( #25100, #29975, #25892, #43002 ) ) ;
#14671 = CARTESIAN_POINT ( 'NONE',  ( 0.000000000000000000, 0.000000000000000000, 0.000000000000000000 ) ) ;
#14672 = ADVANCED_FACE ( 'NONE', ( #23474 ), #37940, .T. ) ;
#14673 = FACE_OUTER_BOUND ( 'NONE', #34461, .T. ) ;
#14674 = AXIS2_PLACEMENT_3D ( 'NONE', #41911, #40934, #45316 ) ;
#14675 = ORIENTED_EDGE ( 'NONE', *, *, #32753, .T. ) ;
#14676 = ORIENTED_EDGE ( 'NONE', *, *, #7013, .T. ) ;
#14677 = DIRECTION ( 'NONE',  ( 1.000000000000000000, -0.000000000000000000, 0.000000000000000000 ) ) ;
#14678 = DIRECTION ( 'NONE',  ( 0.000000000000000000, -0.8910065241883627918, -0.4539904997395568520 ) ) ;
#14679 = EDGE_LOOP ( 'NONE', ( #4087, #19986, #2300, #16732 ) ) ;
#14680 = DIRECTION ( 'NONE',  ( 1.000000000000000000, 0.000000000000000000, 0.000000000000000000 ) ) ;
#14681 = LINE ( 'NONE', #43804, #22998 ) ;
#14682 = DIRECTION ( 'NONE',  ( -1.000000000000000000, -0.000000000000000000, -0.000000000000000000 ) ) ;
#14683 = DIRECTION ( 'NONE',  ( 0.000000000000000000, 0.000000000000000000, 1.000000000000000000 ) ) ;
#14684 = DIRECTION ( 'NONE',  ( -1.000000000000000000, -0.000000000000000000, -0.000000000000000000 ) ) ;
#14685 = FACE_OUTER_BOUND ( 'NONE', #7912, .T. ) ;
#14686 = AXIS2_PLACEMENT_3D ( 'NONE', #15774, #42875, #9326 ) ;
#14687 = PLANE ( 'NONE',  #42731 ) ;
#14688 = CARTESIAN_POINT ( 'NONE',  ( 10.00000000000000000, -76.66974797899844418, 11.30684508768314522 ) ) ;
#14689 = PLANE ( 'NONE',  #47323 ) ;
#14690 = EDGE_LOOP ( 'NONE', ( #36188, #6631, #9740, #46262, #7191, #29753, #38485, #40889 ) ) ;
#14691 = CARTESIAN_POINT ( 'NONE',  ( 0.000000000000000000, -33.71516098798792171, 74.74816331893418919 ) ) ;
#14692 = CARTESIAN_POINT ( 'NONE',  ( 10.00000000000000000, 49.70050353004889132, 59.46389618801982380 ) ) ;
#14693 = DIRECTION ( 'NONE',  ( 0.000000000000000000, -0.9876883405951359940, -0.1564344650402420822 ) ) ;
#14694 = ORIENTED_EDGE ( 'NONE', *, *, #43702, .F. ) ;
#14695 = EDGE_LOOP ( 'NONE', ( #18555, #2090, #37933, #44013 ) ) ;
#14696 = AXIS2_PLACEMENT_3D ( 'NONE', #22670, #36870, #3835 ) ;
#14697 = EDGE_CURVE ( 'NONE', #17725, #14023, #47980, .T. ) ;
#14698 = DIRECTION ( 'NONE',  ( -1.000000000000000000, 0.000000000000000000, 0.000000000000000000 ) ) ;
#14700 = EDGE_CURVE ( 'NONE', #18493, #25478, #4418, .T. ) ;
#14699 = VECTOR ( 'NONE', #15246, 1000.000000000000000 ) ;
#14701 = DIRECTION ( 'NONE',  ( -1.000000000000000000, -0.000000000000000000, -0.000000000000000000 ) ) ;
#14702 = AXIS2_PLACEMENT_3D ( 'NONE', #44684, #45181, #26575 ) ;
#14703 = ORIENTED_EDGE ( 'NONE', *, *, #40363, .T. ) ;
#14704 = EDGE_CURVE ( 'NONE', #10878, #42173, #13581, .T. ) ;
#14705 = EDGE_CURVE ( 'NONE', #20655, #39405, #229, .T. ) ;
#14706 = EDGE_CURVE ( 'NONE', #8228, #15615, #34485, .T. ) ;
#14707 = CARTESIAN_POINT ( 'NONE',  ( 10.00000000000000000, 34.44570377933598593, 69.42325613327452061 ) ) ;
#14708 = ORIENTED_EDGE ( 'NONE', *, *, #162, .T. ) ;
#14709 = DIRECTION ( 'NONE',  ( -1.000000000000000000, -0.000000000000000000, -0.000000000000000000 ) ) ;
#14710 = ORIENTED_EDGE ( 'NONE', *, *, #41343, .T. ) ;
#14711 = ORIENTED_EDGE ( 'NONE', *, *, #2251, .F. ) ;
#14712 = VERTEX_POINT ( 'NONE', #12247 ) ;
#14713 = ORIENTED_EDGE ( 'NONE', *, *, #18169, .F. ) ;
#14714 = FACE_OUTER_BOUND ( 'NONE', #30592, .T. ) ;
#14715 = PRODUCT_DEFINITION_FORMATION_WITH_SPECIFIED_SOURCE ( 'ANY', '', #46831, .NOT_KNOWN. ) ;
#14716 = AXIS2_PLACEMENT_3D ( 'NONE', #34474, #23467, #7589 ) ;
#14717 = DIRECTION ( 'NONE',  ( -1.000000000000000000, -0.000000000000000000, -0.000000000000000000 ) ) ;
#14718 = ORIENTED_EDGE ( 'NONE', *, *, #46032, .F. ) ;
#14719 = ORIENTED_EDGE ( 'NONE', *, *, #18556, .T. ) ;
#14720 = DIRECTION ( 'NONE',  ( -1.000000000000000000, -0.000000000000000000, 0.000000000000000000 ) ) ;
#14721 = ORIENTED_EDGE ( 'NONE', *, *, #15638, .T. ) ;
#14722 = DIRECTION ( 'NONE',  ( 0.000000000000000000, 1.000000000000000000, 0.000000000000000000 ) ) ;
#14723 = CARTESIAN_POINT ( 'NONE',  ( 0.000000000000000000, 0.000000000000000000, 0.000000000000000000 ) ) ;
#14724 = ORIENTED_EDGE ( 'NONE', *, *, #19897, .T. ) ;
#14725 = CARTESIAN_POINT ( 'NONE',  ( 10.00000000000000000, 6.903761155837774943, 77.19088730480525840 ) ) ;
#14726 = CARTESIAN_POINT ( 'NONE',  ( 0.000000000000000000, -63.18004540532994184, -44.88180994100446952 ) ) ;
#14727 = ORIENTED_EDGE ( 'NONE', *, *, #3871, .T. ) ;
#14728 = DIRECTION ( 'NONE',  ( 0.000000000000000000, 0.000000000000000000, -1.000000000000000000 ) ) ;
#14729 = EDGE_CURVE ( 'NONE', #17607, #28640, #7320, .T. ) ;
#14730 = DIRECTION ( 'NONE',  ( 0.000000000000000000, -0.8910065241883722287, 0.4539904997395382558 ) ) ;
#14731 = EDGE_LOOP ( 'NONE', ( #44370, #14132, #11298, #29679 ) ) ;
#14732 = DIRECTION ( 'NONE',  ( -1.000000000000000000, 0.000000000000000000, 0.000000000000000000 ) ) ;
#14733 = ORIENTED_EDGE ( 'NONE', *, *, #22727, .F. ) ;
#14734 = ORIENTED_EDGE ( 'NONE', *, *, #38760, .F. ) ;
#14735 = DIRECTION ( 'NONE',  ( -1.000000000000000000, -0.000000000000000000, 0.000000000000000000 ) ) ;
#14736 = CARTESIAN_POINT ( 'NONE',  ( -17.26469406256017791, -140.1601175325492648, 5.500000000000000000 ) ) ;
#14737 = VECTOR ( 'NONE', #1425, 1000.000000000000114 ) ;
#14738 = CARTESIAN_POINT ( 'NONE',  ( 20.85212586905262100, -130.9402397935870965, 5.500000000000000000 ) ) ;
#14739 = CYLINDRICAL_SURFACE ( 'NONE', #41469, 31.99999999999998579 ) ;
#14740 = LINE ( 'NONE', #3715, #298 ) ;
#14741 = ADVANCED_FACE ( 'NONE', ( #3916 ), #38418, .F. ) ;
#14742 = AXIS2_PLACEMENT_3D ( 'NONE', #8450, #5276, #31721 ) ;
#14743 = CARTESIAN_POINT ( 'NONE',  ( 12.69589495141918611, -96.69089767102708777, 5.500000000000000000 ) ) ;
#14744 = DIRECTION ( 'NONE',  ( 0.000000000000000000, 0.000000000000000000, 1.000000000000000000 ) ) ;
#14745 = LINE ( 'NONE', #44592, #34081 ) ;
#14746 = EDGE_CURVE ( 'NONE', #37265, #32654, #19815, .T. ) ;
#14747 = DIRECTION ( 'NONE',  ( -1.000000000000000000, -0.000000000000000000, 0.000000000000000000 ) ) ;
#14748 = DIRECTION ( 'NONE',  ( -1.000000000000000000, 0.000000000000000000, 0.000000000000000000 ) ) ;
#14749 = CARTESIAN_POINT ( 'NONE',  ( 0.000000000000000000, -16.65972982744991171, 80.28980883073752750 ) ) ;
#14750 = FACE_OUTER_BOUND ( 'NONE', #39813, .T. ) ;
#14751 = CARTESIAN_POINT ( 'NONE',  ( 0.000000000000000000, 0.000000000000000000, 0.000000000000000000 ) ) ;
#14752 = DIRECTION ( 'NONE',  ( -1.000000000000000000, -0.000000000000000000, -0.000000000000000000 ) ) ;
#14753 = VERTEX_POINT ( 'NONE', #44538 ) ;
#14754 = LINE ( 'NONE', #22813, #16276 ) ;
#14755 = DIRECTION ( 'NONE',  ( -1.000000000000000000, 0.000000000000000000, 0.000000000000000000 ) ) ;
#14756 = ORIENTED_EDGE ( 'NONE', *, *, #13261, .T. ) ;
#14757 = CIRCLE ( 'NONE', #26453, 82.00000000000000000 ) ;
#14758 = EDGE_CURVE ( 'NONE', #36706, #33430, #723, .T. ) ;
#14759 = ORIENTED_EDGE ( 'NONE', *, *, #45088, .F. ) ;
#14760 = DIRECTION ( 'NONE',  ( -0.4999999999999919509, -0.8660254037844432595, 0.000000000000000000 ) ) ;
#14761 = ORIENTED_EDGE ( 'NONE', *, *, #27834, .F. ) ;
#14762 = EDGE_CURVE ( 'NONE', #45279, #34171, #15655, .T. ) ;
#14763 = DIRECTION ( 'NONE',  ( -1.000000000000000000, -0.000000000000000000, 0.000000000000000000 ) ) ;
#14764 = DIRECTION ( 'NONE',  ( -0.3373011080932099559, -0.9413968145681674837, -0.000000000000000000 ) ) ;
#14765 = EDGE_CURVE ( 'NONE', #11748, #27398, #9660, .T. ) ;
#14766 = LINE ( 'NONE', #29449, #28359 ) ;
#14767 = ORIENTED_EDGE ( 'NONE', *, *, #5145, .F. ) ;
#14768 = CIRCLE ( 'NONE', #15634, 77.49900000000000944 ) ;
#14769 = ADVANCED_FACE ( 'NONE', ( #14940 ), #8065, .F. ) ;
#14770 = CYLINDRICAL_SURFACE ( 'NONE', #15242, 31.99999999999998579 ) ;
#14771 = AXIS2_PLACEMENT_3D ( 'NONE', #24207, #12713, #4881 ) ;
#14772 = ORIENTED_EDGE ( 'NONE', *, *, #17370, .F. ) ;
#14773 = VECTOR ( 'NONE', #3872, 1000.000000000000114 ) ;
#14774 = CARTESIAN_POINT ( 'NONE',  ( -235.0000123116479926, -123.0000000000000284, -2.500000000000000000 ) ) ;
#14775 = LINE ( 'NONE', #30198, #7798 ) ;
#14777 = ORIENTED_EDGE ( 'NONE', *, *, #29724, .F. ) ;
#14776 = CARTESIAN_POINT ( 'NONE',  ( 0.000000000000000000, 0.000000000000000000, 0.000000000000000000 ) ) ;
#14778 = ORIENTED_EDGE ( 'NONE', *, *, #10693, .F. ) ;
#14779 = DIRECTION ( 'NONE',  ( -1.000000000000000000, 0.000000000000000000, 0.000000000000000000 ) ) ;
#14780 = VERTEX_POINT ( 'NONE', #33763 ) ;
#14781 = DIRECTION ( 'NONE',  ( -1.000000000000000000, 0.000000000000000000, -0.000000000000000000 ) ) ;
#14782 = FACE_OUTER_BOUND ( 'NONE', #13817, .T. ) ;
#14783 = FACE_OUTER_BOUND ( 'NONE', #6680, .T. ) ;
#14784 = COLOUR_RGB ( '', 0.31764706, 0.68627451, 0.89019608) ;
#14785 = CARTESIAN_POINT ( 'NONE',  ( 11.99999999999999822, 14.67089635893713684, 73.72996012237443608 ) ) ;
#14786 = EDGE_LOOP ( 'NONE', ( #31787, #18488, #10416, #28571 ) ) ;
#14787 = DIRECTION ( 'NONE',  ( -1.000000000000000000, -0.000000000000000000, 0.000000000000000000 ) ) ;
#14788 = EDGE_LOOP ( 'NONE', ( #43529, #19141, #21327, #2975 ) ) ;
#14789 = ORIENTED_EDGE ( 'NONE', *, *, #35644, .F. ) ;
#14790 = CARTESIAN_POINT ( 'NONE',  ( 0.000000000000000000, 0.000000000000000000, 0.000000000000000000 ) ) ;
#14791 = DIRECTION ( 'NONE',  ( 0.000000000000000000, 0.6494480483301793283, 0.7604059656000345946 ) ) ;
#14792 = CARTESIAN_POINT ( 'NONE',  ( 11.99999999999999822, 23.16143007188530589, -73.95703589263951017 ) ) ;
#14793 = FACE_OUTER_BOUND ( 'NONE', #29580, .T. ) ;
#14794 = ORIENTED_EDGE ( 'NONE', *, *, #4531, .F. ) ;
#14795 = DIRECTION ( 'NONE',  ( -1.000000000000000000, 0.000000000000000000, 0.000000000000000000 ) ) ;
#14796 = DIRECTION ( 'NONE',  ( 0.000000000000000000, 0.000000000000000000, 1.000000000000000000 ) ) ;
#14797 = ORIENTED_EDGE ( 'NONE', *, *, #23068, .T. ) ;
#14798 = CARTESIAN_POINT ( 'NONE',  ( 5.000000000000000000, 39.04073710021344112, 15.48615015657596850 ) ) ;
#14799 = CARTESIAN_POINT ( 'NONE',  ( 0.9774260708577211521, -121.1378217241763622, 2.500000000000000000 ) ) ;
#14801 = CIRCLE ( 'NONE', #42149, 31.99999999999998579 ) ;
#14800 = LINE ( 'NONE', #44898, #42662 ) ;
#14802 = AXIS2_PLACEMENT_3D ( 'NONE', #36663, #14407, #21972 ) ;
#14803 = CYLINDRICAL_SURFACE ( 'NONE', #1155, 31.99999999999999289 ) ;
#14804 = CARTESIAN_POINT ( 'NONE',  ( 15.00000000000000000, 16.83928648764922542, -16.46020748918050458 ) ) ;
#14805 = LINE ( 'NONE', #5593, #19270 ) ;
#14806 = ADVANCED_FACE ( 'NONE', ( #496 ), #37689, .T. ) ;
#14807 = AXIS2_PLACEMENT_3D ( 'NONE', #2637, #2400, #17329 ) ;
#14808 = DIRECTION ( 'NONE',  ( -1.000000000000000000, 0.000000000000000000, 0.000000000000000000 ) ) ;
#14809 = CARTESIAN_POINT ( 'NONE',  ( 0.000000000000000000, 0.000000000000000000, 37.49900000000000233 ) ) ;
#14810 = DIRECTION ( 'NONE',  ( 0.000000000000000000, 0.9876883405951382144, -0.1564344650402276493 ) ) ;
#14811 = DIRECTION ( 'NONE',  ( 0.000000000000000000, 0.3090169943749480619, -0.9510565162951533091 ) ) ;
#14812 = DIRECTION ( 'NONE',  ( -1.000000000000000000, 0.000000000000000000, 0.000000000000000000 ) ) ;
#14813 = CIRCLE ( 'NONE', #28120, 31.99999999999998579 ) ;
#14814 = CARTESIAN_POINT ( 'NONE',  ( 3.429551818649054340, -146.3199197248623875, 5.500000000000000000 ) ) ;
#14815 = CARTESIAN_POINT ( 'NONE',  ( 11.99999999999999822, 74.65491531819118620, 23.16904090965732621 ) ) ;
#14816 = EDGE_CURVE ( 'NONE', #44741, #22704, #45619, .T. ) ;
#14817 = FACE_OUTER_BOUND ( 'NONE', #18364, .T. ) ;
#14818 = ADVANCED_FACE ( 'NONE', ( #45278 ), #39143, .F. ) ;
#14819 = EDGE_CURVE ( 'NONE', #14564, #33636, #40950, .T. ) ;
#14820 = ORIENTED_EDGE ( 'NONE', *, *, #16239, .T. ) ;
#14821 = EDGE_CURVE ( 'NONE', #29948, #28234, #19795, .T. ) ;
#14822 = EDGE_CURVE ( 'NONE', #28052, #30791, #26082, .T. ) ;
#14823 = VERTEX_POINT ( 'NONE', #13199 ) ;
#14824 = VERTEX_POINT ( 'NONE', #24447 ) ;
#14825 = EDGE_CURVE ( 'NONE', #43468, #2823, #300, .T. ) ;
#14826 = CARTESIAN_POINT ( 'NONE',  ( 4.999999999999999112, 3.925862922256769583, -41.81611651403857621 ) ) ;
#14827 = ORIENTED_EDGE ( 'NONE', *, *, #10784, .T. ) ;
#14828 = AXIS2_PLACEMENT_3D ( 'NONE', #2441, #46535, #17367 ) ;
#14829 = CARTESIAN_POINT ( 'NONE',  ( 0.000000000000000000, 0.000000000000000000, 0.000000000000000000 ) ) ;
#14830 = ORIENTED_EDGE ( 'NONE', *, *, #2535, .T. ) ;
#14831 = AXIS2_PLACEMENT_3D ( 'NONE', #4308, #45175, #11638 ) ;
#14832 = DIRECTION ( 'NONE',  ( 0.000000000000000000, 0.000000000000000000, 1.000000000000000000 ) ) ;
#14834 = ORIENTED_EDGE ( 'NONE', *, *, #35756, .T. ) ;
#14833 = DIRECTION ( 'NONE',  ( -0.6516173805718079581, 0.7585478161175704948, 0.000000000000000000 ) ) ;
#14835 = VECTOR ( 'NONE', #7945, 1000.000000000000000 ) ;
#14836 = ORIENTED_EDGE ( 'NONE', *, *, #47902, .F. ) ;
#14837 = LINE ( 'NONE', #40536, #13323 ) ;
#14838 = ORIENTED_EDGE ( 'NONE', *, *, #4144, .T. ) ;
#14839 = ORIENTED_EDGE ( 'NONE', *, *, #1036, .F. ) ;
#14840 = ORIENTED_EDGE ( 'NONE', *, *, #6568, .F. ) ;
#14841 = CYLINDRICAL_SURFACE ( 'NONE', #28813, 32.00000000000000000 ) ;
#14842 = LINE ( 'NONE', #27070, #6378 ) ;
#14843 = CYLINDRICAL_SURFACE ( 'NONE', #11089, 82.00000000000000000 ) ;
#14844 = EDGE_LOOP ( 'NONE', ( #21311, #44640, #4844, #47141 ) ) ;
#14845 = ORIENTED_EDGE ( 'NONE', *, *, #46870, .T. ) ;
#14846 = VECTOR ( 'NONE', #5693, 1000.000000000000000 ) ;
#14847 = DIRECTION ( 'NONE',  ( -1.000000000000000000, 0.000000000000000000, -0.000000000000000000 ) ) ;
#14848 = VERTEX_POINT ( 'NONE', #27408 ) ;
#14849 = FACE_OUTER_BOUND ( 'NONE', #32244, .T. ) ;
#14850 = DIRECTION ( 'NONE',  ( 0.7273375899149812085, -0.6862798483830533369, 0.000000000000000000 ) ) ;
#14851 = CARTESIAN_POINT ( 'NONE',  ( 15.00000000000000000, -1.278221433540507546, -26.51162292216071492 ) ) ;
#14852 = DIRECTION ( 'NONE',  ( -1.000000000000000000, -0.000000000000000000, -0.000000000000000000 ) ) ;
#14853 = CARTESIAN_POINT ( 'NONE',  ( -12.40464318976452596, 10.41032311384371489, 52.00000000000002132 ) ) ;
#14854 = CARTESIAN_POINT ( 'NONE',  ( 10.00000000000000000, 41.76106447765489094, 62.50884508063442269 ) ) ;
#14855 = DIRECTION ( 'NONE',  ( 1.000000000000000000, 0.000000000000000000, 0.000000000000000000 ) ) ;
#14856 = DIRECTION ( 'NONE',  ( 0.000000000000000000, 0.000000000000000000, 1.000000000000000000 ) ) ;
#14857 = VERTEX_POINT ( 'NONE', #42584 ) ;
#14858 = FACE_OUTER_BOUND ( 'NONE', #46984, .T. ) ;
#14859 = EDGE_CURVE ( 'NONE', #18007, #28297, #12853, .T. ) ;
#14860 = ORIENTED_EDGE ( 'NONE', *, *, #9626, .F. ) ;
#14861 = FACE_OUTER_BOUND ( 'NONE', #13215, .T. ) ;
#14862 = VERTEX_POINT ( 'NONE', #31827 ) ;
#14863 = EDGE_CURVE ( 'NONE', #22486, #44741, #6591, .T. ) ;
#14864 = CARTESIAN_POINT ( 'NONE',  ( 0.000000000000000000, 0.000000000000000000, 0.000000000000000000 ) ) ;
#14865 = DIRECTION ( 'NONE',  ( -1.000000000000000000, 0.000000000000000000, -0.000000000000000000 ) ) ;
#14866 = DIRECTION ( 'NONE',  ( -1.000000000000000000, 0.000000000000000000, 0.000000000000000000 ) ) ;
#14867 = EDGE_CURVE ( 'NONE', #34100, #8511, #9759, .T. ) ;
#14868 = CARTESIAN_POINT ( 'NONE',  ( 10.00000000000000000, 37.01155633439068282, -6.555932627142014191 ) ) ;
#14869 = DIRECTION ( 'NONE',  ( 0.000000000000000000, 0.8090169943749487835, -0.5877852522924712497 ) ) ;
#14870 = AXIS2_PLACEMENT_3D ( 'NONE', #11642, #7954, #22890 ) ;
#14871 = DIRECTION ( 'NONE',  ( 0.000000000000000000, 0.000000000000000000, 1.000000000000000000 ) ) ;
#14872 = DIRECTION ( 'NONE',  ( 0.000000000000000000, 0.4539904997395413644, 0.8910065241883706744 ) ) ;
#14873 = AXIS2_PLACEMENT_3D ( 'NONE', #24104, #5269, #46371 ) ;
#14874 = AXIS2_PLACEMENT_3D ( 'NONE', #37694, #41613, #23011 ) ;
#14875 = CARTESIAN_POINT ( 'NONE',  ( 10.00000000000000000, 16.65560815589464028, -38.55633173626993937 ) ) ;
#14876 = DIRECTION ( 'NONE',  ( -1.000000000000000000, -0.000000000000000000, -0.000000000000000000 ) ) ;
#14877 = AXIS2_PLACEMENT_3D ( 'NONE', #1860, #42488, #23887 ) ;
#14878 = EDGE_CURVE ( 'NONE', #19822, #15289, #10505, .T. ) ;
#14879 = ADVANCED_FACE ( 'NONE', ( #31328 ), #32051, .F. ) ;
#14880 = VERTEX_POINT ( 'NONE', #46968 ) ;
#14881 = CIRCLE ( 'NONE', #34489, 42.00000000000000000 ) ;
#14882 = AXIS2_PLACEMENT_3D ( 'NONE', #32765, #25910, #25659 ) ;
#14883 = ORIENTED_EDGE ( 'NONE', *, *, #48335, .F. ) ;
#14884 = CARTESIAN_POINT ( 'NONE',  ( 10.00000000000000000, 76.66974797899837313, 11.30684508768368524 ) ) ;
#14885 = CARTESIAN_POINT ( 'NONE',  ( 10.00000000000000000, -72.35160999960801576, -20.41045688087902121 ) ) ;
#14886 = EDGE_CURVE ( 'NONE', #29480, #19341, #1463, .T. ) ;
#14887 = CARTESIAN_POINT ( 'NONE',  ( 0.000000000000000000, 0.000000000000000000, 0.000000000000000000 ) ) ;
#14888 = ORIENTED_EDGE ( 'NONE', *, *, #37714, .F. ) ;
#14889 = ORIENTED_EDGE ( 'NONE', *, *, #37626, .F. ) ;
#14890 = FACE_OUTER_BOUND ( 'NONE', #28591, .T. ) ;
#14891 = ORIENTED_EDGE ( 'NONE', *, *, #315, .T. ) ;
#14892 = VECTOR ( 'NONE', #29029, 1000.000000000000114 ) ;
#14893 = FACE_OUTER_BOUND ( 'NONE', #14534, .T. ) ;
#14894 = VERTEX_POINT ( 'NONE', #1700 ) ;
#14895 = FACE_OUTER_BOUND ( 'NONE', #16104, .T. ) ;
#14896 = ORIENTED_EDGE ( 'NONE', *, *, #25767, .F. ) ;
#14897 = CYLINDRICAL_SURFACE ( 'NONE', #33761, 77.49899999999999523 ) ;
#14898 = CIRCLE ( 'NONE', #4767, 37.49900000000000944 ) ;
#14899 = CIRCLE ( 'NONE', #10179, 15.99999999999999822 ) ;
#14900 = DIRECTION ( 'NONE',  ( -1.000000000000000000, 0.000000000000000000, -0.000000000000000000 ) ) ;
#14901 = CARTESIAN_POINT ( 'NONE',  ( 11.99999999999999822, -73.72996012237429397, -14.67089635893794508 ) ) ;
#14902 = ORIENTED_EDGE ( 'NONE', *, *, #48394, .F. ) ;
#14903 = VECTOR ( 'NONE', #16652, 1000.000000000000000 ) ;
#14904 = EDGE_LOOP ( 'NONE', ( #20458, #34140, #41389, #35011 ) ) ;
#14905 = AXIS2_PLACEMENT_3D ( 'NONE', #36748, #21095, #10325 ) ;
#14906 = DIRECTION ( 'NONE',  ( 0.000000000000000000, 0.000000000000000000, 1.000000000000000000 ) ) ;
#14907 = DIRECTION ( 'NONE',  ( -1.000000000000000000, 0.000000000000000000, 0.000000000000000000 ) ) ;
#14908 = ADVANCED_FACE ( 'NONE', ( #42330 ), #4882, .T. ) ;
#14909 = ORIENTED_EDGE ( 'NONE', *, *, #16265, .F. ) ;
#14910 = CIRCLE ( 'NONE', #10225, 31.99999999999999289 ) ;
#14911 = ORIENTED_EDGE ( 'NONE', *, *, #42683, .T. ) ;
#14912 = CARTESIAN_POINT ( 'NONE',  ( -10.00000000000000000, 0.000000000000000000, 0.000000000000000000 ) ) ;
#14913 = ORIENTED_EDGE ( 'NONE', *, *, #14500, .F. ) ;
#14914 = DIRECTION ( 'NONE',  ( 0.000000000000000000, 0.000000000000000000, 1.000000000000000000 ) ) ;
#14915 = EDGE_CURVE ( 'NONE', #17845, #4123, #20287, .T. ) ;
#14916 = DIRECTION ( 'NONE',  ( -1.000000000000000000, -0.000000000000000000, -0.000000000000000000 ) ) ;
#14917 = FACE_OUTER_BOUND ( 'NONE', #43422, .T. ) ;
#14918 = LINE ( 'NONE', #29366, #29233 ) ;
#14919 = LINE ( 'NONE', #4403, #22094 ) ;
#14920 = CARTESIAN_POINT ( 'NONE',  ( 4.999999999999999112, 40.68715046381927891, 10.41901085202092858 ) ) ;
#14921 = ADVANCED_FACE ( 'NONE', ( #5616 ), #16624, .F. ) ;
#14922 = DIRECTION ( 'NONE',  ( 0.000000000000000000, 0.7071067811865439090, 0.7071067811865512365 ) ) ;
#14923 = DIRECTION ( 'NONE',  ( 1.000000000000000000, 0.000000000000000000, -0.000000000000000000 ) ) ;
#14924 = CARTESIAN_POINT ( 'NONE',  ( 1.499592026101426168, -120.0349822133818094, -2.500000000000000000 ) ) ;
#14925 = DIRECTION ( 'NONE',  ( 1.000000000000000000, 0.000000000000000000, 0.000000000000000000 ) ) ;
#14926 = DIRECTION ( 'NONE',  ( -1.000000000000000000, -0.000000000000000000, 0.000000000000000000 ) ) ;
#14927 = CARTESIAN_POINT ( 'NONE',  ( -10.00000000000000000, 0.000000000000000000, 0.000000000000000000 ) ) ;
#14928 = ORIENTED_EDGE ( 'NONE', *, *, #14528, .F. ) ;
#14929 = EDGE_CURVE ( 'NONE', #20943, #46617, #32395, .T. ) ;
#14930 = ADVANCED_FACE ( 'NONE', ( #23981 ), #35463, .T. ) ;
#14931 = ORIENTED_EDGE ( 'NONE', *, *, #31617, .F. ) ;
#14932 = AXIS2_PLACEMENT_3D ( 'NONE', #1320, #23339, #16254 ) ;
#14933 = VECTOR ( 'NONE', #25834, 1000.000000000000000 ) ;
#14934 = ADVANCED_FACE ( 'NONE', ( #39869 ), #21503, .T. ) ;
#14935 = PRODUCT_DEFINITION_CONTEXT ( 'detailed design', #25696, 'design' ) ;
#14936 = DIRECTION ( 'NONE',  ( 0.000000000000000000, 0.000000000000000000, -1.000000000000000000 ) ) ;
#14937 = AXIS2_PLACEMENT_3D ( 'NONE', #17184, #10094, #6905 ) ;
#14938 = AXIS2_PLACEMENT_3D ( 'NONE', #3632, #36904, #26152 ) ;
#14939 = CARTESIAN_POINT ( 'NONE',  ( 11.99999999999999822, 0.000000000000000000, 0.000000000000000000 ) ) ;
#14940 = FACE_OUTER_BOUND ( 'NONE', #48296, .T. ) ;
#14941 = ORIENTED_EDGE ( 'NONE', *, *, #10278, .T. ) ;
#14942 = CIRCLE ( 'NONE', #26683, 37.49900000000000233 ) ;
#14943 = CIRCLE ( 'NONE', #40720, 30.50000000000000000 ) ;
#14944 = ADVANCED_FACE ( 'NONE', ( #47914 ), #47207, .T. ) ;
#14945 = AXIS2_PLACEMENT_3D ( 'NONE', #35627, #31971, #46403 ) ;
#14946 = CARTESIAN_POINT ( 'NONE',  ( 0.000000000000000000, 0.000000000000000000, 0.000000000000000000 ) ) ;
#14947 = VERTEX_POINT ( 'NONE', #21013 ) ;
#14948 = ORIENTED_EDGE ( 'NONE', *, *, #5365, .T. ) ;
#14949 = VERTEX_POINT ( 'NONE', #3367 ) ;
#14950 = VERTEX_POINT ( 'NONE', #21967 ) ;
#14951 = ORIENTED_EDGE ( 'NONE', *, *, #22001, .T. ) ;
#14952 = FACE_OUTER_BOUND ( 'NONE', #11299, .T. ) ;
#14953 = DIRECTION ( 'NONE',  ( 0.000000000000000000, 0.000000000000000000, 1.000000000000000000 ) ) ;
#14954 = VERTEX_POINT ( 'NONE', #48167 ) ;
#14955 = ORIENTED_EDGE ( 'NONE', *, *, #19100, .T. ) ;
#14956 = CARTESIAN_POINT ( 'NONE',  ( 10.00000000000000000, 0.000000000000000000, 0.000000000000000000 ) ) ;
#14957 = VERTEX_POINT ( 'NONE', #17330 ) ;
#14958 = DIRECTION ( 'NONE',  ( 0.000000000000000000, 0.000000000000000000, 1.000000000000000000 ) ) ;
#14959 = CYLINDRICAL_SURFACE ( 'NONE', #40820, 77.49899999999999523 ) ;
#14960 = ORIENTED_EDGE ( 'NONE', *, *, #48094, .T. ) ;
#14961 = CARTESIAN_POINT ( 'NONE',  ( 11.99999999999999822, 0.000000000000000000, 0.000000000000000000 ) ) ;
#14962 = FACE_OUTER_BOUND ( 'NONE', #17919, .T. ) ;
#14963 = VERTEX_POINT ( 'NONE', #32745 ) ;
#14964 = AXIS2_PLACEMENT_3D ( 'NONE', #22566, #29173, #38718 ) ;
#14966 = ORIENTED_EDGE ( 'NONE', *, *, #28590, .T. ) ;
#14965 = LINE ( 'NONE', #40437, #31275 ) ;
#14967 = DIRECTION ( 'NONE',  ( -1.000000000000000000, 0.000000000000000000, 0.000000000000000000 ) ) ;
#14968 = ORIENTED_EDGE ( 'NONE', *, *, #44378, .F. ) ;
#14969 = AXIS2_PLACEMENT_3D ( 'NONE', #24599, #20926, #1842 ) ;
#14970 = DIRECTION ( 'NONE',  ( 1.000000000000000000, 0.000000000000000000, 0.000000000000000000 ) ) ;
#14971 = ORIENTED_EDGE ( 'NONE', *, *, #31300, .F. ) ;
#14972 = ORIENTED_EDGE ( 'NONE', *, *, #16809, .F. ) ;
#14973 = DIRECTION ( 'NONE',  ( -1.000000000000000000, 0.000000000000000000, 0.000000000000000000 ) ) ;
#14974 = CARTESIAN_POINT ( 'NONE',  ( -3.000000000000000000, 8.688484142253939169, 21.88630264137371029 ) ) ;
#14975 = CIRCLE ( 'NONE', #45435, 14.09999999999999964 ) ;
#14976 = VERTEX_POINT ( 'NONE', #2893 ) ;
#14977 = CIRCLE ( 'NONE', #33718, 32.00000000000000000 ) ;
#14978 = EDGE_CURVE ( 'NONE', #17019, #13986, #11280, .T. ) ;
#14979 = CARTESIAN_POINT ( 'NONE',  ( 2.874421927457452952, -143.3717286177755739, 5.500000000000000000 ) ) ;
#14980 = CARTESIAN_POINT ( 'NONE',  ( -12.00000000000000000, 17.30399999999999849, 0.000000000000000000 ) ) ;
#14981 = DIRECTION ( 'NONE',  ( -1.000000000000000000, -0.000000000000000000, -0.000000000000000000 ) ) ;
#14982 = ADVANCED_FACE ( 'NONE', ( #10234 ), #17816, .F. ) ;
#14983 = CARTESIAN_POINT ( 'NONE',  ( 0.000000000000000000, -31.47745569255092235, -68.26794271651296242 ) ) ;
#14984 = EDGE_CURVE ( 'NONE', #29567, #19983, #7355, .T. ) ;
#14985 = AXIS2_PLACEMENT_3D ( 'NONE', #14131, #33214, #36872 ) ;
#14986 = LINE ( 'NONE', #14254, #1651 ) ;
#14987 = DIRECTION ( 'NONE',  ( -1.000000000000000000, 0.000000000000000000, -0.000000000000000000 ) ) ;
#14988 = VERTEX_POINT ( 'NONE', #36180 ) ;
#14989 = DIRECTION ( 'NONE',  ( 0.000000000000000000, -0.8526401643540971742, 0.5224985647159409163 ) ) ;
#14991 = EDGE_CURVE ( 'NONE', #36404, #11421, #14158, .T. ) ;
#14990 = CARTESIAN_POINT ( 'NONE',  ( 0.000000000000000000, -0.8299999999999999600, 0.000000000000000000 ) ) ;
#14992 = CIRCLE ( 'NONE', #42334, 31.99999999999999289 ) ;
#14993 = CYLINDRICAL_SURFACE ( 'NONE', #30303, 82.00000000000000000 ) ;
#14994 = CARTESIAN_POINT ( 'NONE',  ( -10.00000000000000000, 0.000000000000000000, 0.000000000000000000 ) ) ;
#14995 = AXIS2_PLACEMENT_3D ( 'NONE', #33548, #37704, #15207 ) ;
#14996 = DIRECTION ( 'NONE',  ( -0.000000000000000000, 0.1045284632676559550, -0.9945218953682731788 ) ) ;
#14997 = CARTESIAN_POINT ( 'NONE',  ( 0.000000000000000000, 74.65374052328648702, 8.840884882375350529 ) ) ;
#14998 = LINE ( 'NONE', #15477, #31136 ) ;
#14999 = DIRECTION ( 'NONE',  ( 1.000000000000000000, 0.000000000000000000, 0.000000000000000000 ) ) ;
#15000 = ADVANCED_FACE ( 'NONE', ( #44012 ), #10968, .T. ) ;
#15001 = FACE_OUTER_BOUND ( 'NONE', #29578, .T. ) ;
#15002 = ORIENTED_EDGE ( 'NONE', *, *, #38127, .F. ) ;
#15003 = EDGE_CURVE ( 'NONE', #4790, #15507, #10483, .T. ) ;
#15004 = DIRECTION ( 'NONE',  ( 0.000000000000000000, -0.4067366430758009854, -0.9135454576426004225 ) ) ;
#15005 = CARTESIAN_POINT ( 'NONE',  ( -8.944667923005411581E-16, -120.0000000000000142, -55.00000000000000711 ) ) ;
#15006 = CARTESIAN_POINT ( 'NONE',  ( -12.40464318976452596, 10.41032311384371489, 32.98187577049606745 ) ) ;
#15007 = ORIENTED_EDGE ( 'NONE', *, *, #43427, .T. ) ;
#15008 = CIRCLE ( 'NONE', #16541, 77.49899999999999523 ) ;
#15009 = EDGE_CURVE ( 'NONE', #45983, #28806, #2401, .T. ) ;
#15010 = VECTOR ( 'NONE', #26440, 1000.000000000000000 ) ;
#15011 = CIRCLE ( 'NONE', #23594, 82.00000000000000000 ) ;
#15012 = LINE ( 'NONE', #22585, #31560 ) ;
#15013 = ORIENTED_EDGE ( 'NONE', *, *, #26432, .F. ) ;
#15014 = AXIS2_PLACEMENT_3D ( 'NONE', #7456, #22388, #34339 ) ;
#15015 = EDGE_CURVE ( 'NONE', #4524, #41629, #6819, .T. ) ;
#15016 = DIRECTION ( 'NONE',  ( -1.000000000000000000, 0.000000000000000000, 0.000000000000000000 ) ) ;
#15017 = DIRECTION ( 'NONE',  ( 0.000000000000000000, -0.000000000000000000, 1.000000000000000000 ) ) ;
#15019 = EDGE_LOOP ( 'NONE', ( #45410, #39618, #41334, #4086 ) ) ;
#15018 = CARTESIAN_POINT ( 'NONE',  ( 0.000000000000000000, 62.20884554314085335, -46.21855187248562657 ) ) ;
#15020 = AXIS2_PLACEMENT_3D ( 'NONE', #35959, #48186, #14665 ) ;
#15021 = ORIENTED_EDGE ( 'NONE', *, *, #21041, .T. ) ;
#15022 = EDGE_LOOP ( 'NONE', ( #32589, #46963, #38011, #39110 ) ) ;
#15023 = FACE_OUTER_BOUND ( 'NONE', #7852, .T. ) ;
#15024 = DIRECTION ( 'NONE',  ( -1.000000000000000000, 0.000000000000000000, -0.000000000000000000 ) ) ;
#15025 = DIRECTION ( 'NONE',  ( 0.000000000000000000, 0.000000000000000000, 1.000000000000000000 ) ) ;
#15026 = CARTESIAN_POINT ( 'NONE',  ( 0.000000000000000000, 40.65526001592713357, -71.21200624218752750 ) ) ;
#15027 = ORIENTED_EDGE ( 'NONE', *, *, #24210, .F. ) ;
#15028 = CYLINDRICAL_SURFACE ( 'NONE', #47455, 31.99999999999999289 ) ;
#15029 = VERTEX_POINT ( 'NONE', #13683 ) ;
#15030 = VERTEX_POINT ( 'NONE', #28614 ) ;
#15031 = EDGE_CURVE ( 'NONE', #41319, #48218, #26937, .T. ) ;
#15032 = CARTESIAN_POINT ( 'NONE',  ( 10.00000000000000000, 37.01155633439068282, -6.555932627142014191 ) ) ;
#15033 = CARTESIAN_POINT ( 'NONE',  ( 0.000000000000000000, 4.992566952384984269, 37.16516213103279398 ) ) ;
#15034 = FACE_OUTER_BOUND ( 'NONE', #40012, .T. ) ;
#15035 = CYLINDRICAL_SURFACE ( 'NONE', #806, 31.99999999999999289 ) ;
#15036 = ORIENTED_EDGE ( 'NONE', *, *, #44474, .T. ) ;
#15037 = CARTESIAN_POINT ( 'NONE',  ( 10.00000000000000000, 23.16143007188532366, -73.95703589263949596 ) ) ;
#15038 = CARTESIAN_POINT ( 'NONE',  ( 10.00000000000000000, 10.96151621346540317, -35.95386929396244113 ) ) ;
#15039 = EDGE_CURVE ( 'NONE', #46824, #40640, #8924, .T. ) ;
#15040 = DIRECTION ( 'NONE',  ( 1.000000000000000000, 0.000000000000000000, 0.000000000000000000 ) ) ;
#15041 = AXIS2_PLACEMENT_3D ( 'NONE', #28055, #31493, #27567 ) ;
#15042 = DIRECTION ( 'NONE',  ( 1.000000000000000000, -0.000000000000000000, -0.000000000000000000 ) ) ;
#15043 = LINE ( 'NONE', #11613, #34816 ) ;
#15044 = DIRECTION ( 'NONE',  ( 0.000000000000000000, 0.000000000000000000, 1.000000000000000000 ) ) ;
#15046 = EDGE_CURVE ( 'NONE', #46234, #16188, #32990, .T. ) ;
#15045 = FACE_OUTER_BOUND ( 'NONE', #33707, .T. ) ;
#15047 = CARTESIAN_POINT ( 'NONE',  ( 0.000000000000000000, 10.96151621346487914, 35.95386929396260456 ) ) ;
#15048 = CIRCLE ( 'NONE', #30654, 82.00000000000000000 ) ;
#15049 = CARTESIAN_POINT ( 'NONE',  ( 0.000000000000000000, 3.894527615417891830, 81.90746397400390322 ) ) ;
#15050 = CARTESIAN_POINT ( 'NONE',  ( 10.00000000000000000, 33.80338159004307386, -16.23288003029461279 ) ) ;
#15051 = AXIS2_PLACEMENT_3D ( 'NONE', #2272, #18087, #46835 ) ;
#15052 = CARTESIAN_POINT ( 'NONE',  ( 10.00000000000000000, -49.70050353004933896, 59.46389618801946852 ) ) ;
#15053 = CARTESIAN_POINT ( 'NONE',  ( -0.9515373497862389396, -96.47140937769621871, 5.500000000000000000 ) ) ;
#15054 = CARTESIAN_POINT ( 'NONE',  ( 10.00000000000000000, -21.60688246758529019, -79.10210256391388839 ) ) ;
#15055 = CARTESIAN_POINT ( 'NONE',  ( 10.00000000000000000, 0.000000000000000000, 0.000000000000000000 ) ) ;
#15056 = CARTESIAN_POINT ( 'NONE',  ( 11.99999999999999822, -74.65491531819124305, 8.830959090342128448 ) ) ;
#15057 = CIRCLE ( 'NONE', #28323, 31.99999999999998579 ) ;
#15058 = FACE_OUTER_BOUND ( 'NONE', #32718, .T. ) ;
#15059 = VERTEX_POINT ( 'NONE', #7042 ) ;
#15060 = VERTEX_POINT ( 'NONE', #13914 ) ;
#15061 = AXIS2_PLACEMENT_3D ( 'NONE', #6603, #18581, #17609 ) ;
#15062 = LINE ( 'NONE', #44926, #44525 ) ;
#15063 = CIRCLE ( 'NONE', #29914, 31.99999999999998579 ) ;
#15064 = ORIENTED_EDGE ( 'NONE', *, *, #20704, .T. ) ;
#15065 = AXIS2_PLACEMENT_3D ( 'NONE', #19657, #35087, #39011 ) ;
#15066 = AXIS2_PLACEMENT_3D ( 'NONE', #28042, #10089, #34633 ) ;
#15067 = FACE_OUTER_BOUND ( 'NONE', #47853, .T. ) ;
#15068 =( REPRESENTATION_RELATIONSHIP ('NONE','NONE', #5957, #37520 ) REPRESENTATION_RELATIONSHIP_WITH_TRANSFORMATION ( #4942 )SHAPE_REPRESENTATION_RELATIONSHIP( ) );
#15069 = LINE ( 'NONE', #15792, #6241 ) ;
#15070 = AXIS2_PLACEMENT_3D ( 'NONE', #11235, #4130, #46215 ) ;
#15071 = CARTESIAN_POINT ( 'NONE',  ( 0.000000000000000000, 0.000000000000000000, 0.000000000000000000 ) ) ;
#15072 = VERTEX_POINT ( 'NONE', #28839 ) ;
#15073 = CARTESIAN_POINT ( 'NONE',  ( 0.000000000000000000, 12.42422080174638310, 35.38097989696515810 ) ) ;
#15074 = VECTOR ( 'NONE', #4128, 1000.000000000000114 ) ;
#15075 = ORIENTED_EDGE ( 'NONE', *, *, #45712, .T. ) ;
#15076 = VERTEX_POINT ( 'NONE', #43771 ) ;
#15077 = AXIS2_PLACEMENT_3D ( 'NONE', #27389, #42313, #27627 ) ;
#15078 = ORIENTED_EDGE ( 'NONE', *, *, #8301, .T. ) ;
#15079 = CARTESIAN_POINT ( 'NONE',  ( 0.000000000000000000, 0.000000000000000000, 0.000000000000000000 ) ) ;
#15080 = DIRECTION ( 'NONE',  ( -1.000000000000000000, 0.000000000000000000, 0.000000000000000000 ) ) ;
#15081 = FACE_BOUND ( 'NONE', #19410, .T. ) ;
#15082 = ORIENTED_EDGE ( 'NONE', *, *, #39800, .F. ) ;
#15083 = CIRCLE ( 'NONE', #19782, 16.00000000000000000 ) ;
#15084 = ORIENTED_EDGE ( 'NONE', *, *, #43315, .T. ) ;
#15085 = VERTEX_POINT ( 'NONE', #25158 ) ;
#15086 = LINE ( 'NONE', #37355, #11490 ) ;
#15087 = ORIENTED_EDGE ( 'NONE', *, *, #8622, .F. ) ;
#15088 = EDGE_CURVE ( 'NONE', #32597, #17971, #40109, .T. ) ;
#15089 = CARTESIAN_POINT ( 'NONE',  ( 0.000000000000000000, 39.47590169984846398, 71.87247863392427405 ) ) ;
#15090 = DIRECTION ( 'NONE',  ( 0.000000000000000000, 0.000000000000000000, 1.000000000000000000 ) ) ;
#15091 = DIRECTION ( 'NONE',  ( 0.000000000000000000, 0.000000000000000000, -1.000000000000000000 ) ) ;
#15092 = DIRECTION ( 'NONE',  ( -1.000000000000000000, -0.000000000000000000, 0.000000000000000000 ) ) ;
#15093 = CARTESIAN_POINT ( 'NONE',  ( 0.000000000000000000, 8.840884882376133902, -74.65374052328640175 ) ) ;
#15094 = EDGE_CURVE ( 'NONE', #25837, #17873, #41318, .T. ) ;
#15095 = CARTESIAN_POINT ( 'NONE',  ( 0.000000000000000000, -0.8299999999999999600, -1.199999999999999956 ) ) ;
#15096 = DIRECTION ( 'NONE',  ( -0.000000000000000000, -0.000000000000000000, -1.000000000000000000 ) ) ;
#15097 = DIRECTION ( 'NONE',  ( 0.000000000000000000, 0.000000000000000000, 1.000000000000000000 ) ) ;
#15098 = LINE ( 'NONE', #7748, #48035 ) ;
#15099 = VERTEX_POINT ( 'NONE', #44732 ) ;
#15100 = DIRECTION ( 'NONE',  ( -1.000000000000000000, 0.000000000000000000, 0.000000000000000000 ) ) ;
#15101 = ORIENTED_EDGE ( 'NONE', *, *, #25334, .F. ) ;
#15103 = EDGE_CURVE ( 'NONE', #18715, #23803, #18322, .T. ) ;
#15102 = DIRECTION ( 'NONE',  ( 0.000000000000000000, 0.000000000000000000, 1.000000000000000000 ) ) ;
#15104 = EDGE_LOOP ( 'NONE', ( #28413, #9823, #27498, #35107 ) ) ;
#15105 = CARTESIAN_POINT ( 'NONE',  ( 2.500000000000000000, 16.00000000000000000, -19.01812422950394676 ) ) ;
#15106 = EDGE_CURVE ( 'NONE', #20488, #35390, #24590, .T. ) ;
#15107 = DIRECTION ( 'NONE',  ( -1.000000000000000000, -0.000000000000000000, -0.000000000000000000 ) ) ;
#15108 = AXIS2_PLACEMENT_3D ( 'NONE', #23785, #8600, #45837 ) ;
#15109 = CARTESIAN_POINT ( 'NONE',  ( 0.000000000000000000, 0.000000000000000000, 125.0000000000000000 ) ) ;
#15110 =( NAMED_UNIT ( * ) SI_UNIT ( $, .STERADIAN. ) SOLID_ANGLE_UNIT ( ) );
#15112 = VECTOR ( 'NONE', #7406, 1000.000000000000000 ) ;
#15111 = CARTESIAN_POINT ( 'NONE',  ( 25.81725066941077529, -113.8380548628854854, -2.500000000000000444 ) ) ;
#15113 = FACE_OUTER_BOUND ( 'NONE', #18735, .T. ) ;
#15114 = CYLINDRICAL_SURFACE ( 'NONE', #7351, 31.99999999999998579 ) ;
#15115 = ORIENTED_EDGE ( 'NONE', *, *, #43894, .F. ) ;
#15116 = CIRCLE ( 'NONE', #31551, 37.49900000000000944 ) ;
#15117 = VECTOR ( 'NONE', #29641, 1000.000000000000000 ) ;
#15118 = ADVANCED_FACE ( 'NONE', ( #35100 ), #671, .T. ) ;
#15119 = VECTOR ( 'NONE', #26100, 1000.000000000000000 ) ;
#15120 = DIRECTION ( 'NONE',  ( -1.000000000000000000, -0.000000000000000000, 0.000000000000000000 ) ) ;
#15121 =( NAMED_UNIT ( * ) PLANE_ANGLE_UNIT ( ) SI_UNIT ( $, .RADIAN. ) );
#15122 = VECTOR ( 'NONE', #7756, 1000.000000000000000 ) ;
#15123 = CARTESIAN_POINT ( 'NONE',  ( 10.00000000000000000, 35.47612816024556537, -22.48208911017461631 ) ) ;
#15124 = ORIENTED_EDGE ( 'NONE', *, *, #33262, .T. ) ;
#15125 = VERTEX_POINT ( 'NONE', #15603 ) ;
#15126 = AXIS2_PLACEMENT_3D ( 'NONE', #9627, #39517, #13317 ) ;
#15127 = VECTOR ( 'NONE', #29971, 1000.000000000000000 ) ;
#15128 = VERTEX_POINT ( 'NONE', #16509 ) ;
#15129 = LINE ( 'NONE', #30307, #6218 ) ;
#15130 = DIRECTION ( 'NONE',  ( 0.000000000000000000, 0.000000000000000000, 1.000000000000000000 ) ) ;
#15131 = ORIENTED_EDGE ( 'NONE', *, *, #46007, .T. ) ;
#15132 = AXIS2_PLACEMENT_3D ( 'NONE', #16761, #27787, #13561 ) ;
#15133 = EDGE_CURVE ( 'NONE', #41271, #29872, #30823, .T. ) ;
#15134 = CYLINDRICAL_SURFACE ( 'NONE', #4627, 32.00000000000000000 ) ;
#15135 = ADVANCED_FACE ( 'NONE', ( #26865 ), #41804, .T. ) ;
#15136 = ORIENTED_EDGE ( 'NONE', *, *, #43617, .F. ) ;
#15137 = ORIENTED_EDGE ( 'NONE', *, *, #22093, .F. ) ;
#15138 = EDGE_CURVE ( 'NONE', #46278, #36861, #11211, .T. ) ;
#15139 = VECTOR ( 'NONE', #31820, 1000.000000000000000 ) ;
#15140 = PLANE ( 'NONE',  #2249 ) ;
#15142 = ORIENTED_EDGE ( 'NONE', *, *, #1332, .T. ) ;
#15141 = CARTESIAN_POINT ( 'NONE',  ( 12.00000000000000000, -23.29833615347104470, 3.418703333116808629 ) ) ;
#15143 = FACE_OUTER_BOUND ( 'NONE', #18923, .T. ) ;
#15144 = VERTEX_POINT ( 'NONE', #432 ) ;
#15145 = DIRECTION ( 'NONE',  ( 0.000000000000000000, 0.9969173337331276308, 0.07845909572784873220 ) ) ;
#15146 = ORIENTED_EDGE ( 'NONE', *, *, #12385, .F. ) ;
#15147 = ORIENTED_EDGE ( 'NONE', *, *, #11115, .T. ) ;
#15148 = DIRECTION ( 'NONE',  ( -1.000000000000000000, -0.000000000000000000, 0.000000000000000000 ) ) ;
#15149 = AXIS2_PLACEMENT_3D ( 'NONE', #9330, #31878, #47020 ) ;
#15150 = DIRECTION ( 'NONE',  ( -1.000000000000000000, -0.000000000000000000, -0.000000000000000000 ) ) ;
#15151 = ADVANCED_FACE ( 'NONE', ( #11692 ), #18776, .T. ) ;
#15152 = CARTESIAN_POINT ( 'NONE',  ( 10.00000000000000000, 12.26510123303308752, -35.53030884539072787 ) ) ;
#15153 = EDGE_LOOP ( 'NONE', ( #34103, #2195, #668, #32708 ) ) ;
#15154 = EDGE_CURVE ( 'NONE', #8878, #18839, #5018, .T. ) ;
#15155 = EDGE_CURVE ( 'NONE', #23903, #7237, #41086, .T. ) ;
#15156 = ORIENTED_EDGE ( 'NONE', *, *, #33378, .T. ) ;
#15157 = CARTESIAN_POINT ( 'NONE',  ( 13.83832728059186046, -142.6495187161941089, -5.500000000000000000 ) ) ;
#15158 = LINE ( 'NONE', #21993, #13374 ) ;
#15159 = AXIS2_PLACEMENT_3D ( 'NONE', #33053, #36958, #3433 ) ;
#15160 = AXIS2_PLACEMENT_3D ( 'NONE', #36765, #2996, #18154 ) ;
#15161 = ORIENTED_EDGE ( 'NONE', *, *, #37646, .F. ) ;
#15162 = VERTEX_POINT ( 'NONE', #4363 ) ;
#15163 = VECTOR ( 'NONE', #23285, 1000.000000000000000 ) ;
#15164 = CARTESIAN_POINT ( 'NONE',  ( 11.99999999999999822, -8.840884882374576037, -74.65374052328658649 ) ) ;
#15165 = ORIENTED_EDGE ( 'NONE', *, *, #30528, .F. ) ;
#15166 = AXIS2_PLACEMENT_3D ( 'NONE', #23004, #4168, #19082 ) ;
#15167 = CARTESIAN_POINT ( 'NONE',  ( 10.00000000000000000, 0.000000000000000000, 0.000000000000000000 ) ) ;
#15168 = DIRECTION ( 'NONE',  ( 0.000000000000000000, 0.9238795325112851842, 0.3826834323650938341 ) ) ;
#15169 = DIRECTION ( 'NONE',  ( -1.000000000000000000, 0.000000000000000000, 0.000000000000000000 ) ) ;
#15170 = DIRECTION ( 'NONE',  ( -0.5200609990132993854, -0.8541291221503275466, 0.000000000000000000 ) ) ;
#15171 = PLANE ( 'NONE',  #12708 ) ;
#15172 = DIRECTION ( 'NONE',  ( 0.000000000000000000, 0.000000000000000000, 1.000000000000000000 ) ) ;
#15173 = CIRCLE ( 'NONE', #34672, 77.49899999999999523 ) ;
#15174 = CARTESIAN_POINT ( 'NONE',  ( -12.00000000000000000, 0.000000000000000000, 0.000000000000000000 ) ) ;
#15175 = LINE ( 'NONE', #30101, #16925 ) ;
#15176 = CARTESIAN_POINT ( 'NONE',  ( 10.00000000000000000, 37.16516213103277977, 4.992566952385115719 ) ) ;
#15177 = DIRECTION ( 'NONE',  ( 0.000000000000000000, 0.000000000000000000, 1.000000000000000000 ) ) ;
#15178 = CYLINDRICAL_SURFACE ( 'NONE', #26192, 31.99999999999998579 ) ;
#15179 =( NAMED_UNIT ( * ) SI_UNIT ( $, .STERADIAN. ) SOLID_ANGLE_UNIT ( ) );
#15180 = PLANE ( 'NONE',  #39711 ) ;
#15181 = AXIS2_PLACEMENT_3D ( 'NONE', #40814, #29557, #2886 ) ;
#15182 = ORIENTED_EDGE ( 'NONE', *, *, #23272, .T. ) ;
#15183 = AXIS2_PLACEMENT_3D ( 'NONE', #46825, #20375, #9134 ) ;
#15184 = CARTESIAN_POINT ( 'NONE',  ( 0.000000000000000000, 0.000000000000000000, 0.000000000000000000 ) ) ;
#15185 = VECTOR ( 'NONE', #42917, 1000.000000000000000 ) ;
#15186 = VECTOR ( 'NONE', #20951, 1000.000000000000000 ) ;
#15187 = DIRECTION ( 'NONE',  ( -1.000000000000000000, -0.000000000000000000, -0.000000000000000000 ) ) ;
#15188 = DIRECTION ( 'NONE',  ( -0.000000000000000000, -0.000000000000000000, -1.000000000000000000 ) ) ;
#15189 = ORIENTED_EDGE ( 'NONE', *, *, #22707, .F. ) ;
#15190 = EDGE_LOOP ( 'NONE', ( #35102, #31503, #29389, #28518 ) ) ;
#15191 = EDGE_CURVE ( 'NONE', #13412, #44059, #4589, .T. ) ;
#15192 = CIRCLE ( 'NONE', #23780, 42.00000000000000000 ) ;
#15193 = CIRCLE ( 'NONE', #40172, 31.99999999999998579 ) ;
#15194 = LINE ( 'NONE', #22528, #18764 ) ;
#15195 = CIRCLE ( 'NONE', #333, 82.00000000000000000 ) ;
#15196 = VERTEX_POINT ( 'NONE', #37882 ) ;
#15197 = EDGE_CURVE ( 'NONE', #31943, #25264, #30045, .T. ) ;
#15198 = ORIENTED_EDGE ( 'NONE', *, *, #2359, .T. ) ;
#15199 = ORIENTED_EDGE ( 'NONE', *, *, #9033, .F. ) ;
#15200 = VERTEX_POINT ( 'NONE', #37636 ) ;
#15201 = CARTESIAN_POINT ( 'NONE',  ( 11.99999999999999822, 0.000000000000000000, 0.000000000000000000 ) ) ;
#15202 = EDGE_CURVE ( 'NONE', #59, #40154, #15195, .T. ) ;
#15203 = VECTOR ( 'NONE', #16383, 1000.000000000000000 ) ;
#15204 = FACE_OUTER_BOUND ( 'NONE', #31975, .T. ) ;
#15205 = EDGE_LOOP ( 'NONE', ( #24835, #8700, #5461, #206 ) ) ;
#15206 = ORIENTED_EDGE ( 'NONE', *, *, #34197, .F. ) ;
#15207 = DIRECTION ( 'NONE',  ( 0.000000000000000000, -0.8090169943749401238, -0.5877852522924831291 ) ) ;
#15208 = EDGE_LOOP ( 'NONE', ( #30003, #35653, #21075, #31037 ) ) ;
#15209 = CIRCLE ( 'NONE', #21450, 16.00000000000000000 ) ;
#15210 = CARTESIAN_POINT ( 'NONE',  ( 10.00000000000000000, -32.34446384429951138, -26.79245525562750530 ) ) ;
#15211 = DIRECTION ( 'NONE',  ( 0.000000000000000000, 0.000000000000000000, 1.000000000000000000 ) ) ;
#15212 = VERTEX_POINT ( 'NONE', #7286 ) ;
#15213 = EDGE_CURVE ( 'NONE', #925, #20327, #42561, .T. ) ;
#15214 = LINE ( 'NONE', #29413, #35439 ) ;
#15215 = CARTESIAN_POINT ( 'NONE',  ( 0.000000000000000000, 0.000000000000000000, 0.000000000000000000 ) ) ;
#15216 = EDGE_CURVE ( 'NONE', #33075, #40440, #27713, .T. ) ;
#15217 = ORIENTED_EDGE ( 'NONE', *, *, #33526, .F. ) ;
#15219 = EDGE_LOOP ( 'NONE', ( #34605, #25723, #9451, #33899, #9635, #20141 ) ) ;
#15218 = LINE ( 'NONE', #15453, #42229 ) ;
#15220 = AXIS2_PLACEMENT_3D ( 'NONE', #43574, #6132, #21537 ) ;
#15221 = PLANE ( 'NONE',  #14140 ) ;
#15222 = ORIENTED_EDGE ( 'NONE', *, *, #21808, .F. ) ;
#15223 = FACE_OUTER_BOUND ( 'NONE', #1174, .T. ) ;
#15224 = VERTEX_POINT ( 'NONE', #18551 ) ;
#15225 = CARTESIAN_POINT ( 'NONE',  ( 10.00000000000000000, -30.84782396557201878, -21.32104025579148399 ) ) ;
#15226 = VECTOR ( 'NONE', #39782, 1000.000000000000000 ) ;
#15227 = CARTESIAN_POINT ( 'NONE',  ( 10.00000000000000000, -75.11725578898470701, 2.956366410620372864 ) ) ;
#15228 = AXIS2_PLACEMENT_3D ( 'NONE', #32159, #12834, #47077 ) ;
#15229 = CARTESIAN_POINT ( 'NONE',  ( 10.00000000000000000, 26.08949754953062694, -27.05870788708203989 ) ) ;
#15230 = DIRECTION ( 'NONE',  ( -1.000000000000000000, 0.000000000000000000, -0.000000000000000000 ) ) ;
#15231 = CARTESIAN_POINT ( 'NONE',  ( 10.00000000000000000, 29.81001611431009479, 22.74946021919143391 ) ) ;
#15232 = CARTESIAN_POINT ( 'NONE',  ( 11.99999999999999822, -76.66974797899830207, -11.30684508768420571 ) ) ;
#15233 = CARTESIAN_POINT ( 'NONE',  ( 12.00000000000000000, 16.83928648764922542, -16.46020748918050458 ) ) ;
#15234 = ADVANCED_FACE ( 'NONE', ( #7771 ), #48403, .T. ) ;
#15235 = CARTESIAN_POINT ( 'NONE',  ( 0.000000000000000000, -23.29833615347109443, 3.418703333116492438 ) ) ;
#15236 = CIRCLE ( 'NONE', #33967, 77.49900000000000944 ) ;
#15237 = CARTESIAN_POINT ( 'NONE',  ( 0.000000000000000000, -28.89263327155796901, 71.91182617369176455 ) ) ;
#15238 = DIRECTION ( 'NONE',  ( 0.000000000000000000, -0.9876883405951358830, -0.1564344650402420822 ) ) ;
#15239 = CARTESIAN_POINT ( 'NONE',  ( 11.99999999999999822, -46.54456581323762521, -59.03342792756313884 ) ) ;
#15241 = AXIS2_PLACEMENT_3D ( 'NONE', #35920, #5594, #17311 ) ;
#15240 = DIRECTION ( 'NONE',  ( -1.000000000000000000, 0.000000000000000000, -0.000000000000000000 ) ) ;
#15242 = AXIS2_PLACEMENT_3D ( 'NONE', #43898, #29687, #47555 ) ;
#15243 = CIRCLE ( 'NONE', #44153, 77.49900000000000944 ) ;
#15244 = LINE ( 'NONE', #41191, #23658 ) ;
#15245 = DIRECTION ( 'NONE',  ( 0.000000000000000000, -0.000000000000000000, 1.000000000000000000 ) ) ;
#15246 = DIRECTION ( 'NONE',  ( -1.000000000000000000, 0.000000000000000000, -0.000000000000000000 ) ) ;
#15247 = LINE ( 'NONE', #41421, #24912 ) ;
#15248 = CIRCLE ( 'NONE', #372, 0.2999999999999981570 ) ;
#15249 = VERTEX_POINT ( 'NONE', #27781 ) ;
#15250 = VERTEX_POINT ( 'NONE', #47089 ) ;
#15251 = CARTESIAN_POINT ( 'NONE',  ( 11.99999999999999822, 0.000000000000000000, 0.000000000000000000 ) ) ;
#15252 = ORIENTED_EDGE ( 'NONE', *, *, #12334, .F. ) ;
#15253 = LINE ( 'NONE', #11084, #4129 ) ;
#15254 = DIRECTION ( 'NONE',  ( -2.991080821941227764E-16, -1.441094914046774813E-15, 0.9999999999999998890 ) ) ;
#15255 = CARTESIAN_POINT ( 'NONE',  ( 11.99999999999999822, 44.88180994100466847, -63.18004540532978552 ) ) ;
#15256 = ORIENTED_EDGE ( 'NONE', *, *, #46092, .T. ) ;
#15257 = CIRCLE ( 'NONE', #20694, 31.99999999999999289 ) ;
#15258 = AXIS2_PLACEMENT_3D ( 'NONE', #5701, #24546, #39234 ) ;
#15259 = CARTESIAN_POINT ( 'NONE',  ( 9.984461079971730157, -95.40710393340120277, 5.500000000000000000 ) ) ;
#15260 = EDGE_CURVE ( 'NONE', #38600, #14299, #19893, .T. ) ;
#15261 = VERTEX_POINT ( 'NONE', #28731 ) ;
#15262 = ADVANCED_FACE ( 'NONE', ( #36313 ), #17457, .T. ) ;
#15263 = AXIS2_PLACEMENT_3D ( 'NONE', #17943, #47802, #44150 ) ;
#15264 = VECTOR ( 'NONE', #40520, 1000.000000000000000 ) ;
#15265 = DIRECTION ( 'NONE',  ( 0.7533909544171996098, 0.6575728627325955200, -7.625282249115660656E-32 ) ) ;
#15266 = EDGE_CURVE ( 'NONE', #17111, #15663, #6455, .T. ) ;
#15267 = CARTESIAN_POINT ( 'NONE',  ( 0.000000000000000000, 18.84667830672579925, 18.68964196561269020 ) ) ;
#15269 = EDGE_LOOP ( 'NONE', ( #3763, #22990, #7493 ) ) ;
#15268 = LINE ( 'NONE', #30199, #12168 ) ;
#15270 = ORIENTED_EDGE ( 'NONE', *, *, #7017, .T. ) ;
#15271 = AXIS2_PLACEMENT_3D ( 'NONE', #7318, #29361, #21997 ) ;
#15272 = VECTOR ( 'NONE', #43457, 1000.000000000000000 ) ;
#15273 = AXIS2_PLACEMENT_3D ( 'NONE', #23999, #1718, #9778 ) ;
#15274 = FACE_OUTER_BOUND ( 'NONE', #24425, .T. ) ;
#15275 = CYLINDRICAL_SURFACE ( 'NONE', #29610, 77.49899999999999523 ) ;
#15276 = EDGE_CURVE ( 'NONE', #39764, #14287, #12900, .T. ) ;
#15277 = CARTESIAN_POINT ( 'NONE',  ( 11.99999999999999822, -71.27951684758005513, -30.41916302227188851 ) ) ;
#15278 = CARTESIAN_POINT ( 'NONE',  ( 11.99999999999999822, 54.21277698773675979, 55.38113227695801299 ) ) ;
#15279 = VERTEX_POINT ( 'NONE', #35342 ) ;
#15280 = LINE ( 'NONE', #30210, #46714 ) ;
#15281 = EDGE_LOOP ( 'NONE', ( #35708, #3642, #33351, #8935 ) ) ;
#15282 = ORIENTED_EDGE ( 'NONE', *, *, #34142, .F. ) ;
#15283 = EDGE_CURVE ( 'NONE', #13717, #23918, #5068, .T. ) ;
#15284 = DIRECTION ( 'NONE',  ( -0.000000000000000000, -1.000000000000000000, -0.000000000000000000 ) ) ;
#15285 = DIRECTION ( 'NONE',  ( 0.000000000000000000, 0.000000000000000000, 1.000000000000000000 ) ) ;
#15286 = CIRCLE ( 'NONE', #42645, 77.49899999999999523 ) ;
#15287 = CARTESIAN_POINT ( 'NONE',  ( 10.00000000000000000, 0.000000000000000000, 0.000000000000000000 ) ) ;
#15288 = CARTESIAN_POINT ( 'NONE',  ( 10.00000000000000000, 0.000000000000000000, 0.000000000000000000 ) ) ;
#15289 = VERTEX_POINT ( 'NONE', #43658 ) ;
#15290 = FACE_OUTER_BOUND ( 'NONE', #29027, .T. ) ;
#15291 = DIRECTION ( 'NONE',  ( 0.000000000000000000, 0.4539904997395479702, -0.8910065241883673437 ) ) ;
#15292 = CYLINDRICAL_SURFACE ( 'NONE', #9436, 31.99999999999998579 ) ;
#15293 = DIRECTION ( 'NONE',  ( 1.000000000000000000, 0.000000000000000000, 0.000000000000000000 ) ) ;
#15294 = EDGE_CURVE ( 'NONE', #21018, #3559, #12781, .T. ) ;
#15295 = VECTOR ( 'NONE', #46111, 1000.000000000000000 ) ;
#15296 = DIRECTION ( 'NONE',  ( -0.7950889364178798102, 0.6064928550163511956, 0.000000000000000000 ) ) ;
#15297 = DIRECTION ( 'NONE',  ( 0.000000000000000000, 0.000000000000000000, -1.000000000000000000 ) ) ;
#15298 = CARTESIAN_POINT ( 'NONE',  ( -10.00000000000000000, 0.000000000000000000, 0.000000000000000000 ) ) ;
#15299 = CARTESIAN_POINT ( 'NONE',  ( 5.000000000000000000, 33.71516098798740302, 74.74816331893443078 ) ) ;
#15300 = DIRECTION ( 'NONE',  ( 0.000000000000000000, 0.000000000000000000, 1.000000000000000000 ) ) ;
#15301 = CYLINDRICAL_SURFACE ( 'NONE', #47192, 77.49899999999999523 ) ;
#15302 = CARTESIAN_POINT ( 'NONE',  ( 10.00000000000000000, -16.23288003029521320, 33.80338159004277543 ) ) ;
#15303 = ADVANCED_FACE ( 'NONE', ( #25044 ), #20909, .T. ) ;
#15304 = AXIS2_PLACEMENT_3D ( 'NONE', #12319, #23552, #4957 ) ;
#15305 = CARTESIAN_POINT ( 'NONE',  ( 10.00000000000000000, 55.19960302592141232, -51.03279382321027668 ) ) ;
#15306 = CARTESIAN_POINT ( 'NONE',  ( 10.00000000000000000, -34.94270380257586339, -74.18225833017926618 ) ) ;
#15307 = DIRECTION ( 'NONE',  ( 0.000000000000000000, 0.000000000000000000, 1.000000000000000000 ) ) ;
#15308 = ORIENTED_EDGE ( 'NONE', *, *, #16904, .F. ) ;
#15309 = DIRECTION ( 'NONE',  ( 1.000000000000000000, 0.000000000000000000, 0.000000000000000000 ) ) ;
#15310 = AXIS2_PLACEMENT_3D ( 'NONE', #19405, #1549, #15511 ) ;
#15311 = ORIENTED_EDGE ( 'NONE', *, *, #27739, .F. ) ;
#15312 = ORIENTED_EDGE ( 'NONE', *, *, #8337, .T. ) ;
#15313 = ADVANCED_FACE ( 'NONE', ( #42703 ), #13556, .T. ) ;
#15314 = ORIENTED_EDGE ( 'NONE', *, *, #24919, .T. ) ;
#15315 = EDGE_CURVE ( 'NONE', #6863, #32670, #19017, .T. ) ;
#15316 = CIRCLE ( 'NONE', #19210, 31.99999999999998934 ) ;
#15317 = ORIENTED_EDGE ( 'NONE', *, *, #37290, .F. ) ;
#15318 = PLANE ( 'NONE',  #28898 ) ;
#15319 = AXIS2_PLACEMENT_3D ( 'NONE', #12798, #42166, #13049 ) ;
#15320 = ORIENTED_EDGE ( 'NONE', *, *, #47188, .F. ) ;
#15321 = ADVANCED_FACE ( 'NONE', ( #24329 ), #36066, .T. ) ;
#15322 = AXIS2_PLACEMENT_3D ( 'NONE', #2990, #44118, #37001 ) ;
#15323 = CARTESIAN_POINT ( 'NONE',  ( -11.59999999999999787, 0.000000000000000000, 42.00000000000001421 ) ) ;
#15324 = EDGE_CURVE ( 'NONE', #8980, #1474, #17445, .T. ) ;
#15325 = EDGE_CURVE ( 'NONE', #26495, #25548, #32635, .T. ) ;
#15326 = CARTESIAN_POINT ( 'NONE',  ( 15.00000000000000000, -25.60904388321925040, -6.976881207771165272 ) ) ;
#15327 = FACE_OUTER_BOUND ( 'NONE', #23350, .T. ) ;
#15328 = ORIENTED_EDGE ( 'NONE', *, *, #28534, .T. ) ;
#15329 = CARTESIAN_POINT ( 'NONE',  ( 10.00000000000000000, -33.80338159004296017, 16.23288003029484727 ) ) ;
#15330 = ORIENTED_EDGE ( 'NONE', *, *, #29006, .T. ) ;
#15331 = VERTEX_POINT ( 'NONE', #12843 ) ;
#15332 = AXIS2_PLACEMENT_3D ( 'NONE', #1128, #26362, #11673 ) ;
#15333 = ORIENTED_EDGE ( 'NONE', *, *, #18228, .F. ) ;
#15334 = PLANE ( 'NONE',  #19373 ) ;
#15335 = CARTESIAN_POINT ( 'NONE',  ( 11.99999999999999822, -68.26794271651286294, 31.47745569255117104 ) ) ;
#15336 = DIRECTION ( 'NONE',  ( -0.5200609990132993854, -0.8541291221503275466, 0.000000000000000000 ) ) ;
#15337 = CIRCLE ( 'NONE', #19228, 16.00000000000000000 ) ;
#15338 = VERTEX_POINT ( 'NONE', #35829 ) ;
#15339 = EDGE_LOOP ( 'NONE', ( #2207, #22034, #2412, #27564 ) ) ;
#15340 = DIRECTION ( 'NONE',  ( 0.000000000000000000, 0.000000000000000000, 1.000000000000000000 ) ) ;
#15341 = ORIENTED_EDGE ( 'NONE', *, *, #35882, .F. ) ;
#15342 = CARTESIAN_POINT ( 'NONE',  ( 0.000000000000000000, 0.000000000000000000, 0.000000000000000000 ) ) ;
#15343 = VECTOR ( 'NONE', #9864, 1000.000000000000000 ) ;
#15344 = CARTESIAN_POINT ( 'NONE',  ( 10.00000000000000000, -27.13269053701114331, 25.88420570971391754 ) ) ;
#15345 = FACE_OUTER_BOUND ( 'NONE', #41057, .T. ) ;
#15346 = FACE_OUTER_BOUND ( 'NONE', #10192, .T. ) ;
#15347 = DIRECTION ( 'NONE',  ( 0.000000000000000000, 0.000000000000000000, 1.000000000000000000 ) ) ;
#15348 = DIRECTION ( 'NONE',  ( 1.000000000000000000, 0.000000000000000000, 0.000000000000000000 ) ) ;
#15349 = CIRCLE ( 'NONE', #27752, 16.00000000000000000 ) ;
#15350 = CARTESIAN_POINT ( 'NONE',  ( 10.00000000000000000, 73.44644590900061587, 24.73286445877730699 ) ) ;
#15351 = CARTESIAN_POINT ( 'NONE',  ( 5.000000000000002665, 39.47590169984944453, -71.87247863392373404 ) ) ;
#15352 = LINE ( 'NONE', #25850, #25344 ) ;
#15353 = EDGE_LOOP ( 'NONE', ( #34220, #41108 ) ) ;
#15354 = DIRECTION ( 'NONE',  ( 0.000000000000000000, -0.8090169943749531134, 0.5877852522924653655 ) ) ;
#15355 = EDGE_CURVE ( 'NONE', #18078, #8218, #13083, .T. ) ;
#15356 = ORIENTED_EDGE ( 'NONE', *, *, #47765, .F. ) ;
#15357 = ORIENTED_EDGE ( 'NONE', *, *, #31214, .F. ) ;
#15358 = CARTESIAN_POINT ( 'NONE',  ( 10.00000000000000000, -59.03342792756297541, 46.54456581323783126 ) ) ;
#15359 = CARTESIAN_POINT ( 'NONE',  ( 0.000000000000000000, 0.000000000000000000, -56.19999999999998863 ) ) ;
#15360 = AXIS2_PLACEMENT_3D ( 'NONE', #40685, #25255, #7155 ) ;
#15361 = DIRECTION ( 'NONE',  ( -1.000000000000000000, -0.000000000000000000, 0.000000000000000000 ) ) ;
#15362 = CARTESIAN_POINT ( 'NONE',  ( 11.99999999999999822, -65.58780272294100655, 36.73666225445870737 ) ) ;
#15363 = ADVANCED_FACE ( 'NONE', ( #5734 ), #2073, .T. ) ;
#15364 = AXIS2_PLACEMENT_3D ( 'NONE', #41628, #40912, #11045 ) ;
#15365 = DIRECTION ( 'NONE',  ( -0.000000000000000000, 0.8090169943749498938, -0.5877852522924696954 ) ) ;
#15366 = CARTESIAN_POINT ( 'NONE',  ( 19.12409105625795291, -101.5943176906707919, 5.500000000000000000 ) ) ;
#15367 = AXIS2_PLACEMENT_3D ( 'NONE', #36699, #18093, #43580 ) ;
#15368 = DIRECTION ( 'NONE',  ( -1.000000000000000000, -0.000000000000000000, -0.000000000000000000 ) ) ;
#15369 = CARTESIAN_POINT ( 'NONE',  ( 30.50000000000000000, -120.0000000000000000, -2.500000000000000000 ) ) ;
#15370 = FACE_OUTER_BOUND ( 'NONE', #13708, .T. ) ;
#15371 =( NAMED_UNIT ( * ) PLANE_ANGLE_UNIT ( ) SI_UNIT ( $, .RADIAN. ) );
#15372 = CARTESIAN_POINT ( 'NONE',  ( -26.29030328629083968, -123.6496510949466341, 2.500000000000000000 ) ) ;
#15373 = VERTEX_POINT ( 'NONE', #28245 ) ;
#15374 = AXIS2_PLACEMENT_3D ( 'NONE', #24888, #39606, #2365 ) ;
#15375 = EDGE_CURVE ( 'NONE', #22938, #28248, #31671, .T. ) ;
#15376 = VERTEX_POINT ( 'NONE', #3248 ) ;
#15377 = AXIS2_PLACEMENT_3D ( 'NONE', #31129, #41906, #27449 ) ;
#15378 = FACE_OUTER_BOUND ( 'NONE', #15205, .T. ) ;
#15379 = EDGE_CURVE ( 'NONE', #21856, #38600, #25265, .T. ) ;
#15380 = DIRECTION ( 'NONE',  ( 0.9966891607226786576, 0.08130631524009862554, 0.000000000000000000 ) ) ;
#15381 = EDGE_LOOP ( 'NONE', ( #37515, #7791, #8471, #20423 ) ) ;
#15382 = AXIS2_PLACEMENT_3D ( 'NONE', #22981, #3157, #18085 ) ;
#15383 = ADVANCED_FACE ( 'NONE', ( #36550 ), #17935, .T. ) ;
#15384 = LINE ( 'NONE', #8010, #41361 ) ;
#15385 = ORIENTED_EDGE ( 'NONE', *, *, #6209, .F. ) ;
#15386 = ADVANCED_FACE ( 'NONE', ( #37029 ), #40702, .T. ) ;
#15387 = ORIENTED_EDGE ( 'NONE', *, *, #43165, .F. ) ;
#15388 = AXIS2_PLACEMENT_3D ( 'NONE', #38341, #15365, #27333 ) ;
#15389 = DIRECTION ( 'NONE',  ( -1.000000000000000000, 0.000000000000000000, 0.000000000000000000 ) ) ;
#15390 = FACE_OUTER_BOUND ( 'NONE', #7104, .T. ) ;
#15391 = VECTOR ( 'NONE', #42815, 1000.000000000000000 ) ;
#15392 = DIRECTION ( 'NONE',  ( 0.000000000000000000, 0.000000000000000000, 1.000000000000000000 ) ) ;
#15393 = ORIENTED_EDGE ( 'NONE', *, *, #42872, .F. ) ;
#15394 = CARTESIAN_POINT ( 'NONE',  ( 10.00000000000000000, 72.35432306680455383, 20.40083707023012494 ) ) ;
#15395 = EDGE_LOOP ( 'NONE', ( #17992, #15333, #32931, #22658 ) ) ;
#15396 = DIRECTION ( 'NONE',  ( -1.000000000000000000, 0.000000000000000000, -0.000000000000000000 ) ) ;
#15397 = FACE_OUTER_BOUND ( 'NONE', #314, .T. ) ;
#15398 = CARTESIAN_POINT ( 'NONE',  ( 11.99999999999999822, 8.966570791701867549, -81.50828551894218776 ) ) ;
#15399 = ORIENTED_EDGE ( 'NONE', *, *, #48335, .T. ) ;
#15400 = EDGE_LOOP ( 'NONE', ( #6987, #21239, #14245, #18727 ) ) ;
#15401 = SURFACE_SIDE_STYLE ('',( #4134 ) ) ;
#15402 = CARTESIAN_POINT ( 'NONE',  ( 0.000000000000000000, 0.8828120875900632436, 37.48860685352291000 ) ) ;
#15403 = CIRCLE ( 'NONE', #26330, 37.49900000000000233 ) ;
#15404 = ORIENTED_EDGE ( 'NONE', *, *, #23074, .F. ) ;
#15405 = ORIENTED_EDGE ( 'NONE', *, *, #41408, .F. ) ;
#15406 = CARTESIAN_POINT ( 'NONE',  ( 0.000000000000000000, 16.83928648764923253, 16.46020748918050458 ) ) ;
#15407 = EDGE_LOOP ( 'NONE', ( #43068, #2039, #14676, #17249 ) ) ;
#15408 = DIRECTION ( 'NONE',  ( 0.000000000000000000, 0.000000000000000000, -1.000000000000000000 ) ) ;
#15409 = CYLINDRICAL_SURFACE ( 'NONE', #4315, 16.00000000000000000 ) ;
#15410 = AXIS2_PLACEMENT_3D ( 'NONE', #17566, #9029, #38900 ) ;
#15411 = DIRECTION ( 'NONE',  ( -0.8774505977381983346, -0.4796670183876294291, 0.000000000000000000 ) ) ;
#15412 = CARTESIAN_POINT ( 'NONE',  ( 12.49999999999999645, 1.530808498934191127E-15, 125.0000000000000000 ) ) ;
#15413 = LINE ( 'NONE', #11500, #21284 ) ;
#15414 = CARTESIAN_POINT ( 'NONE',  ( 0.000000000000000000, -20.41045688087772092, -72.35160999960838524 ) ) ;
#15415 = CARTESIAN_POINT ( 'NONE',  ( 0.000000000000000000, 37.16516213103277266, 4.992566952385114831 ) ) ;
#15416 = CARTESIAN_POINT ( 'NONE',  ( 0.000000000000000000, 0.000000000000000000, 0.000000000000000000 ) ) ;
#15417 = CARTESIAN_POINT ( 'NONE',  ( 11.99999999999999822, -8.966570791700153364, -81.50828551894235829 ) ) ;
#15418 = ORIENTED_EDGE ( 'NONE', *, *, #18592, .F. ) ;
#15419 = ADVANCED_FACE ( 'NONE', ( #29929 ), #33365, .T. ) ;
#15420 = DIRECTION ( 'NONE',  ( -1.000000000000000000, 0.000000000000000000, -0.000000000000000000 ) ) ;
#15421 = FACE_OUTER_BOUND ( 'NONE', #21760, .T. ) ;
#15422 = DIRECTION ( 'NONE',  ( -1.000000000000000000, -0.000000000000000000, -0.000000000000000000 ) ) ;
#15423 = ORIENTED_EDGE ( 'NONE', *, *, #37402, .T. ) ;
#15424 = AXIS2_PLACEMENT_3D ( 'NONE', #25090, #40038, #39570 ) ;
#15425 = UNCERTAINTY_MEASURE_WITH_UNIT (LENGTH_MEASURE( 1.000000000000000082E-05 ), #4990, 'distance_accuracy_value', 'NONE');
#15426 = CARTESIAN_POINT ( 'NONE',  ( 0.000000000000000000, -78.73519480814938731, -22.90783923731713045 ) ) ;
#15427 = CARTESIAN_POINT ( 'NONE',  ( 0.000000000000000000, -78.73519480814938731, -22.90783923731713756 ) ) ;
#15428 = EDGE_CURVE ( 'NONE', #15687, #14664, #21631, .T. ) ;
#15429 = DIRECTION ( 'NONE',  ( -1.000000000000000000, -0.000000000000000000, 0.000000000000000000 ) ) ;
#15430 = ORIENTED_EDGE ( 'NONE', *, *, #34087, .T. ) ;
#15431 = EDGE_CURVE ( 'NONE', #31692, #3151, #18174, .T. ) ;
#15432 = EDGE_CURVE ( 'NONE', #32581, #6408, #42472, .T. ) ;
#15433 = CIRCLE ( 'NONE', #30290, 31.99999999999999289 ) ;
#15434 = EDGE_CURVE ( 'NONE', #6719, #37275, #23822, .T. ) ;
#15435 = CYLINDRICAL_SURFACE ( 'NONE', #29603, 16.00000000000000000 ) ;
#15436 = AXIS2_PLACEMENT_3D ( 'NONE', #16084, #7758, #23177 ) ;
#15437 = EDGE_LOOP ( 'NONE', ( #36895, #11962, #46931, #19368 ) ) ;
#15438 = ORIENTED_EDGE ( 'NONE', *, *, #29339, .F. ) ;
#15439 = EDGE_CURVE ( 'NONE', #20016, #21863, #7425, .T. ) ;
#15440 = VERTEX_POINT ( 'NONE', #33599 ) ;
#15441 = FACE_OUTER_BOUND ( 'NONE', #30834, .T. ) ;
#15442 = VECTOR ( 'NONE', #22338, 1000.000000000000000 ) ;
#15443 = VERTEX_POINT ( 'NONE', #44383 ) ;
#15444 = ORIENTED_EDGE ( 'NONE', *, *, #8079, .F. ) ;
#15445 = CYLINDRICAL_SURFACE ( 'NONE', #45446, 77.49899999999999523 ) ;
#15446 = ORIENTED_EDGE ( 'NONE', *, *, #3937, .T. ) ;
#15447 = CYLINDRICAL_SURFACE ( 'NONE', #2750, 77.49899999999999523 ) ;
#15448 = DIRECTION ( 'NONE',  ( 1.000000000000000000, 0.000000000000000000, 0.000000000000000000 ) ) ;
#15449 = ORIENTED_EDGE ( 'NONE', *, *, #39034, .T. ) ;
#15450 = CARTESIAN_POINT ( 'NONE',  ( 0.000000000000000000, 0.000000000000000000, 0.000000000000000000 ) ) ;
#15451 = ORIENTED_EDGE ( 'NONE', *, *, #15756, .T. ) ;
#15452 = AXIS2_PLACEMENT_3D ( 'NONE', #15895, #41852, #8310 ) ;
#15453 = CARTESIAN_POINT ( 'NONE',  ( 5.000000000000000000, 3.925862922256160736, 41.81611651403863306 ) ) ;
#15454 = FACE_OUTER_BOUND ( 'NONE', #48012, .T. ) ;
#15455 = VERTEX_POINT ( 'NONE', #3011 ) ;
#15456 = LINE ( 'NONE', #41401, #39695 ) ;
#15457 = ORIENTED_EDGE ( 'NONE', *, *, #16486, .T. ) ;
#15458 = EDGE_LOOP ( 'NONE', ( #26724, #30001, #19374, #38143 ) ) ;
#15459 = CARTESIAN_POINT ( 'NONE',  ( -11.59517495878806947, -96.12423995607481686, 5.500000000000000000 ) ) ;
#15460 = LINE ( 'NONE', #34517, #38687 ) ;
#15461 = VERTEX_POINT ( 'NONE', #25527 ) ;
#15462 = LINE ( 'NONE', #15942, #22305 ) ;
#15463 = DIRECTION ( 'NONE',  ( 1.000000000000000000, -0.000000000000000000, -0.000000000000000000 ) ) ;
#15464 = DIRECTION ( 'NONE',  ( -1.000000000000000000, -0.000000000000000000, -0.000000000000000000 ) ) ;
#15465 = CARTESIAN_POINT ( 'NONE',  ( 0.000000000000000000, 39.78640506895698081, -66.50666863321957578 ) ) ;
#15467 = EDGE_CURVE ( 'NONE', #45354, #7668, #18432, .T. ) ;
#15466 = CYLINDRICAL_SURFACE ( 'NONE', #26674, 77.49899999999999523 ) ;
#15468 = CARTESIAN_POINT ( 'NONE',  ( 11.99999999999999822, -77.32052557432837148, -5.256550761633681290 ) ) ;
#15469 = EDGE_CURVE ( 'NONE', #38129, #44062, #43364, .T. ) ;
#15470 = CARTESIAN_POINT ( 'NONE',  ( 12.00000000000000000, -18.13022148937262656, -15.02647892043543898 ) ) ;
#15471 = PLANE ( 'NONE',  #14674 ) ;
#15472 = FACE_OUTER_BOUND ( 'NONE', #2348, .T. ) ;
#15473 = EDGE_CURVE ( 'NONE', #3134, #35244, #41207, .T. ) ;
#15474 = CIRCLE ( 'NONE', #23320, 82.00000000000000000 ) ;
#15475 = CARTESIAN_POINT ( 'NONE',  ( 12.49999999999999645, 1.530808498934191127E-15, 40.80000000000001847 ) ) ;
#15476 = DIRECTION ( 'NONE',  ( -1.000000000000000000, 0.000000000000000000, 0.000000000000000000 ) ) ;
#15477 = CARTESIAN_POINT ( 'NONE',  ( 11.99999999999999822, 11.30684508768450769, -76.66974797899825944 ) ) ;
#15478 = CARTESIAN_POINT ( 'NONE',  ( 11.99999999999999822, 0.000000000000000000, 0.000000000000000000 ) ) ;
#15479 = EDGE_CURVE ( 'NONE', #27749, #33199, #15012, .T. ) ;
#15480 = VERTEX_POINT ( 'NONE', #3994 ) ;
#15481 = DIRECTION ( 'NONE',  ( 0.000000000000000000, 0.3090169943749482839, -0.9510565162951533091 ) ) ;
#15482 = ORIENTED_EDGE ( 'NONE', *, *, #19613, .F. ) ;
#15483 = DIRECTION ( 'NONE',  ( -1.000000000000000000, -0.000000000000000000, -0.000000000000000000 ) ) ;
#15484 = STYLED_ITEM ( 'NONE', ( #30297 ), #31571 ) ;
#15485 = CARTESIAN_POINT ( 'NONE',  ( 0.000000000000000000, 55.16347631943131802, -60.67117009219075641 ) ) ;
#15486 = ORIENTED_EDGE ( 'NONE', *, *, #48449, .F. ) ;
#15487 = EDGE_CURVE ( 'NONE', #3669, #39957, #33974, .T. ) ;
#15488 = ADVANCED_FACE ( 'NONE', ( #26010 ), #14770, .T. ) ;
#15489 = AXIS2_PLACEMENT_3D ( 'NONE', #22186, #47638, #3089 ) ;
#15490 = ORIENTED_EDGE ( 'NONE', *, *, #8723, .F. ) ;
#15491 = CARTESIAN_POINT ( 'NONE',  ( 10.00000000000000000, 17.80606268964540462, 33.00180498840053644 ) ) ;
#15492 = VERTEX_POINT ( 'NONE', #10361 ) ;
#15493 = ADVANCED_FACE ( 'NONE', ( #40240 ), #44619, .F. ) ;
#15494 = VECTOR ( 'NONE', #9302, 1000.000000000000000 ) ;
#15495 = DIRECTION ( 'NONE',  ( 0.000000000000000000, 0.000000000000000000, -1.000000000000000000 ) ) ;
#15496 = VERTEX_POINT ( 'NONE', #31154 ) ;
#15497 = DIRECTION ( 'NONE',  ( 0.000000000000000000, 0.000000000000000000, 1.000000000000000000 ) ) ;
#15499 = ORIENTED_EDGE ( 'NONE', *, *, #10643, .F. ) ;
#15498 = DIRECTION ( 'NONE',  ( 1.000000000000000000, 0.000000000000000000, -0.000000000000000000 ) ) ;
#15500 = EDGE_LOOP ( 'NONE', ( #19083, #34486, #12366, #10908 ) ) ;
#15501 = CIRCLE ( 'NONE', #1460, 31.99999999999998934 ) ;
#15502 = CIRCLE ( 'NONE', #13924, 16.00000000000000000 ) ;
#15503 = DIRECTION ( 'NONE',  ( -1.000000000000000000, -0.000000000000000000, -0.000000000000000000 ) ) ;
#15504 = LINE ( 'NONE', #45346, #13991 ) ;
#15505 = DIRECTION ( 'NONE',  ( -1.000000000000000000, 0.000000000000000000, 0.000000000000000000 ) ) ;
#15506 = DIRECTION ( 'NONE',  ( -1.000000000000000000, 0.000000000000000000, 0.000000000000000000 ) ) ;
#15507 = VERTEX_POINT ( 'NONE', #23543 ) ;
#15508 = LINE ( 'NONE', #41949, #20887 ) ;
#15509 = VERTEX_POINT ( 'NONE', #15725 ) ;
#15510 = VERTEX_POINT ( 'NONE', #4241 ) ;
#15511 = DIRECTION ( 'NONE',  ( 0.000000000000000000, 0.5877852522924684742, 0.8090169943749506709 ) ) ;
#15512 = DIRECTION ( 'NONE',  ( 0.000000000000000000, 0.000000000000000000, -1.000000000000000000 ) ) ;
#15513 = DIRECTION ( 'NONE',  ( 0.000000000000000000, 0.000000000000000000, 1.000000000000000000 ) ) ;
#15514 = CARTESIAN_POINT ( 'NONE',  ( 11.99999999999999822, 24.73286445877705475, 73.44644590900068692 ) ) ;
#15515 = ORIENTED_EDGE ( 'NONE', *, *, #31312, .T. ) ;
#15516 = DIRECTION ( 'NONE',  ( 0.1276937514489679404, 0.9918136447140103451, -0.000000000000000000 ) ) ;
#15517 = DIRECTION ( 'NONE',  ( -1.000000000000000000, -0.000000000000000000, 0.000000000000000000 ) ) ;
#15518 = DIRECTION ( 'NONE',  ( -1.000000000000000000, 0.000000000000000000, 0.000000000000000000 ) ) ;
#15519 = AXIS2_PLACEMENT_3D ( 'NONE', #2999, #18156, #18653 ) ;
#15520 = DIRECTION ( 'NONE',  ( -1.000000000000000000, 0.000000000000000000, -0.000000000000000000 ) ) ;
#15521 = CARTESIAN_POINT ( 'NONE',  ( 0.000000000000000000, -39.04073710021332744, -15.48615015657624028 ) ) ;
#15522 = EDGE_CURVE ( 'NONE', #11693, #33751, #42152, .T. ) ;
#15523 = LINE ( 'NONE', #31192, #43420 ) ;
#15524 = CARTESIAN_POINT ( 'NONE',  ( -18.24502636017238899, -100.7225776329765665, 5.500000000000000000 ) ) ;
#15525 = DIRECTION ( 'NONE',  ( -0.000000000000000000, 0.1045284632676436315, 0.9945218953682742891 ) ) ;
#15526 = ADVANCED_FACE ( 'NONE', ( #12543 ), #38483, .F. ) ;
#15527 = FACE_OUTER_BOUND ( 'NONE', #42038, .T. ) ;
#15528 = CARTESIAN_POINT ( 'NONE',  ( 0.000000000000000000, 0.000000000000000000, 0.000000000000000000 ) ) ;
#15529 = EDGE_CURVE ( 'NONE', #35660, #12921, #37090, .T. ) ;
#15530 = DIRECTION ( 'NONE',  ( 0.000000000000000000, 0.5877852522924684742, 0.8090169943749507819 ) ) ;
#15531 = CARTESIAN_POINT ( 'NONE',  ( 11.99999999999999822, -20.40083707022829174, -72.35432306680507963 ) ) ;
#15532 = FACE_OUTER_BOUND ( 'NONE', #10318, .T. ) ;
#15533 = DIRECTION ( 'NONE',  ( 0.000000000000000000, -6.982962677686266711E-15, 1.000000000000000000 ) ) ;
#15534 = ORIENTED_EDGE ( 'NONE', *, *, #48389, .T. ) ;
#15535 = AXIS2_PLACEMENT_3D ( 'NONE', #10734, #32989, #13682 ) ;
#15536 = CIRCLE ( 'NONE', #26480, 82.00000000000000000 ) ;
#15537 = DIRECTION ( 'NONE',  ( 0.000000000000000000, 0.000000000000000000, 1.000000000000000000 ) ) ;
#15538 = ORIENTED_EDGE ( 'NONE', *, *, #29933, .F. ) ;
#15539 = EDGE_CURVE ( 'NONE', #44487, #47761, #34548, .T. ) ;
#15540 = EDGE_CURVE ( 'NONE', #42650, #23818, #4949, .T. ) ;
#15541 = EDGE_CURVE ( 'NONE', #30085, #41259, #37759, .T. ) ;
#15542 = ORIENTED_EDGE ( 'NONE', *, *, #14648, .T. ) ;
#15543 = ORIENTED_EDGE ( 'NONE', *, *, #25453, .T. ) ;
#15544 = CARTESIAN_POINT ( 'NONE',  ( 10.00000000000000000, -33.79645857604501913, -16.45098606841161626 ) ) ;
#15545 = EDGE_LOOP ( 'NONE', ( #43179, #41213, #10941, #17481 ) ) ;
#15546 = ADVANCED_FACE ( 'NONE', ( #30918 ), #1290, .T. ) ;
#15547 = LINE ( 'NONE', #15323, #44912 ) ;
#15548 = LINE ( 'NONE', #4539, #37466 ) ;
#15550 = ORIENTED_EDGE ( 'NONE', *, *, #5451, .T. ) ;
#15549 = CYLINDRICAL_SURFACE ( 'NONE', #48021, 77.49899999999999523 ) ;
#15551 = VERTEX_POINT ( 'NONE', #15491 ) ;
#15552 = CARTESIAN_POINT ( 'NONE',  ( 11.99999999999999822, 70.52718814184294160, -26.02418014898236720 ) ) ;
#15553 = ORIENTED_EDGE ( 'NONE', *, *, #22397, .F. ) ;
#15554 = ORIENTED_EDGE ( 'NONE', *, *, #16234, .F. ) ;
#15555 = CYLINDRICAL_SURFACE ( 'NONE', #14702, 82.00000000000000000 ) ;
#15556 = CARTESIAN_POINT ( 'NONE',  ( 11.99999999999999822, 41.76937507738875155, -62.50329211542393892 ) ) ;
#15557 = ORIENTED_EDGE ( 'NONE', *, *, #19931, .F. ) ;
#15558 = ORIENTED_EDGE ( 'NONE', *, *, #37565, .T. ) ;
#15559 = VERTEX_POINT ( 'NONE', #26998 ) ;
#15560 = AXIS2_PLACEMENT_3D ( 'NONE', #37159, #29335, #47672 ) ;
#15561 = CYLINDRICAL_SURFACE ( 'NONE', #31813, 82.00000000000000000 ) ;
#15562 = EDGE_LOOP ( 'NONE', ( #33152, #28119, #47133, #8018 ) ) ;
#15563 = LINE ( 'NONE', #44225, #2006 ) ;
#15564 = CIRCLE ( 'NONE', #38246, 37.49900000000000944 ) ;
#15565 = LINE ( 'NONE', #12622, #40506 ) ;
#15566 = CYLINDRICAL_SURFACE ( 'NONE', #18235, 31.99999999999997868 ) ;
#15567 = CARTESIAN_POINT ( 'NONE',  ( 10.00000000000000000, -65.58780272294048075, -36.73666225445966660 ) ) ;
#15568 = DIRECTION ( 'NONE',  ( -1.000000000000000000, -0.000000000000000000, 0.000000000000000000 ) ) ;
#15569 = DIRECTION ( 'NONE',  ( 0.000000000000000000, 0.9945218953682742891, -0.1045284632676436315 ) ) ;
#15570 = CIRCLE ( 'NONE', #6176, 77.49899999999999523 ) ;
#15571 = LINE ( 'NONE', #19243, #36933 ) ;
#15572 = CYLINDRICAL_SURFACE ( 'NONE', #1676, 31.99999999999998579 ) ;
#15573 = CARTESIAN_POINT ( 'NONE',  ( 11.99999999999999822, 0.000000000000000000, 0.000000000000000000 ) ) ;
#15574 = EDGE_LOOP ( 'NONE', ( #42614, #5089, #19249, #17041 ) ) ;
#15575 = CARTESIAN_POINT ( 'NONE',  ( 0.000000000000000000, 58.39081064771751528, 50.95692526931350841 ) ) ;
#15576 = PLANE ( 'NONE',  #31705 ) ;
#15577 = ORIENTED_EDGE ( 'NONE', *, *, #9485, .T. ) ;
#15578 = EDGE_LOOP ( 'NONE', ( #26230, #24985, #26569, #13429 ) ) ;
#15579 = CARTESIAN_POINT ( 'NONE',  ( 0.000000000000000000, -74.65491531819111515, 23.16904090965678975 ) ) ;
#15580 = ADVANCED_FACE ( 'NONE', ( #16224 ), #45844, .T. ) ;
#15581 = LINE ( 'NONE', #45934, #10543 ) ;
#15582 = DIRECTION ( 'NONE',  ( 0.000000000000000000, 0.000000000000000000, 1.000000000000000000 ) ) ;
#15583 = DIRECTION ( 'NONE',  ( -1.000000000000000000, 0.000000000000000000, -0.000000000000000000 ) ) ;
#15584 = EDGE_CURVE ( 'NONE', #29716, #36977, #41022, .T. ) ;
#15585 = ADVANCED_FACE ( 'NONE', ( #45333 ), #26744, .T. ) ;
#15586 = DIRECTION ( 'NONE',  ( 0.000000000000000000, 0.000000000000000000, 1.000000000000000000 ) ) ;
#15587 = DIRECTION ( 'NONE',  ( 0.000000000000000000, -0.9510565162951500895, -0.3090169943749583314 ) ) ;
#15588 = EDGE_CURVE ( 'NONE', #44874, #40000, #787, .T. ) ;
#15589 = VERTEX_POINT ( 'NONE', #34311 ) ;
#15590 = DIRECTION ( 'NONE',  ( 0.000000000000000000, 0.000000000000000000, 1.000000000000000000 ) ) ;
#15591 = ADVANCED_FACE ( 'NONE', ( #304 ), #45111, .T. ) ;
#15592 = CARTESIAN_POINT ( 'NONE',  ( 10.00000000000000000, -3.925862922255855647, -41.81611651403866858 ) ) ;
#15593 = EDGE_CURVE ( 'NONE', #21273, #13040, #32347, .T. ) ;
#15594 = CARTESIAN_POINT ( 'NONE',  ( 10.00000000000000000, 30.41916302227216562, -71.27951684757994144 ) ) ;
#15595 = ORIENTED_EDGE ( 'NONE', *, *, #16223, .T. ) ;
#15596 = AXIS2_PLACEMENT_3D ( 'NONE', #14011, #6676, #21603 ) ;
#15597 = VERTEX_POINT ( 'NONE', #7891 ) ;
#15598 = VECTOR ( 'NONE', #17276, 1000.000000000000000 ) ;
#15599 = EDGE_CURVE ( 'NONE', #10420, #29421, #22830, .T. ) ;
#15600 = VERTEX_POINT ( 'NONE', #45576 ) ;
#15601 = VERTEX_POINT ( 'NONE', #23309 ) ;
#15602 = CARTESIAN_POINT ( 'NONE',  ( 10.00000000000000000, -6.736453364083817341, 36.88895765772630142 ) ) ;
#15603 = CARTESIAN_POINT ( 'NONE',  ( 12.49999999999999645, 1.530808498934191127E-15, -125.0000000000000000 ) ) ;
#15604 = EDGE_LOOP ( 'NONE', ( #5227, #14839, #30598, #969 ) ) ;
#15605 = EDGE_CURVE ( 'NONE', #19547, #48421, #5677, .T. ) ;
#15606 = CARTESIAN_POINT ( 'NONE',  ( 10.00000000000000000, 0.000000000000000000, 0.000000000000000000 ) ) ;
#15607 = ORIENTED_EDGE ( 'NONE', *, *, #34839, .F. ) ;
#15608 = ORIENTED_EDGE ( 'NONE', *, *, #3924, .F. ) ;
#15609 = CARTESIAN_POINT ( 'NONE',  ( 0.000000000000000000, 0.000000000000000000, 0.000000000000000000 ) ) ;
#15611 = ORIENTED_EDGE ( 'NONE', *, *, #44008, .T. ) ;
#15610 = DIRECTION ( 'NONE',  ( -1.000000000000000000, 0.000000000000000000, 0.000000000000000000 ) ) ;
#15612 = EDGE_CURVE ( 'NONE', #11145, #690, #28188, .T. ) ;
#15613 = LINE ( 'NONE', #45237, #32139 ) ;
#15614 = EDGE_LOOP ( 'NONE', ( #16118, #9536, #8798, #48443 ) ) ;
#15615 = VERTEX_POINT ( 'NONE', #43372 ) ;
#15616 = LINE ( 'NONE', #30543, #41151 ) ;
#15617 = ORIENTED_EDGE ( 'NONE', *, *, #1187, .T. ) ;
#15618 = VERTEX_POINT ( 'NONE', #46311 ) ;
#15619 = DIRECTION ( 'NONE',  ( -1.000000000000000000, -0.000000000000000000, -0.000000000000000000 ) ) ;
#15620 = CARTESIAN_POINT ( 'NONE',  ( 10.00000000000000000, 17.67226234102826510, 33.17418723428314564 ) ) ;
#15621 = DIRECTION ( 'NONE',  ( -1.000000000000000000, -0.000000000000000000, -0.000000000000000000 ) ) ;
#15622 = ORIENTED_EDGE ( 'NONE', *, *, #41506, .T. ) ;
#15623 = ORIENTED_EDGE ( 'NONE', *, *, #33977, .T. ) ;
#15625 = ADVANCED_FACE ( 'NONE', ( #12784 ), #1763, .F. ) ;
#15624 = DIRECTION ( 'NONE',  ( -1.000000000000000000, 0.000000000000000000, -0.000000000000000000 ) ) ;
#15626 = CIRCLE ( 'NONE', #3106, 31.99999999999999289 ) ;
#15627 = DIRECTION ( 'NONE',  ( 0.000000000000000000, 0.000000000000000000, 1.000000000000000000 ) ) ;
#15628 = ORIENTED_EDGE ( 'NONE', *, *, #32656, .F. ) ;
#15629 = VECTOR ( 'NONE', #22592, 1000.000000000000000 ) ;
#15630 = EDGE_CURVE ( 'NONE', #25422, #36021, #23734, .T. ) ;
#15631 = DIRECTION ( 'NONE',  ( -0.000000000000000000, 0.2079116908177663092, 0.9781476007338041345 ) ) ;
#15632 = ORIENTED_EDGE ( 'NONE', *, *, #10103, .F. ) ;
#15633 = DIRECTION ( 'NONE',  ( -1.000000000000000000, -0.000000000000000000, 0.000000000000000000 ) ) ;
#15634 = AXIS2_PLACEMENT_3D ( 'NONE', #13972, #28896, #43832 ) ;
#15635 = CARTESIAN_POINT ( 'NONE',  ( -23.54415474984308787, -120.4156646670583086, 2.500000000000000000 ) ) ;
#15636 = DIRECTION ( 'NONE',  ( 1.000000000000000000, -0.000000000000000000, -0.000000000000000000 ) ) ;
#15637 = LINE ( 'NONE', #42312, #42557 ) ;
#15638 = EDGE_CURVE ( 'NONE', #31411, #17439, #47191, .T. ) ;
#15639 = LINE ( 'NONE', #4867, #47148 ) ;
#15640 = CARTESIAN_POINT ( 'NONE',  ( 11.99999999999999822, -20.41045688087772092, -72.35160999960838524 ) ) ;
#15641 = ADVANCED_FACE ( 'NONE', ( #2236 ), #43601, .T. ) ;
#15642 = CIRCLE ( 'NONE', #14945, 37.49900000000000233 ) ;
#15643 = DIRECTION ( 'NONE',  ( 1.000000000000000000, 0.000000000000000000, -0.000000000000000000 ) ) ;
#15644 = LINE ( 'NONE', #41360, #9100 ) ;
#15645 = AXIS2_PLACEMENT_3D ( 'NONE', #1543, #24064, #6180 ) ;
#15646 = CARTESIAN_POINT ( 'NONE',  ( 10.00000000000000000, -30.84782396557201878, -21.32104025579148399 ) ) ;
#15647 = EDGE_CURVE ( 'NONE', #43176, #38863, #43287, .T. ) ;
#15648 = ORIENTED_EDGE ( 'NONE', *, *, #33535, .T. ) ;
#15649 = CARTESIAN_POINT ( 'NONE',  ( 10.00000000000000000, 0.000000000000000000, 0.000000000000000000 ) ) ;
#15650 = FACE_OUTER_BOUND ( 'NONE', #14527, .T. ) ;
#15651 = DIRECTION ( 'NONE',  ( 0.000000000000000000, -0.8090169943749531134, 0.5877852522924654766 ) ) ;
#15652 = ORIENTED_EDGE ( 'NONE', *, *, #7890, .T. ) ;
#15653 = DIRECTION ( 'NONE',  ( 1.000000000000000000, 0.000000000000000000, 0.000000000000000000 ) ) ;
#15654 = CARTESIAN_POINT ( 'NONE',  ( 0.000000000000000000, 0.000000000000000000, 0.000000000000000000 ) ) ;
#15655 = LINE ( 'NONE', #41141, #45649 ) ;
#15656 = ORIENTED_EDGE ( 'NONE', *, *, #39007, .T. ) ;
#15657 = VERTEX_POINT ( 'NONE', #17394 ) ;
#15658 = CIRCLE ( 'NONE', #19548, 13.71399988598171049 ) ;
#15659 = VECTOR ( 'NONE', #47284, 1000.000000000000114 ) ;
#15660 = DIRECTION ( 'NONE',  ( -1.000000000000000000, 0.000000000000000000, -0.000000000000000000 ) ) ;
#15661 = AXIS2_PLACEMENT_3D ( 'NONE', #32196, #47112, #28523 ) ;
#15662 = CIRCLE ( 'NONE', #43036, 32.00000000000000000 ) ;
#15663 = VERTEX_POINT ( 'NONE', #38978 ) ;
#15664 = ORIENTED_EDGE ( 'NONE', *, *, #46717, .F. ) ;
#15665 = ORIENTED_EDGE ( 'NONE', *, *, #42046, .F. ) ;
#15666 = VECTOR ( 'NONE', #17491, 1000.000000000000000 ) ;
#15667 = AXIS2_PLACEMENT_3D ( 'NONE', #35073, #46827, #20147 ) ;
#15668 = PLANE ( 'NONE',  #41459 ) ;
#15669 = ORIENTED_EDGE ( 'NONE', *, *, #46940, .T. ) ;
#15670 = AXIS2_PLACEMENT_3D ( 'NONE', #28148, #43083, #47235 ) ;
#15671 = VERTEX_POINT ( 'NONE', #17159 ) ;
#15672 = DIRECTION ( 'NONE',  ( 0.000000000000000000, 0.000000000000000000, 1.000000000000000000 ) ) ;
#15673 = VERTEX_POINT ( 'NONE', #35046 ) ;
#15674 = DIRECTION ( 'NONE',  ( -1.000000000000000000, 0.000000000000000000, 0.000000000000000000 ) ) ;
#15675 = ORIENTED_EDGE ( 'NONE', *, *, #47127, .F. ) ;
#15676 = CARTESIAN_POINT ( 'NONE',  ( 11.99999999999999822, 63.18004540533030422, 44.88180994100399346 ) ) ;
#15677 = DIRECTION ( 'NONE',  ( 0.000000000000000000, 0.000000000000000000, 1.000000000000000000 ) ) ;
#15678 = ORIENTED_EDGE ( 'NONE', *, *, #11015, .T. ) ;
#15679 = CARTESIAN_POINT ( 'NONE',  ( 2.117611129180199558, -93.54218975225703048, 5.500000000000000000 ) ) ;
#15680 = VERTEX_POINT ( 'NONE', #32353 ) ;
#15681 = CARTESIAN_POINT ( 'NONE',  ( 10.00000000000000000, 51.03279382321166224, -55.19960302592011914 ) ) ;
#15682 = EDGE_CURVE ( 'NONE', #22252, #270, #8081, .T. ) ;
#15683 = DIRECTION ( 'NONE',  ( 0.000000000000000000, 0.000000000000000000, -1.000000000000000000 ) ) ;
#15684 = ORIENTED_EDGE ( 'NONE', *, *, #12788, .T. ) ;
#15685 = CARTESIAN_POINT ( 'NONE',  ( 10.00000000000000000, 3.894527615419054456, -81.90746397400386059 ) ) ;
#15686 = VERTEX_POINT ( 'NONE', #47278 ) ;
#15687 = VERTEX_POINT ( 'NONE', #46801 ) ;
#15688 = EDGE_CURVE ( 'NONE', #39357, #42999, #22163, .T. ) ;
#15689 = DIRECTION ( 'NONE',  ( -1.000000000000000000, -0.000000000000000000, -0.000000000000000000 ) ) ;
#15690 = DIRECTION ( 'NONE',  ( 0.7273375899149802093, -0.6862798483830544471, 0.000000000000000000 ) ) ;
#15691 = ORIENTED_EDGE ( 'NONE', *, *, #44235, .F. ) ;
#15692 = CARTESIAN_POINT ( 'NONE',  ( -30.50000000000000000, -120.0000000000000000, 2.500000000000000000 ) ) ;
#15693 = CARTESIAN_POINT ( 'NONE',  ( -10.00000000000000000, 0.000000000000000000, 0.000000000000000000 ) ) ;
#15694 = DIRECTION ( 'NONE',  ( -0.7071067811865474617, 8.659560562354932858E-17, -0.7071067811865474617 ) ) ;
#15695 = EDGE_CURVE ( 'NONE', #47223, #5925, #27660, .T. ) ;
#15696 = DIRECTION ( 'NONE',  ( 0.000000000000000000, 0.000000000000000000, 1.000000000000000000 ) ) ;
#15697 = CARTESIAN_POINT ( 'NONE',  ( 11.99999999999999822, 2.946379043147425492, -75.11764819372145041 ) ) ;
#15698 = ADVANCED_FACE ( 'NONE', ( #5436 ), #28677, .T. ) ;
#15699 = FACE_OUTER_BOUND ( 'NONE', #29139, .T. ) ;
#15700 = ORIENTED_EDGE ( 'NONE', *, *, #27223, .F. ) ;
#15701 = DIRECTION ( 'NONE',  ( -1.000000000000000000, 0.000000000000000000, 0.000000000000000000 ) ) ;
#15702 = DIRECTION ( 'NONE',  ( 1.000000000000000000, -0.000000000000000000, 0.000000000000000000 ) ) ;
#15703 = DIRECTION ( 'NONE',  ( 0.000000000000000000, 0.000000000000000000, 1.000000000000000000 ) ) ;
#15704 = ADVANCED_FACE ( 'NONE', ( #43124 ), #20851, .F. ) ;
#15705 = EDGE_LOOP ( 'NONE', ( #25401, #47493, #14474, #36014 ) ) ;
#15706 = AXIS2_PLACEMENT_3D ( 'NONE', #17909, #10326, #47760 ) ;
#15707 = AXIS2_PLACEMENT_3D ( 'NONE', #11223, #34209, #22241 ) ;
#15708 = EDGE_CURVE ( 'NONE', #41148, #26085, #9571, .T. ) ;
#15709 = DIRECTION ( 'NONE',  ( -1.000000000000000000, -0.000000000000000000, 0.000000000000000000 ) ) ;
#15710 = DIRECTION ( 'NONE',  ( 1.000000000000000000, 0.000000000000000000, -0.000000000000000000 ) ) ;
#15711 = CARTESIAN_POINT ( 'NONE',  ( 0.000000000000000000, 65.58780272294076497, 36.73666225445916211 ) ) ;
#15712 = CARTESIAN_POINT ( 'NONE',  ( 10.00000000000000000, -72.35432306680498016, 20.40083707022857951 ) ) ;
#15713 = EDGE_LOOP ( 'NONE', ( #47476, #41385, #26259, #45866 ) ) ;
#15714 = VECTOR ( 'NONE', #42621, 1000.000000000000000 ) ;
#15715 = ORIENTED_EDGE ( 'NONE', *, *, #17340, .T. ) ;
#15716 = DIRECTION ( 'NONE',  ( -1.000000000000000000, 0.000000000000000000, -0.000000000000000000 ) ) ;
#15717 = VECTOR ( 'NONE', #38391, 1000.000000000000000 ) ;
#15718 = ORIENTED_EDGE ( 'NONE', *, *, #41867, .F. ) ;
#15719 =( REPRESENTATION_RELATIONSHIP ('NONE','NONE', #5957, #40966 ) REPRESENTATION_RELATIONSHIP_WITH_TRANSFORMATION ( #16443 )SHAPE_REPRESENTATION_RELATIONSHIP( ) );
#15720 = DIRECTION ( 'NONE',  ( 1.000000000000000000, -0.000000000000000000, 0.000000000000000000 ) ) ;
#15721 = ITEM_DEFINED_TRANSFORMATION ( 'NONE', 'NONE', #28027,  #11636 ) ;
#15722 = LINE ( 'NONE', #41431, #28392 ) ;
#15723 = VERTEX_POINT ( 'NONE', #20121 ) ;
#15724 = EDGE_CURVE ( 'NONE', #29983, #17937, #38607, .T. ) ;
#15725 = CARTESIAN_POINT ( 'NONE',  ( 10.00000000000000000, -39.47590169984793818, -71.87247863392455827 ) ) ;
#15726 = ORIENTED_EDGE ( 'NONE', *, *, #2477, .F. ) ;
#15727 = CIRCLE ( 'NONE', #14964, 12.49999999999999822 ) ;
#15728 = ADVANCED_FACE ( 'NONE', ( #16935 ), #24518, .T. ) ;
#15729 = CARTESIAN_POINT ( 'NONE',  ( -9.937067298023318784, 7.583184918921300088, 125.0000000000000000 ) ) ;
#15730 = VECTOR ( 'NONE', #34380, 1000.000000000000227 ) ;
#15731 = DIRECTION ( 'NONE',  ( -0.000000000000000000, -0.000000000000000000, -1.000000000000000000 ) ) ;
#15732 = DIRECTION ( 'NONE',  ( -1.000000000000000000, -0.000000000000000000, -0.000000000000000000 ) ) ;
#15733 = AXIS2_PLACEMENT_3D ( 'NONE', #16649, #1244, #31600 ) ;
#15734 = CIRCLE ( 'NONE', #44668, 42.00000000000000000 ) ;
#15735 = EDGE_CURVE ( 'NONE', #22256, #24326, #17476, .T. ) ;
#15736 = ORIENTED_EDGE ( 'NONE', *, *, #45775, .T. ) ;
#15737 = EDGE_CURVE ( 'NONE', #30648, #47828, #21793, .T. ) ;
#15738 = CIRCLE ( 'NONE', #34487, 12.49999999999999645 ) ;
#15739 = LINE ( 'NONE', #39223, #7391 ) ;
#15740 = DIRECTION ( 'NONE',  ( -1.000000000000000000, 0.000000000000000000, -0.000000000000000000 ) ) ;
#15741 = AXIS2_PLACEMENT_3D ( 'NONE', #45257, #10765, #3657 ) ;
#15742 = DIRECTION ( 'NONE',  ( -1.000000000000000000, 0.000000000000000000, 0.000000000000000000 ) ) ;
#15743 = DIRECTION ( 'NONE',  ( 0.000000000000000000, 0.000000000000000000, -1.000000000000000000 ) ) ;
#15744 = ORIENTED_EDGE ( 'NONE', *, *, #13798, .F. ) ;
#15745 = DIRECTION ( 'NONE',  ( -1.000000000000000000, 0.000000000000000000, 0.000000000000000000 ) ) ;
#15746 = ORIENTED_EDGE ( 'NONE', *, *, #2875, .F. ) ;
#15747 = ORIENTED_EDGE ( 'NONE', *, *, #2808, .F. ) ;
#15748 = DIRECTION ( 'NONE',  ( -1.000000000000000000, -0.000000000000000000, -0.000000000000000000 ) ) ;
#15749 = ORIENTED_EDGE ( 'NONE', *, *, #46757, .F. ) ;
#15750 = AXIS2_PLACEMENT_3D ( 'NONE', #23497, #7845, #41388 ) ;
#15751 = LINE ( 'NONE', #4733, #7424 ) ;
#15752 = DIRECTION ( 'NONE',  ( 0.000000000000000000, 0.000000000000000000, -1.000000000000000000 ) ) ;
#15753 = FACE_OUTER_BOUND ( 'NONE', #5032, .T. ) ;
#15754 = ORIENTED_EDGE ( 'NONE', *, *, #768, .F. ) ;
#15755 = CARTESIAN_POINT ( 'NONE',  ( 25.81725066941077529, -113.8380548628854854, 5.500000000000000000 ) ) ;
#15756 = EDGE_CURVE ( 'NONE', #42173, #33476, #5756, .T. ) ;
#15757 = DIRECTION ( 'NONE',  ( -1.000000000000000000, -0.000000000000000000, 0.000000000000000000 ) ) ;
#15758 = EDGE_CURVE ( 'NONE', #5993, #34646, #43834, .T. ) ;
#15759 = EDGE_CURVE ( 'NONE', #9826, #5621, #36244, .T. ) ;
#15760 = CARTESIAN_POINT ( 'NONE',  ( 1.192633404626820770, -120.9097392825245407, 2.500000000000000000 ) ) ;
#15761 = DIRECTION ( 'NONE',  ( -1.000000000000000000, -0.000000000000000000, 0.000000000000000000 ) ) ;
#15762 = CIRCLE ( 'NONE', #26692, 42.00000000000000000 ) ;
#15763 = FACE_OUTER_BOUND ( 'NONE', #35101, .T. ) ;
#15764 = DIRECTION ( 'NONE',  ( -1.000000000000000000, 0.000000000000000000, -0.000000000000000000 ) ) ;
#15765 = DIRECTION ( 'NONE',  ( 0.000000000000000000, 0.8910065241883656784, 0.4539904997395510788 ) ) ;
#15766 = CARTESIAN_POINT ( 'NONE',  ( 10.00000000000000000, 0.000000000000000000, 0.000000000000000000 ) ) ;
#15767 = DIRECTION ( 'NONE',  ( 0.000000000000000000, -6.938893903907229955E-15, 1.000000000000000000 ) ) ;
#15768 = DIRECTION ( 'NONE',  ( -0.000000000000000000, 0.1045284632676569680, 0.9945218953682730678 ) ) ;
#15769 = EDGE_LOOP ( 'NONE', ( #16833, #40874, #41748, #38443 ) ) ;
#15770 = DIRECTION ( 'NONE',  ( -1.000000000000000000, 0.000000000000000000, 0.000000000000000000 ) ) ;
#15771 = PRODUCT_RELATED_PRODUCT_CATEGORY ( 'part', '', ( #2652 ) ) ;
#15772 = AXIS2_PLACEMENT_3D ( 'NONE', #14138, #21720, #36643 ) ;
#15773 = EDGE_LOOP ( 'NONE', ( #17259, #2831, #12833, #1584 ) ) ;
#15774 = CARTESIAN_POINT ( 'NONE',  ( 10.00000000000000000, 30.80686688397041451, -21.53537804866048688 ) ) ;
#15775 = CYLINDRICAL_SURFACE ( 'NONE', #5054, 77.49899999999999523 ) ;
#15776 = VECTOR ( 'NONE', #4009, 1000.000000000000000 ) ;
#15777 = VERTEX_POINT ( 'NONE', #18368 ) ;
#15778 = ORIENTED_EDGE ( 'NONE', *, *, #31232, .T. ) ;
#15779 = VECTOR ( 'NONE', #15336, 1000.000000000000114 ) ;
#15780 = VECTOR ( 'NONE', #38279, 1000.000000000000000 ) ;
#15781 = DIRECTION ( 'NONE',  ( -1.000000000000000000, -0.000000000000000000, 0.000000000000000000 ) ) ;
#15782 = AXIS2_PLACEMENT_3D ( 'NONE', #24671, #39617, #6078 ) ;
#15783 = VERTEX_POINT ( 'NONE', #33301 ) ;
#15784 = EDGE_LOOP ( 'NONE', ( #18567, #24826, #23410, #1679 ) ) ;
#15785 = ORIENTED_EDGE ( 'NONE', *, *, #17071, .T. ) ;
#15786 = ORIENTED_EDGE ( 'NONE', *, *, #5867, .T. ) ;
#15787 = CYLINDRICAL_SURFACE ( 'NONE', #40612, 37.49900000000000233 ) ;
#15788 = ORIENTED_EDGE ( 'NONE', *, *, #31749, .F. ) ;
#15789 = ORIENTED_EDGE ( 'NONE', *, *, #27886, .F. ) ;
#15790 = ADVANCED_FACE ( 'NONE', ( #44554, #21312 ), #47731, .T. ) ;
#15791 = CARTESIAN_POINT ( 'NONE',  ( 0.000000000000000000, -34.44570377933648331, 69.42325613327426481 ) ) ;
#15792 = CARTESIAN_POINT ( 'NONE',  ( 5.000000000000000000, -63.97538442413390669, -51.29473840253292849 ) ) ;
#15793 = CARTESIAN_POINT ( 'NONE',  ( 12.49999999999999645, 1.530808498934191127E-15, -56.19999999999998863 ) ) ;
#15794 = EDGE_CURVE ( 'NONE', #18404, #22636, #25699, .T. ) ;
#15795 = VERTEX_POINT ( 'NONE', #47983 ) ;
#15796 = DIRECTION ( 'NONE',  ( -1.000000000000000000, 0.000000000000000000, 0.000000000000000000 ) ) ;
#15797 = VERTEX_POINT ( 'NONE', #10295 ) ;
#15798 = EDGE_CURVE ( 'NONE', #12057, #3234, #14467, .T. ) ;
#15799 = VERTEX_POINT ( 'NONE', #11029 ) ;
#15800 = CARTESIAN_POINT ( 'NONE',  ( 0.000000000000000000, -10.45096189432314837, -21.10159698893440350 ) ) ;
#15801 = FACE_OUTER_BOUND ( 'NONE', #1108, .T. ) ;
#15802 = AXIS2_PLACEMENT_3D ( 'NONE', #3781, #18702, #33633 ) ;
#15803 = VERTEX_POINT ( 'NONE', #7357 ) ;
#15804 = VERTEX_POINT ( 'NONE', #25212 ) ;
#15805 = CARTESIAN_POINT ( 'NONE',  ( 0.000000000000000000, 37.58145647212453611, 0.6853352020791767529 ) ) ;
#15806 = ORIENTED_EDGE ( 'NONE', *, *, #35590, .F. ) ;
#15807 = CIRCLE ( 'NONE', #23623, 77.49900000000000944 ) ;
#15808 = CARTESIAN_POINT ( 'NONE',  ( 0.000000000000000000, 51.02545421589402252, -55.20638768913705263 ) ) ;
#15809 = DIRECTION ( 'NONE',  ( 0.000000000000000000, 0.000000000000000000, 1.000000000000000000 ) ) ;
#15810 = CARTESIAN_POINT ( 'NONE',  ( 10.00000000000000000, 0.000000000000000000, 0.000000000000000000 ) ) ;
#15811 = DIRECTION ( 'NONE',  ( 0.000000000000000000, -0.2334453638559126909, 0.9723699203976748917 ) ) ;
#15812 = DIRECTION ( 'NONE',  ( 0.000000000000000000, -0.7071067811865535679, 0.7071067811865413555 ) ) ;
#15813 = CARTESIAN_POINT ( 'NONE',  ( 0.7800914985199594032, -118.7188063167744900, 2.500000000000000000 ) ) ;
#15814 = CIRCLE ( 'NONE', #24396, 16.00000000000000000 ) ;
#15815 = LINE ( 'NONE', #30750, #4908 ) ;
#15816 = ADVANCED_FACE ( 'NONE', ( #47503 ), #22293, .T. ) ;
#15817 = EDGE_CURVE ( 'NONE', #21525, #14416, #13973, .T. ) ;
#15818 = CARTESIAN_POINT ( 'NONE',  ( -7.469491406282116053, 4.756046723998915482, -45.00000000000000000 ) ) ;
#15819 = DIRECTION ( 'NONE',  ( -1.000000000000000000, -0.000000000000000000, -0.000000000000000000 ) ) ;
#15820 = DIRECTION ( 'NONE',  ( 1.000000000000000000, 0.000000000000000000, 0.000000000000000000 ) ) ;
#15821 = LINE ( 'NONE', #12634, #412 ) ;
#15822 = ORIENTED_EDGE ( 'NONE', *, *, #34295, .F. ) ;
#15823 = ORIENTED_EDGE ( 'NONE', *, *, #18070, .F. ) ;
#15824 = CARTESIAN_POINT ( 'NONE',  ( 10.00000000000000000, 0.000000000000000000, 0.000000000000000000 ) ) ;
#15825 = VECTOR ( 'NONE', #46903, 1000.000000000000114 ) ;
#15826 = DIRECTION ( 'NONE',  ( -0.9227826878668540234, -0.3853207896976547642, 0.000000000000000000 ) ) ;
#15827 = DIRECTION ( 'NONE',  ( 0.000000000000000000, 0.000000000000000000, 1.000000000000000000 ) ) ;
#15828 = LINE ( 'NONE', #34402, #46379 ) ;
#15829 = VECTOR ( 'NONE', #20275, 1000.000000000000114 ) ;
#15830 = DIRECTION ( 'NONE',  ( 0.9827303690289279636, 0.1850432970638682395, 0.000000000000000000 ) ) ;
#15831 = DIRECTION ( 'NONE',  ( -1.000000000000000000, 0.000000000000000000, -0.000000000000000000 ) ) ;
#15832 = EDGE_CURVE ( 'NONE', #23222, #3743, #16733, .T. ) ;
#15833 = DIRECTION ( 'NONE',  ( 0.9038112904824842087, -0.4279312458753000703, 0.000000000000000000 ) ) ;
#15834 = CARTESIAN_POINT ( 'NONE',  ( 0.000000000000000000, 10.41901085202135491, -40.68715046381917944 ) ) ;
#15835 = ORIENTED_EDGE ( 'NONE', *, *, #10836, .T. ) ;
#15836 = LINE ( 'NONE', #4821, #8883 ) ;
#15837 = ORIENTED_EDGE ( 'NONE', *, *, #38501, .F. ) ;
#15838 = ORIENTED_EDGE ( 'NONE', *, *, #11516, .T. ) ;
#15839 = VECTOR ( 'NONE', #10837, 1000.000000000000000 ) ;
#15840 = ORIENTED_EDGE ( 'NONE', *, *, #36135, .F. ) ;
#15841 = ORIENTED_EDGE ( 'NONE', *, *, #10693, .T. ) ;
#15842 = AXIS2_PLACEMENT_3D ( 'NONE', #7790, #8284, #18797 ) ;
#15843 = ORIENTED_EDGE ( 'NONE', *, *, #27938, .T. ) ;
#15844 = DIRECTION ( 'NONE',  ( -0.3853207896976547642, 0.9227826878668540234, 0.000000000000000000 ) ) ;
#15845 = ORIENTED_EDGE ( 'NONE', *, *, #16114, .T. ) ;
#15846 = VECTOR ( 'NONE', #46600, 1000.000000000000000 ) ;
#15847 = ORIENTED_EDGE ( 'NONE', *, *, #2059, .F. ) ;
#15848 = CIRCLE ( 'NONE', #22869, 37.49900000000000233 ) ;
#15849 = CARTESIAN_POINT ( 'NONE',  ( 10.00000000000000000, 8.966570791700695153, 81.50828551894228724 ) ) ;
#15850 = VECTOR ( 'NONE', #10356, 1000.000000000000000 ) ;
#15851 = VERTEX_POINT ( 'NONE', #2949 ) ;
#15852 = ADVANCED_FACE ( 'NONE', ( #17876 ), #14219, .T. ) ;
#15853 = ORIENTED_EDGE ( 'NONE', *, *, #44791, .T. ) ;
#15854 = VERTEX_POINT ( 'NONE', #40420 ) ;
#15855 = ADVANCED_FACE ( 'NONE', ( #6879 ), #42816, .F. ) ;
#15856 = CARTESIAN_POINT ( 'NONE',  ( 0.000000000000000000, -75.11764819372145041, 29.05362095685286761 ) ) ;
#15857 = DIRECTION ( 'NONE',  ( 0.000000000000000000, 0.5224985647159441360, 0.8526401643540952868 ) ) ;
#15858 = DIRECTION ( 'NONE',  ( 0.4796670183876304283, -0.8774505977381978905, 0.000000000000000000 ) ) ;
#15859 = ORIENTED_EDGE ( 'NONE', *, *, #6841, .T. ) ;
#15860 = EDGE_LOOP ( 'NONE', ( #3460, #42962, #30005, #35316 ) ) ;
#15861 = DIRECTION ( 'NONE',  ( -1.000000000000000000, 0.000000000000000000, 0.000000000000000000 ) ) ;
#15862 = EDGE_CURVE ( 'NONE', #1537, #13208, #35928, .T. ) ;
#15863 = VERTEX_POINT ( 'NONE', #28828 ) ;
#15864 = VERTEX_POINT ( 'NONE', #39630 ) ;
#15865 = CYLINDRICAL_SURFACE ( 'NONE', #35341, 35.50000000000000711 ) ;
#15866 = CARTESIAN_POINT ( 'NONE',  ( 0.000000000000000000, 21.40280677340371795, 36.13751322684426270 ) ) ;
#15867 = ORIENTED_EDGE ( 'NONE', *, *, #48449, .T. ) ;
#15868 = DIRECTION ( 'NONE',  ( 0.000000000000000000, 0.000000000000000000, 1.000000000000000000 ) ) ;
#15869 = AXIS2_PLACEMENT_3D ( 'NONE', #28485, #25040, #47786 ) ;
#15870 = FACE_OUTER_BOUND ( 'NONE', #13821, .T. ) ;
#15871 = ORIENTED_EDGE ( 'NONE', *, *, #17977, .F. ) ;
#15872 = ORIENTED_EDGE ( 'NONE', *, *, #33803, .T. ) ;
#15873 = EDGE_CURVE ( 'NONE', #41996, #35358, #13423, .T. ) ;
#15874 = DIRECTION ( 'NONE',  ( 0.000000000000000000, 0.000000000000000000, 1.000000000000000000 ) ) ;
#15875 = DIRECTION ( 'NONE',  ( 0.000000000000000000, 0.000000000000000000, 1.000000000000000000 ) ) ;
#15876 = CIRCLE ( 'NONE', #14295, 31.99999999999998224 ) ;
#15877 = ORIENTED_EDGE ( 'NONE', *, *, #45997, .F. ) ;
#15878 = EDGE_CURVE ( 'NONE', #35390, #33288, #44071, .T. ) ;
#15879 = CARTESIAN_POINT ( 'NONE',  ( 10.00000000000000000, -37.58145647212453611, -0.6853352020794456489 ) ) ;
#15880 = ORIENTED_EDGE ( 'NONE', *, *, #12124, .T. ) ;
#15881 = DIRECTION ( 'NONE',  ( 0.000000000000000000, 0.000000000000000000, 1.000000000000000000 ) ) ;
#15882 = VECTOR ( 'NONE', #14123, 1000.000000000000000 ) ;
#15883 = FACE_OUTER_BOUND ( 'NONE', #38032, .T. ) ;
#15884 = DIRECTION ( 'NONE',  ( 0.000000000000000000, 0.000000000000000000, 1.000000000000000000 ) ) ;
#15885 = ORIENTED_EDGE ( 'NONE', *, *, #44973, .T. ) ;
#15886 = LINE ( 'NONE', #11976, #36965 ) ;
#15887 = AXIS2_PLACEMENT_3D ( 'NONE', #21721, #28338, #29062 ) ;
#15888 = LINE ( 'NONE', #12463, #26335 ) ;
#15889 = EDGE_CURVE ( 'NONE', #17705, #7024, #16692, .T. ) ;
#15890 = CIRCLE ( 'NONE', #22134, 31.99999999999998934 ) ;
#15891 = CARTESIAN_POINT ( 'NONE',  ( 10.00000000000000000, 49.70050353004889132, 59.46389618801982380 ) ) ;
#15892 = DIRECTION ( 'NONE',  ( 0.000000000000000000, 0.000000000000000000, 1.000000000000000000 ) ) ;
#15893 = CARTESIAN_POINT ( 'NONE',  ( 0.000000000000000000, 0.000000000000000000, 0.000000000000000000 ) ) ;
#15894 = SHAPE_REPRESENTATION_RELATIONSHIP ( 'NONE' , 'NONE' ,  #1226, #38066 ) ;
#15895 = CARTESIAN_POINT ( 'NONE',  ( 0.000000000000000000, 0.000000000000000000, 0.000000000000000000 ) ) ;
#15896 = VERTEX_POINT ( 'NONE', #9748 ) ;
#15897 = EDGE_CURVE ( 'NONE', #15224, #19441, #21234, .T. ) ;
#15898 = UNCERTAINTY_MEASURE_WITH_UNIT (LENGTH_MEASURE( 1.000000000000000082E-05 ), #23466, 'distance_accuracy_value', 'NONE');
#15899 = DIRECTION ( 'NONE',  ( 0.000000000000000000, 0.000000000000000000, 1.000000000000000000 ) ) ;
#15900 = DIRECTION ( 'NONE',  ( -1.000000000000000000, 0.000000000000000000, 0.000000000000000000 ) ) ;
#15901 = AXIS2_PLACEMENT_3D ( 'NONE', #21559, #6389, #2460 ) ;
#15902 = DIRECTION ( 'NONE',  ( 0.000000000000000000, 0.000000000000000000, 1.000000000000000000 ) ) ;
#15903 = EDGE_LOOP ( 'NONE', ( #172, #45559, #27855, #32802 ) ) ;
#15904 = AXIS2_PLACEMENT_3D ( 'NONE', #9751, #35457, #17093 ) ;
#15905 = EDGE_CURVE ( 'NONE', #15601, #13149, #36167, .T. ) ;
#15906 = DIRECTION ( 'NONE',  ( -1.000000000000000000, 0.000000000000000000, -0.000000000000000000 ) ) ;
#15907 = AXIS2_PLACEMENT_3D ( 'NONE', #24353, #32662, #39553 ) ;
#15908 = VECTOR ( 'NONE', #35907, 1000.000000000000000 ) ;
#15910 = ORIENTED_EDGE ( 'NONE', *, *, #22674, .F. ) ;
#15909 = CIRCLE ( 'NONE', #47930, 77.49899999999999523 ) ;
#15911 = ORIENTED_EDGE ( 'NONE', *, *, #6427, .F. ) ;
#15912 = ADVANCED_FACE ( 'NONE', ( #39377 ), #28425, .T. ) ;
#15913 = ORIENTED_EDGE ( 'NONE', *, *, #34315, .F. ) ;
#15914 = ORIENTED_EDGE ( 'NONE', *, *, #27750, .F. ) ;
#15915 = ORIENTED_EDGE ( 'NONE', *, *, #27879, .F. ) ;
#15916 = VECTOR ( 'NONE', #16550, 1000.000000000000000 ) ;
#15917 = EDGE_CURVE ( 'NONE', #6864, #10410, #28605, .T. ) ;
#15918 = CARTESIAN_POINT ( 'NONE',  ( 23.49916127795269460, -121.5130826919798039, 2.500000000000000000 ) ) ;
#15919 = VERTEX_POINT ( 'NONE', #24917 ) ;
#15920 = AXIS2_PLACEMENT_3D ( 'NONE', #23842, #34350, #11619 ) ;
#15921 = ORIENTED_EDGE ( 'NONE', *, *, #28185, .F. ) ;
#15922 = DIRECTION ( 'NONE',  ( -1.000000000000000000, 0.000000000000000000, -0.000000000000000000 ) ) ;
#15923 = EDGE_CURVE ( 'NONE', #30240, #37452, #6326, .T. ) ;
#15924 = ORIENTED_EDGE ( 'NONE', *, *, #42934, .T. ) ;
#15925 = LINE ( 'NONE', #4434, #10290 ) ;
#15926 = VECTOR ( 'NONE', #2707, 1000.000000000000000 ) ;
#15927 = EDGE_LOOP ( 'NONE', ( #5098, #16337, #25878, #1646 ) ) ;
#15928 = CARTESIAN_POINT ( 'NONE',  ( 10.00000000000000000, 0.000000000000000000, 0.000000000000000000 ) ) ;
#15929 = DIRECTION ( 'NONE',  ( 0.000000000000000000, 0.000000000000000000, 1.000000000000000000 ) ) ;
#15931 = VERTEX_POINT ( 'NONE', #32515 ) ;
#15930 = CIRCLE ( 'NONE', #34637, 77.49899999999998101 ) ;
#15932 = LINE ( 'NONE', #42115, #30584 ) ;
#15933 = ORIENTED_EDGE ( 'NONE', *, *, #37252, .T. ) ;
#15934 = LINE ( 'NONE', #37715, #23461 ) ;
#15935 = FACE_OUTER_BOUND ( 'NONE', #48315, .T. ) ;
#15936 = VERTEX_POINT ( 'NONE', #47437 ) ;
#15937 = CARTESIAN_POINT ( 'NONE',  ( 0.000000000000000000, -30.00120703465222149, 22.64427369931158296 ) ) ;
#15938 = VERTEX_POINT ( 'NONE', #40096 ) ;
#15939 = ORIENTED_EDGE ( 'NONE', *, *, #32982, .F. ) ;
#15940 = CARTESIAN_POINT ( 'NONE',  ( 0.000000000000000000, 16.00000000000000000, -2.500000000000000000 ) ) ;
#15941 = CARTESIAN_POINT ( 'NONE',  ( -7.469491406282094736, 4.756046723998911929, 32.98187577049606745 ) ) ;
#15942 = CARTESIAN_POINT ( 'NONE',  ( 10.00000000000000000, -62.20884554314051940, 46.21855187248608132 ) ) ;
#15943 = DIRECTION ( 'NONE',  ( 0.000000000000000000, 0.9238795325112851842, 0.3826834323650937786 ) ) ;
#15944 = CYLINDRICAL_SURFACE ( 'NONE', #44042, 31.99999999999998579 ) ;
#15945 = CARTESIAN_POINT ( 'NONE',  ( -1.459549131277904976, -119.6539995182286304, -2.500000000000000000 ) ) ;
#15946 = CARTESIAN_POINT ( 'NONE',  ( 0.000000000000000000, 0.000000000000000000, 0.000000000000000000 ) ) ;
#15947 = CARTESIAN_POINT ( 'NONE',  ( 0.000000000000000000, -58.39081064771713869, -50.95692526931392052 ) ) ;
#15948 = EDGE_CURVE ( 'NONE', #29613, #43524, #16865, .T. ) ;
#15949 = ORIENTED_EDGE ( 'NONE', *, *, #46189, .F. ) ;
#15950 = VECTOR ( 'NONE', #26967, 1000.000000000000000 ) ;
#15951 = CARTESIAN_POINT ( 'NONE',  ( -21.67772167707813935, -110.8034581014852762, -5.500000000000000000 ) ) ;
#15952 = DIRECTION ( 'NONE',  ( -1.000000000000000000, 0.000000000000000000, 0.000000000000000000 ) ) ;
#15953 = DIRECTION ( 'NONE',  ( -0.000000000000000000, -0.000000000000000000, -1.000000000000000000 ) ) ;
#15954 = ORIENTED_EDGE ( 'NONE', *, *, #12412, .T. ) ;
#15955 = AXIS2_PLACEMENT_3D ( 'NONE', #9601, #47310, #17425 ) ;
#15956 = CIRCLE ( 'NONE', #29215, 37.49900000000000233 ) ;
#15957 = CIRCLE ( 'NONE', #43309, 16.00000000000000000 ) ;
#15958 = DIRECTION ( 'NONE',  ( -1.000000000000000000, -0.000000000000000000, 0.000000000000000000 ) ) ;
#15959 = CARTESIAN_POINT ( 'NONE',  ( 11.99999999999999822, 11.30684508768339569, 76.66974797899841576 ) ) ;
#15960 = DIRECTION ( 'NONE',  ( 0.000000000000000000, -0.9876883405951359940, -0.1564344650402420545 ) ) ;
#15961 = DIRECTION ( 'NONE',  ( 0.000000000000000000, 0.4067366430757887730, 0.9135454576426059736 ) ) ;
#15962 = ORIENTED_EDGE ( 'NONE', *, *, #22166, .T. ) ;
#15963 = EDGE_CURVE ( 'NONE', #3496, #20812, #38649, .T. ) ;
#15964 = FACE_BOUND ( 'NONE', #4667, .T. ) ;
#15965 = AXIS2_PLACEMENT_3D ( 'NONE', #42928, #43644, #10110 ) ;
#15966 = VERTEX_POINT ( 'NONE', #21490 ) ;
#15967 = VECTOR ( 'NONE', #46228, 1000.000000000000000 ) ;
#15968 = DIRECTION ( 'NONE',  ( 1.000000000000000000, -0.000000000000000000, 0.000000000000000000 ) ) ;
#15969 = VECTOR ( 'NONE', #29079, 1000.000000000000114 ) ;
#15970 = ITEM_DEFINED_TRANSFORMATION ( 'NONE', 'NONE', #45994,  #11636 ) ;
#15971 = CARTESIAN_POINT ( 'NONE',  ( 11.99999999999999822, 55.19960302592066625, 51.03279382321107249 ) ) ;
#15972 = VERTEX_POINT ( 'NONE', #13188 ) ;
#15973 = EDGE_CURVE ( 'NONE', #24326, #22256, #31632, .T. ) ;
#15974 = DIRECTION ( 'NONE',  ( 0.3311129884571281101, 0.9435911131814402886, 0.000000000000000000 ) ) ;
#15975 = ORIENTED_EDGE ( 'NONE', *, *, #30357, .F. ) ;
#15976 = ADVANCED_FACE ( 'NONE', ( #1690 ), #32041, .T. ) ;
#15977 = AXIS2_PLACEMENT_3D ( 'NONE', #13003, #9310, #22000 ) ;
#15978 = LINE ( 'NONE', #30922, #4238 ) ;
#15979 = EDGE_CURVE ( 'NONE', #26518, #34988, #46484, .T. ) ;
#15980 = DIRECTION ( 'NONE',  ( -1.000000000000000000, 0.000000000000000000, -0.000000000000000000 ) ) ;
#15981 = AXIS2_PLACEMENT_3D ( 'NONE', #13582, #46645, #9914 ) ;
#15982 = CARTESIAN_POINT ( 'NONE',  ( 0.000000000000000000, 0.000000000000000000, 0.000000000000000000 ) ) ;
#15983 = AXIS2_PLACEMENT_3D ( 'NONE', #44610, #44131, #14760 ) ;
#15984 = ORIENTED_EDGE ( 'NONE', *, *, #8499, .T. ) ;
#15985 = EDGE_CURVE ( 'NONE', #44254, #28319, #24197, .T. ) ;
#15986 = VERTEX_POINT ( 'NONE', #9501 ) ;
#15987 = LINE ( 'NONE', #35061, #1132 ) ;
#15988 = DIRECTION ( 'NONE',  ( -1.000000000000000000, 0.000000000000000000, -0.000000000000000000 ) ) ;
#15989 = DIRECTION ( 'NONE',  ( -1.000000000000000000, 0.000000000000000000, -0.000000000000000000 ) ) ;
#15991 = ORIENTED_EDGE ( 'NONE', *, *, #13064, .F. ) ;
#15990 = DIRECTION ( 'NONE',  ( 0.000000000000000000, 0.000000000000000000, -1.000000000000000000 ) ) ;
#15992 = AXIS2_PLACEMENT_3D ( 'NONE', #4779, #30727, #7952 ) ;
#15993 = VECTOR ( 'NONE', #2452, 1000.000000000000000 ) ;
#15994 = VERTEX_POINT ( 'NONE', #24436 ) ;
#15995 = DIRECTION ( 'NONE',  ( -1.000000000000000000, -0.000000000000000000, 0.000000000000000000 ) ) ;
#15996 = ORIENTED_EDGE ( 'NONE', *, *, #16680, .T. ) ;
#15997 = ORIENTED_EDGE ( 'NONE', *, *, #22637, .F. ) ;
#15998 = CIRCLE ( 'NONE', #7404, 42.00000000000000000 ) ;
#15999 = DIRECTION ( 'NONE',  ( -0.000000000000000000, -0.000000000000000000, -1.000000000000000000 ) ) ;
#16000 = AXIS2_PLACEMENT_3D ( 'NONE', #558, #8608, #19617 ) ;
#16001 = DIRECTION ( 'NONE',  ( -1.000000000000000000, 0.000000000000000000, 0.000000000000000000 ) ) ;
#16002 = DIRECTION ( 'NONE',  ( -1.000000000000000000, -0.000000000000000000, -0.000000000000000000 ) ) ;
#16003 = LINE ( 'NONE', #42915, #11020 ) ;
#16004 = ORIENTED_EDGE ( 'NONE', *, *, #27039, .T. ) ;
#16005 = CARTESIAN_POINT ( 'NONE',  ( 0.000000000000000000, -68.67312586195022561, 35.91791733033451806 ) ) ;
#16006 = AXIS2_PLACEMENT_3D ( 'NONE', #37204, #3674, #18603 ) ;
#16007 = CARTESIAN_POINT ( 'NONE',  ( 11.99999999999999822, 0.000000000000000000, 0.000000000000000000 ) ) ;
#16008 = EDGE_CURVE ( 'NONE', #3237, #45718, #36418, .T. ) ;
#16009 = CARTESIAN_POINT ( 'NONE',  ( 10.00000000000000000, 0.000000000000000000, 0.000000000000000000 ) ) ;
#16010 = DIRECTION ( 'NONE',  ( -1.000000000000000000, 0.000000000000000000, 0.000000000000000000 ) ) ;
#16011 = CARTESIAN_POINT ( 'NONE',  ( 0.000000000000000000, 0.000000000000000000, 0.000000000000000000 ) ) ;
#16012 = DIRECTION ( 'NONE',  ( -1.000000000000000000, 0.000000000000000000, 0.000000000000000000 ) ) ;
#16013 = FACE_OUTER_BOUND ( 'NONE', #39038, .T. ) ;
#16014 = CARTESIAN_POINT ( 'NONE',  ( 4.999999999999999112, -36.13751322684434797, 21.40280677340357940 ) ) ;
#16015 = CARTESIAN_POINT ( 'NONE',  ( 10.00000000000000000, 6.736453364084091788, -36.88895765772625879 ) ) ;
#16016 = CYLINDRICAL_SURFACE ( 'NONE', #245, 16.00000000000000355 ) ;
#16017 = ORIENTED_EDGE ( 'NONE', *, *, #33044, .T. ) ;
#16018 = EDGE_LOOP ( 'NONE', ( #19478, #28689, #3991, #34497 ) ) ;
#16019 = AXIS2_PLACEMENT_3D ( 'NONE', #41116, #29835, #15168 ) ;
#16020 = EDGE_CURVE ( 'NONE', #31490, #32836, #3353, .T. ) ;
#16021 = CARTESIAN_POINT ( 'NONE',  ( 10.00000000000000000, 41.76106447765489094, 62.50884508063442269 ) ) ;
#16022 = DIRECTION ( 'NONE',  ( 0.5200609990132993854, 0.8541291221503275466, 0.000000000000000000 ) ) ;
#16023 = ORIENTED_EDGE ( 'NONE', *, *, #26424, .F. ) ;
#16024 = ORIENTED_EDGE ( 'NONE', *, *, #45581, .F. ) ;
#16025 = VECTOR ( 'NONE', #19179, 1000.000000000000000 ) ;
#16026 = EDGE_CURVE ( 'NONE', #4179, #17031, #21728, .T. ) ;
#16027 = EDGE_CURVE ( 'NONE', #36913, #5880, #15192, .T. ) ;
#16028 = DIRECTION ( 'NONE',  ( 0.000000000000000000, 0.3090169943749480619, -0.9510565162951533091 ) ) ;
#16029 = VERTEX_POINT ( 'NONE', #48158 ) ;
#16030 = VECTOR ( 'NONE', #14540, 1000.000000000000227 ) ;
#16031 = AXIS2_PLACEMENT_3D ( 'NONE', #3292, #11141, #14326 ) ;
#16032 = VECTOR ( 'NONE', #18081, 1000.000000000000000 ) ;
#16033 = ORIENTED_EDGE ( 'NONE', *, *, #39121, .T. ) ;
#16034 = ADVANCED_FACE ( 'NONE', ( #25872 ), #15114, .T. ) ;
#16035 = ORIENTED_EDGE ( 'NONE', *, *, #5985, .F. ) ;
#16036 = CIRCLE ( 'NONE', #14462, 37.49900000000000233 ) ;
#16037 = ADVANCED_FACE ( 'NONE', ( #3108 ), #14640, .F. ) ;
#16038 = AXIS2_PLACEMENT_3D ( 'NONE', #32588, #29410, #44568 ) ;
#16039 = ADVANCED_FACE ( 'NONE', ( #44249 ), #11458, .F. ) ;
#16040 = CYLINDRICAL_SURFACE ( 'NONE', #42581, 77.49899999999999523 ) ;
#16041 = PLANE ( 'NONE',  #21106 ) ;
#16042 = CARTESIAN_POINT ( 'NONE',  ( 10.00000000000000000, 26.02418014898310261, 70.52718814184268581 ) ) ;
#16043 = ORIENTED_EDGE ( 'NONE', *, *, #2208, .T. ) ;
#16044 = DIRECTION ( 'NONE',  ( -1.000000000000000000, -0.000000000000000000, 0.000000000000000000 ) ) ;
#16045 = VECTOR ( 'NONE', #11982, 1000.000000000000000 ) ;
#16046 = ADVANCED_FACE ( 'NONE', ( #47901 ), #7272, .T. ) ;
#16047 = EDGE_LOOP ( 'NONE', ( #13760, #12482, #30302, #40186 ) ) ;
#16048 = ORIENTED_EDGE ( 'NONE', *, *, #24217, .T. ) ;
#16049 = CARTESIAN_POINT ( 'NONE',  ( 0.000000000000000000, 8.688484142254221609, -21.88630264137359660 ) ) ;
#16050 = FACE_OUTER_BOUND ( 'NONE', #13223, .T. ) ;
#16051 = CARTESIAN_POINT ( 'NONE',  ( 10.00000000000000000, 0.000000000000000000, 0.000000000000000000 ) ) ;
#16052 = CIRCLE ( 'NONE', #4359, 31.99999999999998579 ) ;
#16053 = ORIENTED_EDGE ( 'NONE', *, *, #43851, .F. ) ;
#16054 = ORIENTED_EDGE ( 'NONE', *, *, #8302, .T. ) ;
#16055 = ORIENTED_EDGE ( 'NONE', *, *, #18477, .F. ) ;
#16056 = DIRECTION ( 'NONE',  ( -1.000000000000000000, -0.000000000000000000, -0.000000000000000000 ) ) ;
#16057 = VERTEX_POINT ( 'NONE', #2883 ) ;
#16058 = AXIS2_PLACEMENT_3D ( 'NONE', #37726, #26, #3959 ) ;
#16059 = CARTESIAN_POINT ( 'NONE',  ( 10.00000000000000000, 31.47745569255140552, 68.26794271651274926 ) ) ;
#16060 = FACE_OUTER_BOUND ( 'NONE', #13356, .T. ) ;
#16061 = CARTESIAN_POINT ( 'NONE',  ( -3.000000000000000000, -14.54903810567645195, -22.19967320028775504 ) ) ;
#16062 = CARTESIAN_POINT ( 'NONE',  ( -21.67772167707813935, -110.8034581014852762, -2.500000000000000000 ) ) ;
#16063 = LINE ( 'NONE', #37601, #21973 ) ;
#16064 = DIRECTION ( 'NONE',  ( -0.3311129884571280546, -0.9435911131814402886, 0.000000000000000000 ) ) ;
#16065 = LINE ( 'NONE', #8693, #45537 ) ;
#16066 = VERTEX_POINT ( 'NONE', #10474 ) ;
#16067 = DIRECTION ( 'NONE',  ( 0.000000000000000000, 0.000000000000000000, 1.000000000000000000 ) ) ;
#16068 = DIRECTION ( 'NONE',  ( -1.000000000000000000, 0.000000000000000000, -0.000000000000000000 ) ) ;
#16069 = CARTESIAN_POINT ( 'NONE',  ( 10.00000000000000000, 5.202137450156907761, -37.22597642581151689 ) ) ;
#16070 = DIRECTION ( 'NONE',  ( -1.000000000000000000, 0.000000000000000000, 0.000000000000000000 ) ) ;
#16071 = VECTOR ( 'NONE', #36729, 1000.000000000000000 ) ;
#16072 = AXIS2_PLACEMENT_3D ( 'NONE', #36829, #48100, #29499 ) ;
#16073 = ORIENTED_EDGE ( 'NONE', *, *, #29336, .T. ) ;
#16074 = ORIENTED_EDGE ( 'NONE', *, *, #47616, .F. ) ;
#16075 = CARTESIAN_POINT ( 'NONE',  ( -3.961125083139900749, -143.2122702051246677, -5.500000000000000000 ) ) ;
#16076 = AXIS2_PLACEMENT_3D ( 'NONE', #41471, #33158, #591 ) ;
#16077 = DIRECTION ( 'NONE',  ( 0.000000000000000000, -0.8910065241883722287, 0.4539904997395382003 ) ) ;
#16078 = DIRECTION ( 'NONE',  ( 0.000000000000000000, 0.3090169943749461745, -0.9510565162951539753 ) ) ;
#16079 = CARTESIAN_POINT ( 'NONE',  ( 0.000000000000000000, 77.19088730480532945, -6.903761155836932062 ) ) ;
#16080 = AXIS2_PLACEMENT_3D ( 'NONE', #11898, #8220, #23151 ) ;
#16081 = CIRCLE ( 'NONE', #43435, 31.99999999999998579 ) ;
#16082 = EDGE_CURVE ( 'NONE', #18399, #15510, #34705, .T. ) ;
#16083 = DIRECTION ( 'NONE',  ( -1.000000000000000000, -0.000000000000000000, -0.000000000000000000 ) ) ;
#16084 = CARTESIAN_POINT ( 'NONE',  ( 0.000000000000000000, 46.53671651293948486, 59.03961581697416250 ) ) ;
#16085 = EDGE_LOOP ( 'NONE', ( #42102, #43715, #13331, #1946 ) ) ;
#16087 = EDGE_CURVE ( 'NONE', #31329, #2031, #35480, .T. ) ;
#16086 = AXIS2_PLACEMENT_3D ( 'NONE', #32843, #43639, #47541 ) ;
#16088 = DIRECTION ( 'NONE',  ( -1.000000000000000000, -0.000000000000000000, -0.000000000000000000 ) ) ;
#16089 = LINE ( 'NONE', #41789, #32629 ) ;
#16090 = ORIENTED_EDGE ( 'NONE', *, *, #28466, .F. ) ;
#16091 = EDGE_CURVE ( 'NONE', #43487, #33738, #18762, .T. ) ;
#16092 = CIRCLE ( 'NONE', #32503, 77.49900000000000944 ) ;
#16093 = EDGE_LOOP ( 'NONE', ( #7427, #44573, #23801, #44014 ) ) ;
#16094 =( NAMED_UNIT ( * ) SI_UNIT ( $, .STERADIAN. ) SOLID_ANGLE_UNIT ( ) );
#16095 = EDGE_CURVE ( 'NONE', #37458, #32278, #47976, .T. ) ;
#16096 = CARTESIAN_POINT ( 'NONE',  ( 0.000000000000000000, -22.90783923731575200, -78.73519480814978522 ) ) ;
#16097 = VERTEX_POINT ( 'NONE', #47656 ) ;
#16098 = AXIS2_PLACEMENT_3D ( 'NONE', #33343, #22070, #26976 ) ;
#16099 = VERTEX_POINT ( 'NONE', #29794 ) ;
#16100 = ADVANCED_FACE ( 'NONE', ( #41074 ), #44721, .T. ) ;
#16101 = ORIENTED_EDGE ( 'NONE', *, *, #14758, .F. ) ;
#16102 = EDGE_CURVE ( 'NONE', #25704, #12511, #25391, .T. ) ;
#16103 = EDGE_CURVE ( 'NONE', #2158, #47361, #26377, .T. ) ;
#16104 = EDGE_LOOP ( 'NONE', ( #2293, #38837, #7477, #35632 ) ) ;
#16105 = CIRCLE ( 'NONE', #41889, 16.00000000000000355 ) ;
#16106 = CARTESIAN_POINT ( 'NONE',  ( 11.99999999999999822, 75.11764819372149304, -2.946379043146603482 ) ) ;
#16107 = DIRECTION ( 'NONE',  ( 0.000000000000000000, 0.1564344650402244019, 0.9876883405951387696 ) ) ;
#16108 = ORIENTED_EDGE ( 'NONE', *, *, #11620, .T. ) ;
#16109 = EDGE_LOOP ( 'NONE', ( #36538, #15136 ) ) ;
#16110 = AXIS2_PLACEMENT_3D ( 'NONE', #29661, #22802, #32839 ) ;
#16111 = ORIENTED_EDGE ( 'NONE', *, *, #16588, .F. ) ;
#16112 = AXIS2_PLACEMENT_3D ( 'NONE', #10642, #4017, #37536 ) ;
#16113 = CARTESIAN_POINT ( 'NONE',  ( 10.00000000000000000, 73.72996012237440766, 14.67089635893739619 ) ) ;
#16114 = EDGE_CURVE ( 'NONE', #29882, #35670, #7761, .T. ) ;
#16116 = VERTEX_POINT ( 'NONE', #40349 ) ;
#16115 = CARTESIAN_POINT ( 'NONE',  ( 10.00000000000000000, -63.18004540532994184, -44.88180994100446952 ) ) ;
#16117 = CARTESIAN_POINT ( 'NONE',  ( 10.00000000000000000, 37.58145647212453611, 16.68533520207917675 ) ) ;
#16118 = ORIENTED_EDGE ( 'NONE', *, *, #39202, .T. ) ;
#16119 = VECTOR ( 'NONE', #37562, 1000.000000000000000 ) ;
#16120 = CARTESIAN_POINT ( 'NONE',  ( 15.00000000000000000, 22.07842321921480888, -8.187992925817425771 ) ) ;
#16121 = EDGE_LOOP ( 'NONE', ( #42410, #33420, #3077, #32947 ) ) ;
#16122 = ORIENTED_EDGE ( 'NONE', *, *, #46924, .F. ) ;
#16123 = CARTESIAN_POINT ( 'NONE',  ( 11.99999999999999822, -81.96053171279903893, 2.543863470248101333 ) ) ;
#16124 = CARTESIAN_POINT ( 'NONE',  ( 11.99999999999999822, -46.11716303203136391, -67.80270845531939017 ) ) ;
#16125 = ORIENTED_EDGE ( 'NONE', *, *, #33918, .F. ) ;
#16126 = AXIS2_PLACEMENT_3D ( 'NONE', #36532, #10338, #6918 ) ;
#16127 = CARTESIAN_POINT ( 'NONE',  ( 11.99999999999999822, 0.000000000000000000, 0.000000000000000000 ) ) ;
#16128 = DIRECTION ( 'NONE',  ( 0.000000000000000000, 0.000000000000000000, 1.000000000000000000 ) ) ;
#16129 = DIRECTION ( 'NONE',  ( 0.000000000000000000, 0.6691306063588661202, 0.7431448254773871387 ) ) ;
#16130 = AXIS2_PLACEMENT_3D ( 'NONE', #33408, #10660, #43937 ) ;
#16131 = ORIENTED_EDGE ( 'NONE', *, *, #11398, .F. ) ;
#16132 = DIRECTION ( 'NONE',  ( -1.000000000000000000, -0.000000000000000000, -0.000000000000000000 ) ) ;
#16133 = AXIS2_PLACEMENT_3D ( 'NONE', #24963, #39909, #17622 ) ;
#16134 = DIRECTION ( 'NONE',  ( 0.000000000000000000, -0.9723699203976741146, -0.2334453638559159938 ) ) ;
#16135 = ORIENTED_EDGE ( 'NONE', *, *, #27683, .T. ) ;
#16136 = CYLINDRICAL_SURFACE ( 'NONE', #33768, 31.99999999999998579 ) ;
#16137 = VERTEX_POINT ( 'NONE', #3801 ) ;
#16138 = CARTESIAN_POINT ( 'NONE',  ( 10.00000000000000000, 44.88180994100376608, 63.18004540533043922 ) ) ;
#16139 = DIRECTION ( 'NONE',  ( -1.000000000000000000, -0.000000000000000000, 0.000000000000000000 ) ) ;
#16140 = DIRECTION ( 'NONE',  ( -1.000000000000000000, -0.000000000000000000, -0.000000000000000000 ) ) ;
#16141 = CARTESIAN_POINT ( 'NONE',  ( 11.99999999999999822, -0.8261519478436571973, 77.49459641780886443 ) ) ;
#16142 = CARTESIAN_POINT ( 'NONE',  ( 11.99999999999999822, -73.72996012237429397, -14.67089635893794508 ) ) ;
#16143 = DIRECTION ( 'NONE',  ( -1.000000000000000000, -0.000000000000000000, 0.000000000000000000 ) ) ;
#16144 = VECTOR ( 'NONE', #6068, 1000.000000000000000 ) ;
#16145 = CARTESIAN_POINT ( 'NONE',  ( 0.000000000000000000, 0.000000000000000000, 0.000000000000000000 ) ) ;
#16146 = FACE_OUTER_BOUND ( 'NONE', #45174, .T. ) ;
#16147 = EDGE_CURVE ( 'NONE', #39227, #28808, #19853, .T. ) ;
#16148 = CIRCLE ( 'NONE', #13034, 31.99999999999999645 ) ;
#16149 = CARTESIAN_POINT ( 'NONE',  ( 10.00000000000000000, -71.27951684758005513, -30.41916302227188851 ) ) ;
#16150 = EDGE_CURVE ( 'NONE', #2760, #4312, #25335, .T. ) ;
#16151 = ORIENTED_EDGE ( 'NONE', *, *, #21841, .F. ) ;
#16152 = EDGE_LOOP ( 'NONE', ( #17641, #14948, #9535, #28608, #28788, #42030 ) ) ;
#16153 = AXIS2_PLACEMENT_3D ( 'NONE', #38896, #35198, #45488 ) ;
#16154 = CARTESIAN_POINT ( 'NONE',  ( 0.000000000000000000, 0.000000000000000000, 52.00000000000002132 ) ) ;
#16155 = DIRECTION ( 'NONE',  ( 0.000000000000000000, 0.000000000000000000, 1.000000000000000000 ) ) ;
#16156 = CIRCLE ( 'NONE', #5994, 82.00000000000000000 ) ;
#16157 = DIRECTION ( 'NONE',  ( 0.000000000000000000, 6.938893903907229364E-16, 1.000000000000000000 ) ) ;
#16158 = ORIENTED_EDGE ( 'NONE', *, *, #18157, .T. ) ;
#16159 = ADVANCED_FACE ( 'NONE', ( #5082 ), #30130, .T. ) ;
#16160 = EDGE_CURVE ( 'NONE', #3407, #1420, #19997, .T. ) ;
#16161 = AXIS2_PLACEMENT_3D ( 'NONE', #23179, #26375, #15590 ) ;
#16162 = ORIENTED_EDGE ( 'NONE', *, *, #39486, .T. ) ;
#16163 = EDGE_CURVE ( 'NONE', #19053, #13639, #4259, .T. ) ;
#16164 = DIRECTION ( 'NONE',  ( -1.000000000000000000, 0.000000000000000000, -0.000000000000000000 ) ) ;
#16165 = ORIENTED_EDGE ( 'NONE', *, *, #35301, .T. ) ;
#16166 = ORIENTED_EDGE ( 'NONE', *, *, #8554, .T. ) ;
#16167 = VERTEX_POINT ( 'NONE', #38619 ) ;
#16168 = ORIENTED_EDGE ( 'NONE', *, *, #38852, .F. ) ;
#16169 = ADVANCED_FACE ( 'NONE', ( #38862 ), #34931, .F. ) ;
#16170 = VECTOR ( 'NONE', #37595, 1000.000000000000000 ) ;
#16171 = DIRECTION ( 'NONE',  ( 1.000000000000000000, 0.000000000000000000, 0.000000000000000000 ) ) ;
#16172 = ORIENTED_EDGE ( 'NONE', *, *, #43605, .T. ) ;
#16173 = DIRECTION ( 'NONE',  ( 0.000000000000000000, 0.000000000000000000, 1.000000000000000000 ) ) ;
#16174 = ORIENTED_EDGE ( 'NONE', *, *, #31452, .T. ) ;
#16175 = DIRECTION ( 'NONE',  ( 0.000000000000000000, -0.7071067811865389130, -0.7071067811865563435 ) ) ;
#16176 = AXIS2_PLACEMENT_3D ( 'NONE', #39853, #24913, #13419 ) ;
#16177 = DIRECTION ( 'NONE',  ( -0.000000000000000000, -0.3090169943749448977, -0.9510565162951543083 ) ) ;
#16178 = CARTESIAN_POINT ( 'NONE',  ( 10.00000000000000000, 0.000000000000000000, 0.000000000000000000 ) ) ;
#16179 = ORIENTED_EDGE ( 'NONE', *, *, #8334, .F. ) ;
#16180 = CARTESIAN_POINT ( 'NONE',  ( 0.000000000000000000, 0.000000000000000000, 0.000000000000000000 ) ) ;
#16181 = EDGE_LOOP ( 'NONE', ( #16779, #42840, #37202, #17105 ) ) ;
#16182 = CYLINDRICAL_SURFACE ( 'NONE', #41434, 31.99999999999999289 ) ;
#16183 = CARTESIAN_POINT ( 'NONE',  ( 10.00000000000000000, -21.32104025579135964, 30.84782396557210760 ) ) ;
#16184 = ORIENTED_EDGE ( 'NONE', *, *, #39138, .T. ) ;
#16185 = VECTOR ( 'NONE', #9612, 1000.000000000000000 ) ;
#16186 = CYLINDRICAL_SURFACE ( 'NONE', #23290, 31.99999999999999289 ) ;
#16187 = ORIENTED_EDGE ( 'NONE', *, *, #16686, .F. ) ;
#16188 = VERTEX_POINT ( 'NONE', #18615 ) ;
#16189 = LINE ( 'NONE', #31119, #45562 ) ;
#16190 = FACE_OUTER_BOUND ( 'NONE', #18618, .T. ) ;
#16191 = ORIENTED_EDGE ( 'NONE', *, *, #10842, .F. ) ;
#16192 = CARTESIAN_POINT ( 'NONE',  ( 10.00000000000000000, 0.000000000000000000, 0.000000000000000000 ) ) ;
#16193 = DIRECTION ( 'NONE',  ( 0.000000000000000000, 0.2334453638558990629, 0.9723699203976782224 ) ) ;
#16194 = CYLINDRICAL_SURFACE ( 'NONE', #32349, 77.49899999999999523 ) ;
#16195 = LINE ( 'NONE', #11788, #10114 ) ;
#16196 = LINE ( 'NONE', #38222, #16504 ) ;
#16197 = AXIS2_PLACEMENT_3D ( 'NONE', #13130, #1138, #38595 ) ;
#16198 = DIRECTION ( 'NONE',  ( 0.000000000000000000, 0.5877852522924743583, -0.8090169943749466741 ) ) ;
#16199 = LINE ( 'NONE', #3969, #45787 ) ;
#16200 = CARTESIAN_POINT ( 'NONE',  ( 15.00000000000000000, -11.95096189432345746, -23.69967320028757030 ) ) ;
#16201 = CARTESIAN_POINT ( 'NONE',  ( 24.94940289813197509, -237.3777120880564553, 5.500000000000000000 ) ) ;
#16202 = EDGE_CURVE ( 'NONE', #48350, #6120, #37866, .T. ) ;
#16203 = ADVANCED_FACE ( 'NONE', ( #20240 ), #31042, .T. ) ;
#16204 = DIRECTION ( 'NONE',  ( 0.000000000000000000, 0.000000000000000000, 1.000000000000000000 ) ) ;
#16205 = CARTESIAN_POINT ( 'NONE',  ( 0.000000000000000000, 46.54456581323805153, 59.03342792756280488 ) ) ;
#16206 = DIRECTION ( 'NONE',  ( -1.000000000000000000, 0.000000000000000000, 0.000000000000000000 ) ) ;
#16207 = ADVANCED_FACE ( 'NONE', ( #27594 ), #33541, .T. ) ;
#16208 = FACE_OUTER_BOUND ( 'NONE', #48120, .T. ) ;
#16209 = EDGE_CURVE ( 'NONE', #20931, #28111, #16334, .T. ) ;
#16210 = ORIENTED_EDGE ( 'NONE', *, *, #9448, .F. ) ;
#16211 = ORIENTED_EDGE ( 'NONE', *, *, #13173, .T. ) ;
#16212 = AXIS2_PLACEMENT_3D ( 'NONE', #12093, #4726, #27018 ) ;
#16213 = CARTESIAN_POINT ( 'NONE',  ( 0.000000000000000000, 16.65972982744934683, 80.28980883073764119 ) ) ;
#16214 = EDGE_CURVE ( 'NONE', #40594, #15144, #26212, .T. ) ;
#16215 = ORIENTED_EDGE ( 'NONE', *, *, #47311, .F. ) ;
#16216 = ADVANCED_FACE ( 'NONE', ( #14952 ), #42278, .T. ) ;
#16217 = CARTESIAN_POINT ( 'NONE',  ( 10.00000000000000000, 21.32104025579114648, 30.84782396557224970 ) ) ;
#16218 = APPLICATION_PROTOCOL_DEFINITION ( 'draft international standard', 'automotive_design', 1998, #6638 ) ;
#16219 = AXIS2_PLACEMENT_3D ( 'NONE', #9497, #9981, #2619 ) ;
#16220 = LINE ( 'NONE', #31149, #44809 ) ;
#16221 = ORIENTED_EDGE ( 'NONE', *, *, #33483, .F. ) ;
#16222 = AXIS2_PLACEMENT_3D ( 'NONE', #48271, #41650, #37257 ) ;
#16223 = EDGE_CURVE ( 'NONE', #22722, #28723, #11276, .T. ) ;
#16224 = FACE_OUTER_BOUND ( 'NONE', #13883, .T. ) ;
#16225 = ORIENTED_EDGE ( 'NONE', *, *, #15724, .F. ) ;
#16226 = AXIS2_PLACEMENT_3D ( 'NONE', #39692, #17379, #45626 ) ;
#16227 = EDGE_CURVE ( 'NONE', #13807, #21898, #22970, .T. ) ;
#16228 = DIRECTION ( 'NONE',  ( -1.000000000000000000, -0.000000000000000000, 0.000000000000000000 ) ) ;
#16229 = CARTESIAN_POINT ( 'NONE',  ( 10.00000000000000000, -30.80686688397025108, 21.53537804866070715 ) ) ;
#16230 = VERTEX_POINT ( 'NONE', #44559 ) ;
#16231 = CARTESIAN_POINT ( 'NONE',  ( 15.00000000000000000, -10.45096189432344502, -21.10159698893425784 ) ) ;
#16232 = ORIENTED_EDGE ( 'NONE', *, *, #37311, .F. ) ;
#16233 = ORIENTED_EDGE ( 'NONE', *, *, #47249, .F. ) ;
#16234 = EDGE_CURVE ( 'NONE', #33766, #9506, #23673, .T. ) ;
#16235 = FACE_OUTER_BOUND ( 'NONE', #30110, .T. ) ;
#16236 = CYLINDRICAL_SURFACE ( 'NONE', #40210, 16.00000000000000000 ) ;
#16237 = DIRECTION ( 'NONE',  ( 1.000000000000000000, 0.000000000000000000, -0.000000000000000000 ) ) ;
#16238 = DIRECTION ( 'NONE',  ( 1.000000000000000000, 0.000000000000000000, 0.000000000000000000 ) ) ;
#16239 = EDGE_CURVE ( 'NONE', #29827, #15289, #41150, .T. ) ;
#16241 = CARTESIAN_POINT ( 'NONE',  ( 12.50000000000000000, -132.5000000000000000, 40.00000000000000000 ) ) ;
#16240 = AXIS2_PLACEMENT_3D ( 'NONE', #8345, #23278, #33791 ) ;
#16242 = VERTEX_POINT ( 'NONE', #8495 ) ;
#16243 = CARTESIAN_POINT ( 'NONE',  ( 10.00000000000000000, -27.13269053701078448, -25.88420570971428702 ) ) ;
#16244 = EDGE_LOOP ( 'NONE', ( #16937, #21607, #37851, #24952 ) ) ;
#16245 = ORIENTED_EDGE ( 'NONE', *, *, #28069, .T. ) ;
#16246 = CARTESIAN_POINT ( 'NONE',  ( 0.000000000000000000, 0.000000000000000000, 52.00000000000002132 ) ) ;
#16247 = CIRCLE ( 'NONE', #18569, 15.99999999999999822 ) ;
#16248 = CARTESIAN_POINT ( 'NONE',  ( 0.000000000000000000, -26.02418014898260878, -70.52718814184285634 ) ) ;
#16249 = DIRECTION ( 'NONE',  ( -0.000000000000000000, -1.000000000000000000, -0.000000000000000000 ) ) ;
#16250 = CARTESIAN_POINT ( 'NONE',  ( 10.00000000000000000, 21.32104025579114648, 30.84782396557224970 ) ) ;
#16251 = ORIENTED_EDGE ( 'NONE', *, *, #20509, .F. ) ;
#16252 = DIRECTION ( 'NONE',  ( -1.000000000000000000, -0.000000000000000000, 0.000000000000000000 ) ) ;
#16253 = CARTESIAN_POINT ( 'NONE',  ( 10.00000000000000000, 31.52238457039638320, -27.75498641678709788 ) ) ;
#16254 = DIRECTION ( 'NONE',  ( 0.000000000000000000, 0.000000000000000000, 1.000000000000000000 ) ) ;
#16255 = CARTESIAN_POINT ( 'NONE',  ( 10.00000000000000000, 0.000000000000000000, 0.000000000000000000 ) ) ;
#16256 = EDGE_CURVE ( 'NONE', #26232, #37461, #23428, .T. ) ;
#16257 = CARTESIAN_POINT ( 'NONE',  ( 0.000000000000000000, 12.24744871391589207, -2.500000000000000000 ) ) ;
#16258 = AXIS2_PLACEMENT_3D ( 'NONE', #19480, #45695, #8713 ) ;
#16259 = LINE ( 'NONE', #45616, #14472 ) ;
#16260 = CARTESIAN_POINT ( 'NONE',  ( 0.000000000000000000, -24.73286445877757345, 73.44644590900053061 ) ) ;
#16261 = DIRECTION ( 'NONE',  ( 0.000000000000000000, 0.000000000000000000, 1.000000000000000000 ) ) ;
#16262 = EDGE_CURVE ( 'NONE', #46617, #9384, #37048, .T. ) ;
#16263 = CARTESIAN_POINT ( 'NONE',  ( 10.00000000000000000, 33.71516098798738881, 74.74816331893441657 ) ) ;
#16264 = FACE_OUTER_BOUND ( 'NONE', #24418, .T. ) ;
#16265 = EDGE_CURVE ( 'NONE', #37023, #23034, #35889, .T. ) ;
#16266 = ORIENTED_EDGE ( 'NONE', *, *, #7662, .F. ) ;
#16267 = VECTOR ( 'NONE', #37444, 1000.000000000000227 ) ;
#16268 = VERTEX_POINT ( 'NONE', #20733 ) ;
#16269 = CYLINDRICAL_SURFACE ( 'NONE', #31656, 16.00000000000000000 ) ;
#16270 = EDGE_LOOP ( 'NONE', ( #45415, #28292, #7339, #47446 ) ) ;
#16271 = ORIENTED_EDGE ( 'NONE', *, *, #24823, .T. ) ;
#16272 = EDGE_CURVE ( 'NONE', #1412, #19636, #2591, .T. ) ;
#16273 = CARTESIAN_POINT ( 'NONE',  ( 0.000000000000000000, 0.000000000000000000, 0.000000000000000000 ) ) ;
#16274 = CARTESIAN_POINT ( 'NONE',  ( 10.00000000000000000, 0.000000000000000000, 0.000000000000000000 ) ) ;
#16275 = ORIENTED_EDGE ( 'NONE', *, *, #16227, .F. ) ;
#16276 = VECTOR ( 'NONE', #3232, 1000.000000000000000 ) ;
#16277 = ORIENTED_EDGE ( 'NONE', *, *, #27478, .T. ) ;
#16278 = CIRCLE ( 'NONE', #40489, 42.00000000000000000 ) ;
#16279 = ORIENTED_EDGE ( 'NONE', *, *, #15917, .T. ) ;
#16280 = CARTESIAN_POINT ( 'NONE',  ( 11.99999999999999822, 2.946379043146343246, 75.11764819372150725 ) ) ;
#16281 = DIRECTION ( 'NONE',  ( 0.000000000000000000, -1.000000000000000000, -1.040834085586084257E-14 ) ) ;
#16282 = PLANE ( 'NONE',  #44144 ) ;
#16283 = ORIENTED_EDGE ( 'NONE', *, *, #32293, .F. ) ;
#16284 = CARTESIAN_POINT ( 'NONE',  ( 0.000000000000000000, 0.000000000000000000, 0.000000000000000000 ) ) ;
#16285 = ORIENTED_EDGE ( 'NONE', *, *, #4685, .T. ) ;
#16286 = VERTEX_POINT ( 'NONE', #31775 ) ;
#16287 = DIRECTION ( 'NONE',  ( -1.000000000000000000, 0.000000000000000000, 0.000000000000000000 ) ) ;
#16288 = DIRECTION ( 'NONE',  ( -1.000000000000000000, 0.000000000000000000, 0.000000000000000000 ) ) ;
#16289 = DIRECTION ( 'NONE',  ( 0.000000000000000000, -0.7431448254773862505, 0.6691306063588672304 ) ) ;
#16290 = AXIS2_PLACEMENT_3D ( 'NONE', #39916, #20577, #9325 ) ;
#16291 = VERTEX_POINT ( 'NONE', #47153 ) ;
#16292 = ORIENTED_EDGE ( 'NONE', *, *, #10459, .F. ) ;
#16293 = ORIENTED_EDGE ( 'NONE', *, *, #19603, .T. ) ;
#16294 = CARTESIAN_POINT ( 'NONE',  ( 5.000000000000000000, 59.75363087400076267, 56.15606465354979804 ) ) ;
#16295 = ORIENTED_EDGE ( 'NONE', *, *, #30622, .T. ) ;
#16296 = DIRECTION ( 'NONE',  ( 0.6862798483830534479, 0.7273375899149810975, 0.000000000000000000 ) ) ;
#16297 = LINE ( 'NONE', #27079, #43647 ) ;
#16298 = CARTESIAN_POINT ( 'NONE',  ( -3.000000000000000000, -1.278221433540502217, 26.51162292216071847 ) ) ;
#16299 = DIRECTION ( 'NONE',  ( -1.000000000000000000, 0.000000000000000000, 0.000000000000000000 ) ) ;
#16300 = DIRECTION ( 'NONE',  ( 0.000000000000000000, 0.000000000000000000, 1.000000000000000000 ) ) ;
#16301 = DIRECTION ( 'NONE',  ( -1.000000000000000000, -0.000000000000000000, -0.000000000000000000 ) ) ;
#16302 = DIRECTION ( 'NONE',  ( 0.5200609990132993854, 0.8541291221503275466, -0.000000000000000000 ) ) ;
#16303 = ORIENTED_EDGE ( 'NONE', *, *, #1619, .F. ) ;
#16304 = CARTESIAN_POINT ( 'NONE',  ( 0.000000000000000000, 31.47745569255237896, -68.26794271651228030 ) ) ;
#16305 = DIRECTION ( 'NONE',  ( -1.000000000000000000, 0.000000000000000000, 0.000000000000000000 ) ) ;
#16306 = CARTESIAN_POINT ( 'NONE',  ( 0.000000000000000000, -46.54456581323847786, 59.03342792756247093 ) ) ;
#16307 = FACE_OUTER_BOUND ( 'NONE', #29742, .T. ) ;
#16308 = ORIENTED_EDGE ( 'NONE', *, *, #14363, .T. ) ;
#16309 = PLANE ( 'NONE',  #43489 ) ;
#16310 = DIRECTION ( 'NONE',  ( 0.000000000000000000, 0.000000000000000000, 1.000000000000000000 ) ) ;
#16311 = DIRECTION ( 'NONE',  ( -1.000000000000000000, 0.000000000000000000, -0.000000000000000000 ) ) ;
#16312 = DIRECTION ( 'NONE',  ( -1.000000000000000000, 0.000000000000000000, 0.000000000000000000 ) ) ;
#16313 = ADVANCED_FACE ( 'NONE', ( #42772 ), #13624, .F. ) ;
#16314 = CIRCLE ( 'NONE', #8478, 37.49900000000000233 ) ;
#16315 = CARTESIAN_POINT ( 'NONE',  ( 10.00000000000000000, 0.000000000000000000, 0.000000000000000000 ) ) ;
#16316 = DIRECTION ( 'NONE',  ( -1.000000000000000000, 0.000000000000000000, 0.000000000000000000 ) ) ;
#16317 = EDGE_CURVE ( 'NONE', #7360, #13104, #8966, .T. ) ;
#16318 = DIRECTION ( 'NONE',  ( 0.000000000000000000, -1.000000000000000000, -1.047444401652940007E-14 ) ) ;
#16319 = DIRECTION ( 'NONE',  ( -1.000000000000000000, 0.000000000000000000, 0.000000000000000000 ) ) ;
#16320 = EDGE_LOOP ( 'NONE', ( #14733, #44083, #36982, #7497 ) ) ;
#16321 = EDGE_CURVE ( 'NONE', #37827, #4186, #39591, .T. ) ;
#16322 = ADVANCED_FACE ( 'NONE', ( #17049 ), #35408, .T. ) ;
#16323 = ORIENTED_EDGE ( 'NONE', *, *, #12291, .T. ) ;
#16324 = DIRECTION ( 'NONE',  ( 0.000000000000000000, 0.000000000000000000, 1.000000000000000000 ) ) ;
#16325 = LINE ( 'NONE', #27339, #30770 ) ;
#16326 = VERTEX_POINT ( 'NONE', #25109 ) ;
#16327 = VECTOR ( 'NONE', #32096, 1000.000000000000000 ) ;
#16328 = ORIENTED_EDGE ( 'NONE', *, *, #17008, .F. ) ;
#16329 = CYLINDRICAL_SURFACE ( 'NONE', #46075, 37.49900000000000233 ) ;
#16330 = VERTEX_POINT ( 'NONE', #39821 ) ;
#16331 = ORIENTED_EDGE ( 'NONE', *, *, #45098, .F. ) ;
#16332 = AXIS2_PLACEMENT_3D ( 'NONE', #25406, #14654, #40365 ) ;
#16333 = LINE ( 'NONE', #23671, #34343 ) ;
#16334 = LINE ( 'NONE', #3931, #1888 ) ;
#16335 = CIRCLE ( 'NONE', #38215, 82.00000000000000000 ) ;
#16336 = VERTEX_POINT ( 'NONE', #21446 ) ;
#16337 = ORIENTED_EDGE ( 'NONE', *, *, #21370, .T. ) ;
#16338 = AXIS2_PLACEMENT_3D ( 'NONE', #18994, #8237, #23168 ) ;
#16339 = CIRCLE ( 'NONE', #31982, 16.00000000000000000 ) ;
#16340 = DIRECTION ( 'NONE',  ( 0.000000000000000000, 0.9238795325112877377, -0.3826834323650873948 ) ) ;
#16342 = ORIENTED_EDGE ( 'NONE', *, *, #39396, .F. ) ;
#16341 = LINE ( 'NONE', #31780, #17258 ) ;
#16343 = DIRECTION ( 'NONE',  ( -1.000000000000000000, 0.000000000000000000, 0.000000000000000000 ) ) ;
#16344 = EDGE_CURVE ( 'NONE', #1582, #7124, #28561, .T. ) ;
#16345 = EDGE_LOOP ( 'NONE', ( #39958, #11783, #3118, #42820 ) ) ;
#16346 = ORIENTED_EDGE ( 'NONE', *, *, #27366, .F. ) ;
#16347 = DIRECTION ( 'NONE',  ( 1.000000000000000000, 0.000000000000000000, 0.000000000000000000 ) ) ;
#16348 = ORIENTED_EDGE ( 'NONE', *, *, #47943, .T. ) ;
#16349 = ORIENTED_EDGE ( 'NONE', *, *, #7293, .F. ) ;
#16350 = DIRECTION ( 'NONE',  ( -1.000000000000000000, 0.000000000000000000, -0.000000000000000000 ) ) ;
#16351 = CYLINDRICAL_SURFACE ( 'NONE', #9244, 31.99999999999999289 ) ;
#16352 = EDGE_CURVE ( 'NONE', #43548, #47535, #31525, .T. ) ;
#16353 = ORIENTED_EDGE ( 'NONE', *, *, #34868, .F. ) ;
#16354 = CARTESIAN_POINT ( 'NONE',  ( 10.00000000000000000, -36.72794159290197769, -65.59268652807249111 ) ) ;
#16355 = DIRECTION ( 'NONE',  ( 0.000000000000000000, 0.9876883405951382144, -0.1564344650402276493 ) ) ;
#16356 = CYLINDRICAL_SURFACE ( 'NONE', #17393, 77.49899999999999523 ) ;
#16357 = EDGE_CURVE ( 'NONE', #21831, #37286, #11323, .T. ) ;
#16358 = VERTEX_POINT ( 'NONE', #43494 ) ;
#16359 = STYLED_ITEM ( 'NONE', ( #662 ), #37976 ) ;
#16360 = CARTESIAN_POINT ( 'NONE',  ( 11.99999999999999822, -77.49459641780886443, -0.8261519478439277586 ) ) ;
#16361 = CARTESIAN_POINT ( 'NONE',  ( 23.11608002360578240, -124.4885236261218182, 5.500000000000000000 ) ) ;
#16362 = ORIENTED_EDGE ( 'NONE', *, *, #77, .T. ) ;
#16363 = CARTESIAN_POINT ( 'NONE',  ( 16.84844760790522855, -103.5491698323862124, 5.500000000000000000 ) ) ;
#16364 = VERTEX_POINT ( 'NONE', #40055 ) ;
#16365 = DIRECTION ( 'NONE',  ( -1.000000000000000000, -0.000000000000000000, -0.000000000000000000 ) ) ;
#16366 = CARTESIAN_POINT ( 'NONE',  ( 4.999999999999999112, 16.65560815589411092, 38.55633173627015253 ) ) ;
#16367 = CARTESIAN_POINT ( 'NONE',  ( -10.00000000000000000, 0.000000000000000000, 0.000000000000000000 ) ) ;
#16368 = CARTESIAN_POINT ( 'NONE',  ( 10.00000000000000000, 0.000000000000000000, 0.000000000000000000 ) ) ;
#16369 = ADVANCED_FACE ( 'NONE', ( #13384 ), #16823, .T. ) ;
#16370 = ADVANCED_FACE ( 'NONE', ( #32473 ), #20969, .T. ) ;
#16371 = DIRECTION ( 'NONE',  ( -1.000000000000000000, 0.000000000000000000, -0.000000000000000000 ) ) ;
#16372 = CARTESIAN_POINT ( 'NONE',  ( -11.59999999999999787, 0.000000000000000000, 42.00000000000001421 ) ) ;
#16373 = VECTOR ( 'NONE', #16422, 1000.000000000000000 ) ;
#16374 = LINE ( 'NONE', #39629, #20838 ) ;
#16375 = VECTOR ( 'NONE', #44932, 1000.000000000000000 ) ;
#16376 = CARTESIAN_POINT ( 'NONE',  ( 1.233757462863572574, -119.1468631277289347, 2.500000000000000000 ) ) ;
#16377 = ORIENTED_EDGE ( 'NONE', *, *, #6452, .T. ) ;
#16378 = VECTOR ( 'NONE', #22475, 1000.000000000000000 ) ;
#16379 =( LENGTH_UNIT ( ) NAMED_UNIT ( * ) SI_UNIT ( .MILLI., .METRE. ) );
#16380 = PRODUCT_DEFINITION ( 'UNKNOWN', '', #3023, #21786 ) ;
#16381 = EDGE_LOOP ( 'NONE', ( #37018, #9155, #5261, #38103 ) ) ;
#16382 = AXIS2_PLACEMENT_3D ( 'NONE', #35903, #11368, #20980 ) ;
#16383 = DIRECTION ( 'NONE',  ( -1.000000000000000000, 0.000000000000000000, -0.000000000000000000 ) ) ;
#16384 = CARTESIAN_POINT ( 'NONE',  ( 11.99999999999999822, 68.26794271651307611, -31.47745569255064169 ) ) ;
#16385 = DIRECTION ( 'NONE',  ( 0.000000000000000000, 1.000000000000000000, -6.938893903907229364E-16 ) ) ;
#16386 = ORIENTED_EDGE ( 'NONE', *, *, #26424, .T. ) ;
#16387 = ORIENTED_EDGE ( 'NONE', *, *, #24090, .F. ) ;
#16388 = DIRECTION ( 'NONE',  ( -1.000000000000000000, 0.000000000000000000, -0.000000000000000000 ) ) ;
#16389 = ORIENTED_EDGE ( 'NONE', *, *, #7828, .F. ) ;
#16390 = ORIENTED_EDGE ( 'NONE', *, *, #30873, .F. ) ;
#16391 = ORIENTED_EDGE ( 'NONE', *, *, #48145, .T. ) ;
#16392 = VERTEX_POINT ( 'NONE', #5556 ) ;
#16393 = ORIENTED_EDGE ( 'NONE', *, *, #40682, .T. ) ;
#16394 = AXIS2_PLACEMENT_3D ( 'NONE', #36221, #14441, #32559 ) ;
#16395 = DIRECTION ( 'NONE',  ( 1.000000000000000000, -0.000000000000000000, -0.000000000000000000 ) ) ;
#16396 = EDGE_CURVE ( 'NONE', #35643, #26166, #47266, .T. ) ;
#16398 = ORIENTED_EDGE ( 'NONE', *, *, #20842, .T. ) ;
#16397 = AXIS2_PLACEMENT_3D ( 'NONE', #16991, #41991, #46861 ) ;
#16399 = CARTESIAN_POINT ( 'NONE',  ( 10.00000000000000000, -36.88895765772628010, -6.736453364083947015 ) ) ;
#16400 = ORIENTED_EDGE ( 'NONE', *, *, #4810, .T. ) ;
#16401 = DIRECTION ( 'NONE',  ( 1.000000000000000000, -0.000000000000000000, -0.000000000000000000 ) ) ;
#16403 = EDGE_CURVE ( 'NONE', #11961, #45643, #28076, .T. ) ;
#16402 = AXIS2_PLACEMENT_3D ( 'NONE', #9568, #28186, #45640 ) ;
#16404 = CARTESIAN_POINT ( 'NONE',  ( 0.000000000000000000, -12.42422080174663712, 35.38097989696507994 ) ) ;
#16405 = CYLINDRICAL_SURFACE ( 'NONE', #2517, 37.49900000000000233 ) ;
#16406 = EDGE_CURVE ( 'NONE', #24069, #25536, #23814, .T. ) ;
#16407 = ORIENTED_EDGE ( 'NONE', *, *, #36234, .F. ) ;
#16408 = VECTOR ( 'NONE', #26355, 1000.000000000000000 ) ;
#16409 = CARTESIAN_POINT ( 'NONE',  ( 0.000000000000000000, 0.000000000000000000, 0.000000000000000000 ) ) ;
#16410 = ORIENTED_EDGE ( 'NONE', *, *, #3692, .F. ) ;
#16411 = DIRECTION ( 'NONE',  ( -1.000000000000000000, -0.000000000000000000, -0.000000000000000000 ) ) ;
#16412 = DIRECTION ( 'NONE',  ( 0.000000000000000000, 0.000000000000000000, 1.000000000000000000 ) ) ;
#16413 = EDGE_LOOP ( 'NONE', ( #23843, #19099, #32074, #12082 ) ) ;
#16414 = DIRECTION ( 'NONE',  ( -1.000000000000000000, -0.000000000000000000, -0.000000000000000000 ) ) ;
#16415 = ORIENTED_EDGE ( 'NONE', *, *, #19618, .F. ) ;
#16416 = ORIENTED_EDGE ( 'NONE', *, *, #2964, .T. ) ;
#16417 = LINE ( 'NONE', #46279, #8788 ) ;
#16418 = LINE ( 'NONE', #45304, #9084 ) ;
#16419 = LINE ( 'NONE', #12514, #31650 ) ;
#16420 = CARTESIAN_POINT ( 'NONE',  ( 10.00000000000000000, 80.55351364060589958, 15.33399622253511829 ) ) ;
#16421 = LINE ( 'NONE', #31369, #5763 ) ;
#16422 = DIRECTION ( 'NONE',  ( -1.000000000000000000, -0.000000000000000000, 0.000000000000000000 ) ) ;
#16423 = EDGE_CURVE ( 'NONE', #46298, #39398, #4298, .T. ) ;
#16424 = CARTESIAN_POINT ( 'NONE',  ( 10.00000000000000000, 26.79245525562761188, -32.34446384429941901 ) ) ;
#16425 = EDGE_CURVE ( 'NONE', #4936, #15072, #31663, .T. ) ;
#16426 = CARTESIAN_POINT ( 'NONE',  ( 10.00000000000000000, 0.000000000000000000, 0.000000000000000000 ) ) ;
#16427 = ORIENTED_EDGE ( 'NONE', *, *, #11999, .F. ) ;
#16428 = CARTESIAN_POINT ( 'NONE',  ( 10.00000000000000000, 0.000000000000000000, 0.000000000000000000 ) ) ;
#16429 = CARTESIAN_POINT ( 'NONE',  ( 15.00000000000000000, 6.762365576493647445, 25.66652317338391498 ) ) ;
#16430 = CARTESIAN_POINT ( 'NONE',  ( 5.000000000000000000, 50.23322058963348979, 64.81221759200361987 ) ) ;
#16431 = CARTESIAN_POINT ( 'NONE',  ( 11.99999999999999822, 2.543863470248389103, 81.96053171279902472 ) ) ;
#16432 = CARTESIAN_POINT ( 'NONE',  ( 10.00000000000000000, 37.01155633439059756, 6.555932627142549762 ) ) ;
#16433 = DIRECTION ( 'NONE',  ( -1.000000000000000000, -0.000000000000000000, -0.000000000000000000 ) ) ;
#16434 = CARTESIAN_POINT ( 'NONE',  ( 10.00000000000000000, 5.202137450156907761, -37.22597642581151689 ) ) ;
#16435 = ORIENTED_EDGE ( 'NONE', *, *, #17228, .T. ) ;
#16436 = ADVANCED_FACE ( 'NONE', ( #22170 ), #7236, .F. ) ;
#16437 = AXIS2_PLACEMENT_3D ( 'NONE', #16284, #20920, #35351 ) ;
#16438 = CARTESIAN_POINT ( 'NONE',  ( 11.99999999999999822, 59.03342792756328095, -46.54456581323744757 ) ) ;
#16439 = VECTOR ( 'NONE', #27726, 1000.000000000000000 ) ;
#16440 = CYLINDRICAL_SURFACE ( 'NONE', #43993, 42.00000000000000000 ) ;
#16441 = AXIS2_PLACEMENT_3D ( 'NONE', #21159, #9916, #24841 ) ;
#16442 = AXIS2_PLACEMENT_3D ( 'NONE', #18845, #44562, #26693 ) ;
#16443 = ITEM_DEFINED_TRANSFORMATION ( 'NONE', 'NONE', #25654,  #11636 ) ;
#16444 = DIRECTION ( 'NONE',  ( -1.000000000000000000, -0.000000000000000000, 0.000000000000000000 ) ) ;
#16445 = ORIENTED_EDGE ( 'NONE', *, *, #26136, .F. ) ;
#16446 = AXIS2_PLACEMENT_3D ( 'NONE', #8859, #5439, #35048 ) ;
#16447 = CIRCLE ( 'NONE', #43794, 82.00000000000000000 ) ;
#16448 = AXIS2_PLACEMENT_3D ( 'NONE', #21757, #32546, #47469 ) ;
#16449 = DIRECTION ( 'NONE',  ( 0.000000000000000000, -6.938893903907231533E-15, 1.000000000000000000 ) ) ;
#16450 = ORIENTED_EDGE ( 'NONE', *, *, #21163, .T. ) ;
#16451 = LINE ( 'NONE', #31400, #42221 ) ;
#16452 = CARTESIAN_POINT ( 'NONE',  ( 0.000000000000000000, 0.000000000000000000, 0.000000000000000000 ) ) ;
#16453 = ORIENTED_EDGE ( 'NONE', *, *, #17551, .T. ) ;
#16454 = FACE_OUTER_BOUND ( 'NONE', #16954, .T. ) ;
#16455 = EDGE_LOOP ( 'NONE', ( #26688, #23606, #18120, #6398 ) ) ;
#16456 = CARTESIAN_POINT ( 'NONE',  ( 4.999999999999999112, 10.41901085202135491, -40.68715046381917944 ) ) ;
#16457 = ORIENTED_EDGE ( 'NONE', *, *, #7828, .T. ) ;
#16458 = ADVANCED_FACE ( 'NONE', ( #7719 ), #33429, .T. ) ;
#16459 = VERTEX_POINT ( 'NONE', #22419 ) ;
#16460 = EDGE_CURVE ( 'NONE', #17350, #39780, #42586, .T. ) ;
#16461 = DIRECTION ( 'NONE',  ( -1.000000000000000000, -0.000000000000000000, 0.000000000000000000 ) ) ;
#16462 = VERTEX_POINT ( 'NONE', #29518 ) ;
#16463 = ADVANCED_FACE ( 'NONE', ( #44444 ), #10430, .F. ) ;
#16464 = DIRECTION ( 'NONE',  ( 0.000000000000000000, 0.4539904997395478592, -0.8910065241883673437 ) ) ;
#16465 = DIRECTION ( 'NONE',  ( -0.9918136447140104561, 0.1276937514489679681, 0.000000000000000000 ) ) ;
#16466 = DIRECTION ( 'NONE',  ( 0.000000000000000000, 0.000000000000000000, -1.000000000000000000 ) ) ;
#16467 = ADVANCED_FACE ( 'NONE', ( #11158 ), #21688, .T. ) ;
#16468 = FACE_OUTER_BOUND ( 'NONE', #46938, .T. ) ;
#16469 = EDGE_LOOP ( 'NONE', ( #45226, #47442, #35795, #181 ) ) ;
#16470 = CARTESIAN_POINT ( 'NONE',  ( -12.50000000000000000, -107.5000000000000000, -2.500000000000000000 ) ) ;
#16471 = ORIENTED_EDGE ( 'NONE', *, *, #33237, .T. ) ;
#16472 = ORIENTED_EDGE ( 'NONE', *, *, #33810, .F. ) ;
#16473 = EDGE_CURVE ( 'NONE', #47238, #39281, #27740, .T. ) ;
#16474 = DIRECTION ( 'NONE',  ( 0.000000000000000000, 0.000000000000000000, 1.000000000000000000 ) ) ;
#16475 = AXIS2_PLACEMENT_3D ( 'NONE', #25015, #47534, #43399 ) ;
#16476 = ORIENTED_EDGE ( 'NONE', *, *, #17990, .T. ) ;
#16477 = AXIS2_PLACEMENT_3D ( 'NONE', #2192, #17828, #47677 ) ;
#16478 = DIRECTION ( 'NONE',  ( 0.000000000000000000, -0.7071067811865535679, 0.7071067811865414665 ) ) ;
#16479 = CARTESIAN_POINT ( 'NONE',  ( 24.95699195200416654, -110.9640411295978595, 5.500000000000000000 ) ) ;
#16480 = CYLINDRICAL_SURFACE ( 'NONE', #839, 82.00000000000000000 ) ;
#16481 = ORIENTED_EDGE ( 'NONE', *, *, #28773, .F. ) ;
#16482 = CARTESIAN_POINT ( 'NONE',  ( 10.00000000000000000, 36.88895765772633695, 6.736453364083687667 ) ) ;
#16483 = DIRECTION ( 'NONE',  ( -1.000000000000000000, 0.000000000000000000, -0.000000000000000000 ) ) ;
#16484 = AXIS2_PLACEMENT_3D ( 'NONE', #39936, #28681, #47985 ) ;
#16485 = CARTESIAN_POINT ( 'NONE',  ( 0.000000000000000000, 0.000000000000000000, 0.000000000000000000 ) ) ;
#16486 = EDGE_CURVE ( 'NONE', #6719, #25698, #3808, .T. ) ;
#16487 = CIRCLE ( 'NONE', #25060, 77.49899999999999523 ) ;
#16488 = CARTESIAN_POINT ( 'NONE',  ( 10.00000000000000000, -37.48860685352291711, 0.8828120875899322373 ) ) ;
#16489 = DIRECTION ( 'NONE',  ( -1.000000000000000000, 0.000000000000000000, 0.000000000000000000 ) ) ;
#16490 = VECTOR ( 'NONE', #29051, 1000.000000000000000 ) ;
#16491 = CARTESIAN_POINT ( 'NONE',  ( 0.000000000000000000, 69.42325613327489009, -34.44570377933524696 ) ) ;
#16492 = EDGE_CURVE ( 'NONE', #42004, #39534, #44679, .T. ) ;
#16493 = DIRECTION ( 'NONE',  ( -1.000000000000000000, 0.000000000000000000, 0.000000000000000000 ) ) ;
#16494 = DIRECTION ( 'NONE',  ( 0.000000000000000000, -0.9510565162951499785, -0.3090169943749582204 ) ) ;
#16495 = LINE ( 'NONE', #46606, #18957 ) ;
#16496 = CARTESIAN_POINT ( 'NONE',  ( 0.000000000000000000, 46.53671651293948486, 59.03961581697416250 ) ) ;
#16497 = ORIENTED_EDGE ( 'NONE', *, *, #37932, .F. ) ;
#16498 = EDGE_CURVE ( 'NONE', #27191, #26165, #8195, .T. ) ;
#16499 = CYLINDRICAL_SURFACE ( 'NONE', #17544, 16.00000000000000000 ) ;
#16500 = VERTEX_POINT ( 'NONE', #6766 ) ;
#16501 = DIRECTION ( 'NONE',  ( -1.000000000000000000, 0.000000000000000000, 0.000000000000000000 ) ) ;
#16502 = CARTESIAN_POINT ( 'NONE',  ( 0.000000000000000000, 0.000000000000000000, 40.80000000000001847 ) ) ;
#16503 = ORIENTED_EDGE ( 'NONE', *, *, #17245, .F. ) ;
#16504 = VECTOR ( 'NONE', #23287, 1000.000000000000000 ) ;
#16505 = ADVANCED_FACE ( 'NONE', ( #36607 ), #11417, .T. ) ;
#16506 = CIRCLE ( 'NONE', #43854, 31.99999999999999645 ) ;
#16507 = AXIS2_PLACEMENT_3D ( 'NONE', #30748, #4075, #33676 ) ;
#16508 = CIRCLE ( 'NONE', #7099, 31.99999999999999289 ) ;
#16509 = CARTESIAN_POINT ( 'NONE',  ( 0.000000000000000000, -80.28980883073747066, -16.65972982745018172 ) ) ;
#16510 = VERTEX_POINT ( 'NONE', #17768 ) ;
#16511 = ORIENTED_EDGE ( 'NONE', *, *, #15973, .T. ) ;
#16512 = DIRECTION ( 'NONE',  ( 0.000000000000000000, -0.9510565162951544194, -0.3090169943749450643 ) ) ;
#16513 = PRESENTATION_LAYER_ASSIGNMENT (  '', '', ( #31273 ) ) ;
#16514 = EDGE_CURVE ( 'NONE', #10059, #21026, #35524, .T. ) ;
#16515 = FACE_OUTER_BOUND ( 'NONE', #42522, .T. ) ;
#16516 = DIRECTION ( 'NONE',  ( 0.000000000000000000, -0.9876883405951359940, -0.1564344650402420545 ) ) ;
#16517 = VERTEX_POINT ( 'NONE', #43959 ) ;
#16518 = EDGE_CURVE ( 'NONE', #38732, #28147, #12892, .T. ) ;
#16519 = CARTESIAN_POINT ( 'NONE',  ( 0.000000000000000000, 0.000000000000000000, 0.000000000000000000 ) ) ;
#16520 = VERTEX_POINT ( 'NONE', #44208 ) ;
#16521 = EDGE_CURVE ( 'NONE', #38433, #23803, #21918, .T. ) ;
#16522 = CARTESIAN_POINT ( 'NONE',  ( 5.000000000000002665, 76.69515212746057387, -29.01471420065480089 ) ) ;
#16523 = CARTESIAN_POINT ( 'NONE',  ( 0.000000000000000000, 35.95386929396256903, -10.96151621346501237 ) ) ;
#16524 = DIRECTION ( 'NONE',  ( 0.000000000000000000, -0.3826834323650969427, 0.9238795325112838519 ) ) ;
#16525 = CIRCLE ( 'NONE', #20422, 11.59999999999999787 ) ;
#16526 = EDGE_LOOP ( 'NONE', ( #27596, #31762, #38264, #39139 ) ) ;
#16527 = ORIENTED_EDGE ( 'NONE', *, *, #34084, .F. ) ;
#16528 = VERTEX_POINT ( 'NONE', #18247 ) ;
#16529 = DIRECTION ( 'NONE',  ( -1.000000000000000000, 0.000000000000000000, 0.000000000000000000 ) ) ;
#16530 = ORIENTED_EDGE ( 'NONE', *, *, #36367, .F. ) ;
#16531 = EDGE_CURVE ( 'NONE', #6004, #38691, #15236, .T. ) ;
#16532 = CYLINDRICAL_SURFACE ( 'NONE', #41864, 31.99999999999999289 ) ;
#16533 = DIRECTION ( 'NONE',  ( -1.000000000000000000, -0.000000000000000000, -0.000000000000000000 ) ) ;
#16534 = CARTESIAN_POINT ( 'NONE',  ( 10.00000000000000000, -34.44570377933549565, -69.42325613327476219 ) ) ;
#16535 = DIRECTION ( 'NONE',  ( 0.000000000000000000, 0.000000000000000000, 1.000000000000000000 ) ) ;
#16536 = CYLINDRICAL_SURFACE ( 'NONE', #14202, 77.49899999999999523 ) ;
#16537 = DIRECTION ( 'NONE',  ( 0.000000000000000000, 0.000000000000000000, 1.000000000000000000 ) ) ;
#16538 = DIRECTION ( 'NONE',  ( 0.000000000000000000, 0.000000000000000000, 1.000000000000000000 ) ) ;
#16539 = ORIENTED_EDGE ( 'NONE', *, *, #24315, .F. ) ;
#16540 = CYLINDRICAL_SURFACE ( 'NONE', #25387, 16.00000000000000000 ) ;
#16541 = AXIS2_PLACEMENT_3D ( 'NONE', #42862, #3344, #16665 ) ;
#16542 = CARTESIAN_POINT ( 'NONE',  ( 0.000000000000000000, 0.6853352020790449695, 37.58145647212454321 ) ) ;
#16543 = CYLINDRICAL_SURFACE ( 'NONE', #40290, 31.99999999999998579 ) ;
#16544 = VERTEX_POINT ( 'NONE', #38554 ) ;
#16545 = ORIENTED_EDGE ( 'NONE', *, *, #44613, .F. ) ;
#16546 = AXIS2_PLACEMENT_3D ( 'NONE', #20677, #35613, #23617 ) ;
#16547 = SURFACE_STYLE_USAGE ( .BOTH. , #5052 ) ;
#16548 = AXIS2_PLACEMENT_3D ( 'NONE', #32706, #2145, #9711 ) ;
#16549 = CARTESIAN_POINT ( 'NONE',  ( 10.00000000000000000, 0.000000000000000000, 0.000000000000000000 ) ) ;
#16550 = DIRECTION ( 'NONE',  ( 1.000000000000000000, -0.000000000000000000, -0.000000000000000000 ) ) ;
#16551 = AXIS2_PLACEMENT_3D ( 'NONE', #19964, #38101, #5295 ) ;
#16552 = DIRECTION ( 'NONE',  ( 0.000000000000000000, 0.000000000000000000, 1.000000000000000000 ) ) ;
#16553 = CARTESIAN_POINT ( 'NONE',  ( -3.000000000000000000, -4.261787119645322974, 26.19803753235774835 ) ) ;
#16554 = DIRECTION ( 'NONE',  ( 0.000000000000000000, 0.000000000000000000, 1.000000000000000000 ) ) ;
#16555 = DIRECTION ( 'NONE',  ( -1.000000000000000000, -0.000000000000000000, -0.000000000000000000 ) ) ;
#16556 = ORIENTED_EDGE ( 'NONE', *, *, #42094, .T. ) ;
#16557 = CARTESIAN_POINT ( 'NONE',  ( 0.000000000000000000, -3.948201729842348850, 23.21447184625293048 ) ) ;
#16558 = ORIENTED_EDGE ( 'NONE', *, *, #10123, .F. ) ;
#16559 =( LENGTH_UNIT ( ) NAMED_UNIT ( * ) SI_UNIT ( .MILLI., .METRE. ) );
#16560 = CARTESIAN_POINT ( 'NONE',  ( 11.99999999999999822, -62.50884508063395373, -41.76106447765554464 ) ) ;
#16561 = ORIENTED_EDGE ( 'NONE', *, *, #42374, .F. ) ;
#16562 = ADVANCED_FACE ( 'NONE', ( #27535 ), #46137, .T. ) ;
#16563 = ORIENTED_EDGE ( 'NONE', *, *, #11221, .F. ) ;
#16564 = DIRECTION ( 'NONE',  ( -1.000000000000000000, -0.000000000000000000, -0.000000000000000000 ) ) ;
#16565 = VERTEX_POINT ( 'NONE', #27299 ) ;
#16566 = CIRCLE ( 'NONE', #36127, 16.00000000000000000 ) ;
#16567 = EDGE_CURVE ( 'NONE', #44578, #38804, #45176, .T. ) ;
#16568 = DIRECTION ( 'NONE',  ( 0.000000000000000000, 0.000000000000000000, -1.000000000000000000 ) ) ;
#16569 = AXIS2_PLACEMENT_3D ( 'NONE', #2034, #9584, #6177 ) ;
#16570 = DIRECTION ( 'NONE',  ( 0.000000000000000000, -0.5877852522924802425, 0.8090169943749422332 ) ) ;
#16571 = VERTEX_POINT ( 'NONE', #8925 ) ;
#16572 = ORIENTED_EDGE ( 'NONE', *, *, #28014, .F. ) ;
#16573 = EDGE_CURVE ( 'NONE', #14427, #1582, #12142, .T. ) ;
#16574 = ORIENTED_EDGE ( 'NONE', *, *, #33376, .F. ) ;
#16575 = VECTOR ( 'NONE', #6256, 1000.000000000000000 ) ;
#16576 = DIRECTION ( 'NONE',  ( -1.000000000000000000, 0.000000000000000000, 0.000000000000000000 ) ) ;
#16577 = DIRECTION ( 'NONE',  ( -1.000000000000000000, 0.000000000000000000, 0.000000000000000000 ) ) ;
#16578 = CARTESIAN_POINT ( 'NONE',  ( 10.00000000000000000, 70.52718814184260054, 26.02418014898334420 ) ) ;
#16579 = VERTEX_POINT ( 'NONE', #15793 ) ;
#16580 = CYLINDRICAL_SURFACE ( 'NONE', #6763, 82.00000000000000000 ) ;
#16581 = ORIENTED_EDGE ( 'NONE', *, *, #27928, .T. ) ;
#16582 = ORIENTED_EDGE ( 'NONE', *, *, #25823, .F. ) ;
#16583 = EDGE_CURVE ( 'NONE', #5172, #20943, #27062, .T. ) ;
#16584 = DIRECTION ( 'NONE',  ( 0.9038112904824842087, -0.4279312458753000703, 0.000000000000000000 ) ) ;
#16585 = DIRECTION ( 'NONE',  ( -1.000000000000000000, 0.000000000000000000, -0.000000000000000000 ) ) ;
#16586 = VECTOR ( 'NONE', #19507, 1000.000000000000000 ) ;
#16587 = ORIENTED_EDGE ( 'NONE', *, *, #35081, .F. ) ;
#16588 = EDGE_CURVE ( 'NONE', #18777, #44892, #37086, .T. ) ;
#16589 = CARTESIAN_POINT ( 'NONE',  ( 10.00000000000000000, -66.50666863322028632, 39.78640506895582973 ) ) ;
#16590 = CARTESIAN_POINT ( 'NONE',  ( 5.000000000000002665, -29.01471420065507090, -76.69515212746047439 ) ) ;
#16591 = CARTESIAN_POINT ( 'NONE',  ( 11.99999999999999822, -74.74816331893404708, -33.71516098798819172 ) ) ;
#16592 = ORIENTED_EDGE ( 'NONE', *, *, #4538, .T. ) ;
#16593 = EDGE_LOOP ( 'NONE', ( #31231, #16472, #20682, #31901 ) ) ;
#16594 = DIRECTION ( 'NONE',  ( 0.000000000000000000, 0.000000000000000000, 1.000000000000000000 ) ) ;
#16595 = DIRECTION ( 'NONE',  ( 0.000000000000000000, 0.000000000000000000, 1.000000000000000000 ) ) ;
#16596 = ORIENTED_EDGE ( 'NONE', *, *, #43552, .T. ) ;
#16597 = DIRECTION ( 'NONE',  ( -1.000000000000000000, -0.000000000000000000, 0.000000000000000000 ) ) ;
#16598 = ORIENTED_EDGE ( 'NONE', *, *, #27712, .T. ) ;
#16599 = AXIS2_PLACEMENT_3D ( 'NONE', #27381, #19519, #11493 ) ;
#16601 = EDGE_CURVE ( 'NONE', #42647, #15803, #42215, .T. ) ;
#16600 = CARTESIAN_POINT ( 'NONE',  ( 10.00000000000000000, 0.000000000000000000, 0.000000000000000000 ) ) ;
#16602 = CARTESIAN_POINT ( 'NONE',  ( 11.99999999999999822, -40.65526001592663619, 71.21200624218782593 ) ) ;
#16603 = CARTESIAN_POINT ( 'NONE',  ( 10.00000000000000000, 15.48615015657582283, 39.04073710021349797 ) ) ;
#16604 = CARTESIAN_POINT ( 'NONE',  ( 6.000000000000000000, 39.47590169984846398, 71.87247863392427405 ) ) ;
#16605 = DIRECTION ( 'NONE',  ( -1.000000000000000000, 0.000000000000000000, -0.000000000000000000 ) ) ;
#16607 = VECTOR ( 'NONE', #14261, 999.9999999999998863 ) ;
#16606 = CARTESIAN_POINT ( 'NONE',  ( -12.00000000000000000, 0.000000000000000000, -17.30399999999999849 ) ) ;
#16608 = VECTOR ( 'NONE', #3956, 1000.000000000000000 ) ;
#16609 = CARTESIAN_POINT ( 'NONE',  ( 0.000000000000000000, -74.74816331893453025, 33.71516098798714722 ) ) ;
#16610 = CARTESIAN_POINT ( 'NONE',  ( 10.00000000000000000, 37.22597642581158084, -5.202137450156524068 ) ) ;
#16611 = CARTESIAN_POINT ( 'NONE',  ( 0.000000000000000000, 2.663952781846149254, 41.91543099594818500 ) ) ;
#16612 = ORIENTED_EDGE ( 'NONE', *, *, #28874, .T. ) ;
#16613 = VECTOR ( 'NONE', #18072, 1000.000000000000000 ) ;
#16614 = FACE_OUTER_BOUND ( 'NONE', #26415, .T. ) ;
#16615 = SURFACE_STYLE_USAGE ( .BOTH. , #20042 ) ;
#16616 = VECTOR ( 'NONE', #16966, 1000.000000000000000 ) ;
#16617 = ORIENTED_EDGE ( 'NONE', *, *, #21492, .T. ) ;
#16618 = ORIENTED_EDGE ( 'NONE', *, *, #4103, .T. ) ;
#16619 = ADVANCED_FACE ( 'NONE', ( #15327 ), #16282, .F. ) ;
#16620 = AXIS2_PLACEMENT_3D ( 'NONE', #8465, #8950, #8227 ) ;
#16621 = CIRCLE ( 'NONE', #2521, 31.99999999999999289 ) ;
#16622 = ADVANCED_FACE ( 'NONE', ( #33898 ), #15549, .T. ) ;
#16623 = DIRECTION ( 'NONE',  ( -1.000000000000000000, 0.000000000000000000, -0.000000000000000000 ) ) ;
#16624 = PLANE ( 'NONE',  #1096 ) ;
#16625 = EDGE_CURVE ( 'NONE', #18915, #30366, #26807, .T. ) ;
#16626 = ORIENTED_EDGE ( 'NONE', *, *, #19580, .T. ) ;
#16627 = ORIENTED_EDGE ( 'NONE', *, *, #4831, .F. ) ;
#16628 = CARTESIAN_POINT ( 'NONE',  ( 0.000000000000000000, 5.835314593368477354, 22.81335362449854642 ) ) ;
#16629 = VECTOR ( 'NONE', #38947, 1000.000000000000000 ) ;
#16630 = ORIENTED_EDGE ( 'NONE', *, *, #46052, .F. ) ;
#16631 = EDGE_LOOP ( 'NONE', ( #4339, #13387, #23556, #39750 ) ) ;
#16632 = VERTEX_POINT ( 'NONE', #19444 ) ;
#16633 = VECTOR ( 'NONE', #41926, 1000.000000000000000 ) ;
#16634 = ADVANCED_FACE ( 'NONE', ( #23137 ), #11639, .T. ) ;
#16635 = EDGE_CURVE ( 'NONE', #18426, #20915, #45692, .T. ) ;
#16636 = EDGE_CURVE ( 'NONE', #39485, #34540, #22242, .T. ) ;
#16637 = AXIS2_PLACEMENT_3D ( 'NONE', #46060, #42140, #34536 ) ;
#16638 = FACE_OUTER_BOUND ( 'NONE', #1988, .T. ) ;
#16639 = EDGE_LOOP ( 'NONE', ( #20409, #9075, #36050, #9067 ) ) ;
#16640 = LINE ( 'NONE', #27922, #21572 ) ;
#16641 = VERTEX_POINT ( 'NONE', #22888 ) ;
#16642 = DIRECTION ( 'NONE',  ( -1.000000000000000000, 0.000000000000000000, 0.000000000000000000 ) ) ;
#16643 = AXIS2_PLACEMENT_3D ( 'NONE', #17836, #47686, #14176 ) ;
#16644 = CIRCLE ( 'NONE', #18964, 82.00000000000000000 ) ;
#16645 = FACE_OUTER_BOUND ( 'NONE', #21511, .T. ) ;
#16646 = DIRECTION ( 'NONE',  ( -1.000000000000000000, -0.000000000000000000, -0.000000000000000000 ) ) ;
#16647 = CIRCLE ( 'NONE', #45571, 31.99999999999999289 ) ;
#16648 = ORIENTED_EDGE ( 'NONE', *, *, #33692, .F. ) ;
#16649 = CARTESIAN_POINT ( 'NONE',  ( 10.00000000000000000, 0.000000000000000000, 0.000000000000000000 ) ) ;
#16650 = ORIENTED_EDGE ( 'NONE', *, *, #48178, .T. ) ;
#16651 = CYLINDRICAL_SURFACE ( 'NONE', #28951, 30.50000000000000000 ) ;
#16652 = DIRECTION ( 'NONE',  ( -1.000000000000000000, 0.000000000000000000, 0.000000000000000000 ) ) ;
#16653 = CIRCLE ( 'NONE', #9620, 16.00000000000000000 ) ;
#16654 = DIRECTION ( 'NONE',  ( 1.000000000000000000, 0.000000000000000000, 0.000000000000000000 ) ) ;
#16655 = EDGE_LOOP ( 'NONE', ( #11935, #43035, #5643, #42228 ) ) ;
#16656 = ORIENTED_EDGE ( 'NONE', *, *, #15897, .T. ) ;
#16657 = CARTESIAN_POINT ( 'NONE',  ( 10.00000000000000000, -31.52238457039580055, -27.75498641678775869 ) ) ;
#16658 = FACE_OUTER_BOUND ( 'NONE', #23319, .T. ) ;
#16659 = ORIENTED_EDGE ( 'NONE', *, *, #23193, .F. ) ;
#16660 = VECTOR ( 'NONE', #15781, 1000.000000000000000 ) ;
#16661 = FACE_OUTER_BOUND ( 'NONE', #15614, .T. ) ;
#16662 = CARTESIAN_POINT ( 'NONE',  ( 10.00000000000000000, -49.70050353004933896, 59.46389618801946852 ) ) ;
#16663 = CARTESIAN_POINT ( 'NONE',  ( 11.99999999999999822, -77.49459641780886443, 0.8261519478428549501 ) ) ;
#16664 = FACE_OUTER_BOUND ( 'NONE', #45405, .T. ) ;
#16665 = DIRECTION ( 'NONE',  ( 0.000000000000000000, 0.8090169943749445647, 0.5877852522924770229 ) ) ;
#16666 = DIRECTION ( 'NONE',  ( 0.000000000000000000, 0.000000000000000000, -1.000000000000000000 ) ) ;
#16667 = VERTEX_POINT ( 'NONE', #620 ) ;
#16668 = DIRECTION ( 'NONE',  ( 0.000000000000000000, 0.000000000000000000, -1.000000000000000000 ) ) ;
#16669 = CARTESIAN_POINT ( 'NONE',  ( -14.25258209288423750, -138.6845900058201551, 2.500000000000000000 ) ) ;
#16670 = CARTESIAN_POINT ( 'NONE',  ( 10.00000000000000000, 22.90783923731629912, 78.73519480814962890 ) ) ;
#16671 = DIRECTION ( 'NONE',  ( 0.000000000000000000, -0.7431448254773953543, -0.6691306063588570163 ) ) ;
#16672 = DIRECTION ( 'NONE',  ( 0.000000000000000000, -0.8660254037844363761, 0.5000000000000039968 ) ) ;
#16674 = AXIS2_PLACEMENT_3D ( 'NONE', #36709, #13254, #43114 ) ;
#16673 = DIRECTION ( 'NONE',  ( -1.000000000000000000, 0.000000000000000000, 0.000000000000000000 ) ) ;
#16675 = CARTESIAN_POINT ( 'NONE',  ( 0.000000000000000000, -37.48860685352291711, 0.8828120875899322373 ) ) ;
#16676 = ORIENTED_EDGE ( 'NONE', *, *, #16498, .T. ) ;
#16677 = EDGE_CURVE ( 'NONE', #19426, #3571, #45400, .T. ) ;
#16678 = CIRCLE ( 'NONE', #15904, 0.9999999999999991118 ) ;
#16679 = EDGE_LOOP ( 'NONE', ( #14615, #46737, #29326, #26819 ) ) ;
#16680 = EDGE_CURVE ( 'NONE', #14823, #32747, #37934, .T. ) ;
#16681 = LINE ( 'NONE', #8843, #26850 ) ;
#16682 = CYLINDRICAL_SURFACE ( 'NONE', #19758, 16.00000000000000000 ) ;
#16683 = AXIS2_PLACEMENT_3D ( 'NONE', #17299, #9723, #17547 ) ;
#16684 = CIRCLE ( 'NONE', #22202, 42.00000000000000000 ) ;
#16685 = AXIS2_PLACEMENT_3D ( 'NONE', #7763, #10728, #18768 ) ;
#16686 = EDGE_CURVE ( 'NONE', #24474, #6004, #35592, .T. ) ;
#16687 = CIRCLE ( 'NONE', #29184, 31.99999999999999289 ) ;
#16688 = CARTESIAN_POINT ( 'NONE',  ( 0.000000000000000000, 0.000000000000000000, 0.000000000000000000 ) ) ;
#16689 = EDGE_CURVE ( 'NONE', #12049, #42351, #19155, .T. ) ;
#16690 = AXIS2_PLACEMENT_3D ( 'NONE', #34905, #45686, #46171 ) ;
#16691 = ORIENTED_EDGE ( 'NONE', *, *, #16713, .T. ) ;
#16692 = CIRCLE ( 'NONE', #9651, 32.00000000000000000 ) ;
#16693 = AXIS2_PLACEMENT_3D ( 'NONE', #41717, #4517, #41478 ) ;
#16694 = DIRECTION ( 'NONE',  ( -1.000000000000000000, 0.000000000000000000, 0.000000000000000000 ) ) ;
#16695 = AXIS2_PLACEMENT_3D ( 'NONE', #45570, #19614, #34797 ) ;
#16696 = CARTESIAN_POINT ( 'NONE',  ( 10.00000000000000000, 0.000000000000000000, 0.000000000000000000 ) ) ;
#16697 = EDGE_LOOP ( 'NONE', ( #24331, #33776, #1015, #26023 ) ) ;
#16698 = CARTESIAN_POINT ( 'NONE',  ( 11.99999999999999822, 71.27951684758069462, -30.41916302227037150 ) ) ;
#16699 = EDGE_CURVE ( 'NONE', #35244, #20241, #42713, .T. ) ;
#16700 = EDGE_CURVE ( 'NONE', #41993, #46585, #2302, .T. ) ;
#16701 = CYLINDRICAL_SURFACE ( 'NONE', #12071, 20.99999999999999645 ) ;
#16702 = DIRECTION ( 'NONE',  ( -1.000000000000000000, 0.000000000000000000, 0.000000000000000000 ) ) ;
#16703 = ORIENTED_EDGE ( 'NONE', *, *, #40951, .T. ) ;
#16705 = ORIENTED_EDGE ( 'NONE', *, *, #14762, .T. ) ;
#16704 = LINE ( 'NONE', #16456, #1211 ) ;
#16706 = ORIENTED_EDGE ( 'NONE', *, *, #26210, .T. ) ;
#16707 = PRODUCT_DEFINITION ( 'UNKNOWN', '', #37413, #20840 ) ;
#16708 = CARTESIAN_POINT ( 'NONE',  ( 0.000000000000000000, 11.30684508768450591, -76.66974797899824523 ) ) ;
#16709 = CARTESIAN_POINT ( 'NONE',  ( 11.99999999999999822, 71.91182617369230456, -28.89263327155667938 ) ) ;
#16710 = CARTESIAN_POINT ( 'NONE',  ( 0.000000000000000000, 0.000000000000000000, 0.000000000000000000 ) ) ;
#16711 = DIRECTION ( 'NONE',  ( 0.000000000000000000, 0.9510565162951543083, 0.3090169943749449533 ) ) ;
#16712 = CIRCLE ( 'NONE', #39389, 15.99999999999999822 ) ;
#16713 = EDGE_CURVE ( 'NONE', #18460, #35877, #28742, .T. ) ;
#16714 = DIRECTION ( 'NONE',  ( 0.000000000000000000, -0.9876883405951394357, 0.1564344650402205716 ) ) ;
#16715 = ORIENTED_EDGE ( 'NONE', *, *, #23252, .T. ) ;
#16716 = CYLINDRICAL_SURFACE ( 'NONE', #6868, 37.49900000000000233 ) ;
#16717 = VERTEX_POINT ( 'NONE', #47096 ) ;
#16718 = VECTOR ( 'NONE', #6484, 1000.000000000000000 ) ;
#16719 = DIRECTION ( 'NONE',  ( -1.000000000000000000, -0.000000000000000000, -0.000000000000000000 ) ) ;
#16720 = CIRCLE ( 'NONE', #44840, 15.77977592589476608 ) ;
#16721 = ORIENTED_EDGE ( 'NONE', *, *, #30605, .T. ) ;
#16722 = AXIS2_PLACEMENT_3D ( 'NONE', #33945, #9815, #40576 ) ;
#16723 = DIRECTION ( 'NONE',  ( 0.000000000000000000, 0.000000000000000000, -1.000000000000000000 ) ) ;
#16724 = CYLINDRICAL_SURFACE ( 'NONE', #32109, 42.00000000000000000 ) ;
#16725 = DIRECTION ( 'NONE',  ( 0.000000000000000000, 0.000000000000000000, -1.000000000000000000 ) ) ;
#16726 = ORIENTED_EDGE ( 'NONE', *, *, #4823, .F. ) ;
#16727 = DIRECTION ( 'NONE',  ( 1.000000000000000000, -0.000000000000000000, 0.000000000000000000 ) ) ;
#16728 = DIRECTION ( 'NONE',  ( -1.000000000000000000, 0.000000000000000000, 0.000000000000000000 ) ) ;
#16729 = DIRECTION ( 'NONE',  ( -1.000000000000000000, -0.000000000000000000, 0.000000000000000000 ) ) ;
#16730 = CARTESIAN_POINT ( 'NONE',  ( 6.000000000000000000, 81.50828551894240093, -8.966570791699810528 ) ) ;
#16731 = CARTESIAN_POINT ( 'NONE',  ( 10.00000000000000000, -33.17418723428319538, 17.67226234102814431 ) ) ;
#16732 = ORIENTED_EDGE ( 'NONE', *, *, #35252, .T. ) ;
#16733 = CIRCLE ( 'NONE', #42515, 31.99999999999998934 ) ;
#16734 = AXIS2_PLACEMENT_3D ( 'NONE', #25260, #26254, #22076 ) ;
#16735 = LINE ( 'NONE', #2274, #5892 ) ;
#16736 = FILL_AREA_STYLE_COLOUR ( '', #4836 ) ;
#16737 = DIRECTION ( 'NONE',  ( 0.000000000000000000, 0.4539904997395478037, -0.8910065241883673437 ) ) ;
#16738 = AXIS2_PLACEMENT_3D ( 'NONE', #2385, #47428, #32262 ) ;
#16739 = AXIS2_PLACEMENT_3D ( 'NONE', #24508, #39452, #5927 ) ;
#16740 = DIRECTION ( 'NONE',  ( 0.000000000000000000, -0.1564344650402170744, -0.9876883405951399908 ) ) ;
#16741 = DIRECTION ( 'NONE',  ( -1.000000000000000000, 0.000000000000000000, 0.000000000000000000 ) ) ;
#16742 = AXIS2_PLACEMENT_3D ( 'NONE', #19156, #23314, #19389 ) ;
#16743 = VERTEX_POINT ( 'NONE', #13820 ) ;
#16744 = CARTESIAN_POINT ( 'NONE',  ( 11.99999999999999822, -17.28742895386137945, 75.54627589209938776 ) ) ;
#16745 = ORIENTED_EDGE ( 'NONE', *, *, #21987, .F. ) ;
#16746 = CYLINDRICAL_SURFACE ( 'NONE', #31614, 16.00000000000000000 ) ;
#16747 = EDGE_CURVE ( 'NONE', #19851, #37098, #44183, .T. ) ;
#16748 = DIRECTION ( 'NONE',  ( -1.000000000000000000, -0.000000000000000000, -0.000000000000000000 ) ) ;
#16749 = ADVANCED_FACE ( 'NONE', ( #5744, #46862, #21136 ), #13091, .T. ) ;
#16750 = VERTEX_POINT ( 'NONE', #32180 ) ;
#16751 = EDGE_CURVE ( 'NONE', #13135, #8929, #13566, .T. ) ;
#16752 = VECTOR ( 'NONE', #22401, 1000.000000000000000 ) ;
#16753 = DIRECTION ( 'NONE',  ( -1.000000000000000000, -0.000000000000000000, -0.000000000000000000 ) ) ;
#16754 = ORIENTED_EDGE ( 'NONE', *, *, #37639, .T. ) ;
#16755 = AXIS2_PLACEMENT_3D ( 'NONE', #22368, #41685, #4489 ) ;
#16756 = VERTEX_POINT ( 'NONE', #35837 ) ;
#16757 = ORIENTED_EDGE ( 'NONE', *, *, #13704, .T. ) ;
#16758 = EDGE_CURVE ( 'NONE', #26166, #20595, #12924, .T. ) ;
#16759 = VECTOR ( 'NONE', #5605, 1000.000000000000114 ) ;
#16760 = AXIS2_PLACEMENT_3D ( 'NONE', #45321, #4930, #26492 ) ;
#16761 = CARTESIAN_POINT ( 'NONE',  ( 0.000000000000000000, -17.67226234102801286, -33.17418723428327354 ) ) ;
#16762 = EDGE_CURVE ( 'NONE', #42524, #19183, #407, .T. ) ;
#16763 = VECTOR ( 'NONE', #7523, 1000.000000000000000 ) ;
#16764 = DIRECTION ( 'NONE',  ( -1.000000000000000000, 0.000000000000000000, -0.000000000000000000 ) ) ;
#16765 = CARTESIAN_POINT ( 'NONE',  ( 11.99999999999999822, 0.000000000000000000, 0.000000000000000000 ) ) ;
#16766 = ORIENTED_EDGE ( 'NONE', *, *, #46032, .T. ) ;
#16767 = CYLINDRICAL_SURFACE ( 'NONE', #28963, 16.00000000000000000 ) ;
#16768 = ORIENTED_EDGE ( 'NONE', *, *, #35202, .T. ) ;
#16769 = ORIENTED_EDGE ( 'NONE', *, *, #15529, .F. ) ;
#16770 = AXIS2_PLACEMENT_3D ( 'NONE', #48141, #37605, #45198 ) ;
#16771 = LINE ( 'NONE', #13336, #3014 ) ;
#16772 = FACE_OUTER_BOUND ( 'NONE', #46505, .T. ) ;
#16773 = CYLINDRICAL_SURFACE ( 'NONE', #18054, 77.49899999999999523 ) ;
#16774 = EDGE_CURVE ( 'NONE', #23667, #12709, #30112, .T. ) ;
#16775 = ORIENTED_EDGE ( 'NONE', *, *, #28398, .T. ) ;
#16776 = ORIENTED_EDGE ( 'NONE', *, *, #38753, .F. ) ;
#16777 = ORIENTED_EDGE ( 'NONE', *, *, #395, .T. ) ;
#16778 = DIRECTION ( 'NONE',  ( -1.000000000000000000, 0.000000000000000000, 0.000000000000000000 ) ) ;
#16779 = ORIENTED_EDGE ( 'NONE', *, *, #1708, .T. ) ;
#16780 = LINE ( 'NONE', #40266, #33249 ) ;
#16781 = CARTESIAN_POINT ( 'NONE',  ( -3.000000000000000000, -14.54903810567676636, 22.19967320028755964 ) ) ;
#16782 = CARTESIAN_POINT ( 'NONE',  ( 11.99999999999999822, -15.33399622253540606, 80.55351364060582853 ) ) ;
#16783 = CARTESIAN_POINT ( 'NONE',  ( 10.00000000000000000, -10.74501242461258244, -35.92658777277521409 ) ) ;
#16784 = CARTESIAN_POINT ( 'NONE',  ( 12.00000000000000000, 24.81905959214260804, -9.408202855044828894 ) ) ;
#16785 = CARTESIAN_POINT ( 'NONE',  ( 11.99999999999999822, -26.02418014898260878, -70.52718814184285634 ) ) ;
#16786 = DIRECTION ( 'NONE',  ( 0.000000000000000000, 0.000000000000000000, 1.000000000000000000 ) ) ;
#16787 = ORIENTED_EDGE ( 'NONE', *, *, #6096, .F. ) ;
#16788 = FACE_OUTER_BOUND ( 'NONE', #18500, .T. ) ;
#16789 = LINE ( 'NONE', #5293, #39453 ) ;
#16790 = EDGE_CURVE ( 'NONE', #22095, #36859, #34005, .T. ) ;
#16791 = CARTESIAN_POINT ( 'NONE',  ( 10.00000000000000000, -22.90783923731686045, 78.73519480814947258 ) ) ;
#16792 = VECTOR ( 'NONE', #10764, 1000.000000000000000 ) ;
#16793 = DIRECTION ( 'NONE',  ( -1.000000000000000000, -0.000000000000000000, 0.000000000000000000 ) ) ;
#16794 = VERTEX_POINT ( 'NONE', #39770 ) ;
#16795 = CARTESIAN_POINT ( 'NONE',  ( 10.00000000000000000, 16.23288003029543347, -33.80338159004267595 ) ) ;
#16796 = VECTOR ( 'NONE', #29749, 1000.000000000000000 ) ;
#16797 = VECTOR ( 'NONE', #10351, 1000.000000000000114 ) ;
#16798 = CYLINDRICAL_SURFACE ( 'NONE', #18090, 31.99999999999998579 ) ;
#16799 = CARTESIAN_POINT ( 'NONE',  ( 10.00000000000000000, -21.40280677340345505, -36.13751322684441902 ) ) ;
#16800 = FACE_OUTER_BOUND ( 'NONE', #36316, .T. ) ;
#16801 = CARTESIAN_POINT ( 'NONE',  ( 11.99999999999999822, 0.000000000000000000, 0.000000000000000000 ) ) ;
#16802 = AXIS2_PLACEMENT_3D ( 'NONE', #8207, #5019, #34872 ) ;
#16803 = DIRECTION ( 'NONE',  ( -1.000000000000000000, 0.000000000000000000, 0.000000000000000000 ) ) ;
#16804 = CARTESIAN_POINT ( 'NONE',  ( 0.000000000000000000, -0.8299999999999999600, 0.000000000000000000 ) ) ;
#16805 = ORIENTED_EDGE ( 'NONE', *, *, #10306, .T. ) ;
#16806 = AXIS2_PLACEMENT_3D ( 'NONE', #34400, #12175, #4343 ) ;
#16807 = EDGE_CURVE ( 'NONE', #18388, #10792, #5498, .T. ) ;
#16808 = DIRECTION ( 'NONE',  ( -0.9781476007338069101, 0.2079116908177532363, 0.000000000000000000 ) ) ;
#16809 = EDGE_CURVE ( 'NONE', #42385, #17337, #29333, .T. ) ;
#16810 = VECTOR ( 'NONE', #14244, 1000.000000000000000 ) ;
#16811 = VERTEX_POINT ( 'NONE', #5270 ) ;
#16812 = CARTESIAN_POINT ( 'NONE',  ( -12.49999999999999645, 0.000000000000000000, 125.0000000000000000 ) ) ;
#16813 = EDGE_CURVE ( 'NONE', #37423, #13942, #25403, .T. ) ;
#16814 = ORIENTED_EDGE ( 'NONE', *, *, #9387, .F. ) ;
#16815 = VERTEX_POINT ( 'NONE', #35605 ) ;
#16816 = ADVANCED_FACE ( 'NONE', ( #1834 ), #31715, .F. ) ;
#16817 = EDGE_CURVE ( 'NONE', #32670, #40177, #16992, .T. ) ;
#16818 = LINE ( 'NONE', #27588, #710 ) ;
#16819 = ORIENTED_EDGE ( 'NONE', *, *, #42067, .T. ) ;
#16820 = ORIENTED_EDGE ( 'NONE', *, *, #34810, .F. ) ;
#16821 = VECTOR ( 'NONE', #26303, 1000.000000000000000 ) ;
#16822 = DIRECTION ( 'NONE',  ( 0.000000000000000000, 0.000000000000000000, -1.000000000000000000 ) ) ;
#16823 = CYLINDRICAL_SURFACE ( 'NONE', #19884, 82.00000000000000000 ) ;
#16824 = ORIENTED_EDGE ( 'NONE', *, *, #45776, .T. ) ;
#16825 = ORIENTED_EDGE ( 'NONE', *, *, #39417, .F. ) ;
#16826 = CARTESIAN_POINT ( 'NONE',  ( 0.000000000000000000, 0.000000000000000000, 0.000000000000000000 ) ) ;
#16828 = EDGE_LOOP ( 'NONE', ( #8324, #40526, #27400, #44124 ) ) ;
#16827 = DIRECTION ( 'NONE',  ( 1.000000000000000000, 0.000000000000000000, 0.000000000000000000 ) ) ;
#16829 = EDGE_CURVE ( 'NONE', #40361, #35892, #23850, .T. ) ;
#16830 = CARTESIAN_POINT ( 'NONE',  ( 10.00000000000000000, -25.88420570971419821, 27.13269053701087330 ) ) ;
#16831 = AXIS2_PLACEMENT_3D ( 'NONE', #16042, #45903, #12372 ) ;
#16832 = VECTOR ( 'NONE', #40488, 1000.000000000000000 ) ;
#16833 = ORIENTED_EDGE ( 'NONE', *, *, #15638, .F. ) ;
#16834 = ORIENTED_EDGE ( 'NONE', *, *, #14657, .T. ) ;
#16835 = LINE ( 'NONE', #32015, #4406 ) ;
#16836 = ORIENTED_EDGE ( 'NONE', *, *, #21916, .T. ) ;
#16837 = VERTEX_POINT ( 'NONE', #6002 ) ;
#16838 = CARTESIAN_POINT ( 'NONE',  ( 4.999999999999999112, -40.68715046381921496, -10.41901085202121280 ) ) ;
#16839 = DIRECTION ( 'NONE',  ( 0.000000000000000000, 0.1045284632676436315, 0.9945218953682742891 ) ) ;
#16840 = AXIS2_PLACEMENT_3D ( 'NONE', #46166, #38836, #24132 ) ;
#16841 = DIRECTION ( 'NONE',  ( 0.000000000000000000, 0.000000000000000000, 1.000000000000000000 ) ) ;
#16842 = DIRECTION ( 'NONE',  ( 0.000000000000000000, 0.000000000000000000, 1.000000000000000000 ) ) ;
#16843 = CARTESIAN_POINT ( 'NONE',  ( 11.99999999999999822, 0.000000000000000000, 0.000000000000000000 ) ) ;
#16844 = EDGE_CURVE ( 'NONE', #26882, #929, #31702, .T. ) ;
#16846 = ORIENTED_EDGE ( 'NONE', *, *, #27919, .T. ) ;
#16845 = AXIS2_PLACEMENT_3D ( 'NONE', #6723, #9912, #32192 ) ;
#16847 = AXIS2_PLACEMENT_3D ( 'NONE', #42842, #9526, #24226 ) ;
#16848 = ORIENTED_EDGE ( 'NONE', *, *, #36407, .T. ) ;
#16849 = CARTESIAN_POINT ( 'NONE',  ( 10.00000000000000000, 14.66109333815564852, -73.73191006444555740 ) ) ;
#16850 = EDGE_CURVE ( 'NONE', #32306, #19020, #48051, .T. ) ;
#16851 = CARTESIAN_POINT ( 'NONE',  ( 0.000000000000000000, -73.44644590900077219, 24.73286445877677764 ) ) ;
#16852 = ORIENTED_EDGE ( 'NONE', *, *, #36974, .F. ) ;
#16853 = CARTESIAN_POINT ( 'NONE',  ( 0.000000000000000000, 22.07842321921481243, 8.187992925817422218 ) ) ;
#16854 = EDGE_LOOP ( 'NONE', ( #27017, #31852, #34991, #20358, #36187, #17761 ) ) ;
#16855 = CARTESIAN_POINT ( 'NONE',  ( 10.00000000000000000, 16.00000000000000000, 2.500000000000000000 ) ) ;
#16856 = CARTESIAN_POINT ( 'NONE',  ( 10.00000000000000000, 26.01480285779837232, 70.53064760720326376 ) ) ;
#16857 = FACE_OUTER_BOUND ( 'NONE', #3626, .T. ) ;
#16858 = CIRCLE ( 'NONE', #2012, 14.09999999999999964 ) ;
#16859 = CYLINDRICAL_SURFACE ( 'NONE', #214, 16.00000000000000000 ) ;
#16860 = LINE ( 'NONE', #23964, #6189 ) ;
#16861 = CYLINDRICAL_SURFACE ( 'NONE', #22422, 42.00000000000000000 ) ;
#16862 = AXIS2_PLACEMENT_3D ( 'NONE', #38278, #45878, #8896 ) ;
#16863 = ORIENTED_EDGE ( 'NONE', *, *, #1287, .F. ) ;
#16864 = CARTESIAN_POINT ( 'NONE',  ( 4.250000000000000000, -13.95926121303099343, -1.199999999999999956 ) ) ;
#16865 = LINE ( 'NONE', #13906, #16759 ) ;
#16866 = CARTESIAN_POINT ( 'NONE',  ( 0.000000000000000000, 0.000000000000000000, -1.199999999999999956 ) ) ;
#16867 = ADVANCED_FACE ( 'NONE', ( #32876 ), #7433, .T. ) ;
#16868 = FACE_OUTER_BOUND ( 'NONE', #178, .T. ) ;
#16869 = EDGE_CURVE ( 'NONE', #36710, #15673, #37039, .T. ) ;
#16870 = EDGE_LOOP ( 'NONE', ( #36142, #8313, #6337, #38389 ) ) ;
#16871 = ORIENTED_EDGE ( 'NONE', *, *, #33546, .T. ) ;
#16872 = EDGE_CURVE ( 'NONE', #23277, #25392, #37285, .T. ) ;
#16873 = EDGE_CURVE ( 'NONE', #21372, #32749, #14488, .T. ) ;
#16874 = DIRECTION ( 'NONE',  ( 0.000000000000000000, 1.000000000000000000, 3.491481338843133355E-15 ) ) ;
#16875 = DIRECTION ( 'NONE',  ( -0.3311129884571281101, -0.9435911131814402886, 0.000000000000000000 ) ) ;
#16876 = AXIS2_PLACEMENT_3D ( 'NONE', #43395, #35311, #32138 ) ;
#16877 = ORIENTED_EDGE ( 'NONE', *, *, #40347, .F. ) ;
#16878 = CLOSED_SHELL ( 'NONE', ( #10423, #4928, #7023, #25276, #9632, #24969, #27645, #41572, #17514, #8285, #7721, #2710, #5214, #36224, #22918, #37860, #36838, #44751, #44433, #47601, #7487, #7336, #31517, #604, #39078, #10727, #31185, #32795, #39911, #8875, #11108, #30147, #28740, #13314, #47025, #3725, #46327, #10488, #34753, #41554, #29569, #29054, #29280, #3338, #11400, #31121, #26123, #24641, #29771, #32534, #10946, #6798, #28765, #9611, #616, #20498, #19173, #47791, #29452, #11143, #19875, #28842, #12840, #45517, #31899, #34249, #20693, #45834, #37176, #42335, #4391, #40120, #23808, #17941, #12723, #20011, #1579, #25402, #33148, #25618, #22561, #27155, #275, #30681, #1381, #18146, #31146, #15698, #48154, #20120, #47781, #28737, #33529, #17452, #40460, #2017, #37830, #3404, #12016, #26517, #37574, #11687, #20907, #3531, #11039, #44375, #31944, #4535, #26754, #45893, #40760, #6869, #46760, #15303, #14908, #27048, #553, #17723, #10931, #35039, #43664, #8312, #39643, #1104, #11465, #21938, #42024, #24541, #19222, #41168, #20346, #22283, #16, #36816, #27924, #35869, #10835, #36239, #5924, #45982, #35964, #36680, #13738, #713, #796, #26369, #10948, #28021, #24409, #2185, #30694, #10906, #7348, #29880, #43745, #13932, #15585, #36514, #36947, #27351, #42801, #17106, #16159, #38300, #48346, #39548, #8904, #33071, #19442, #43210, #14921, #21193, #42402 ) ) ;
#16879 = DIRECTION ( 'NONE',  ( 0.000000000000000000, 0.000000000000000000, 1.000000000000000000 ) ) ;
#16880 = ORIENTED_EDGE ( 'NONE', *, *, #18107, .T. ) ;
#16881 = VERTEX_POINT ( 'NONE', #3748 ) ;
#16882 = EDGE_LOOP ( 'NONE', ( #23267, #27410, #32123, #11532 ) ) ;
#16883 = AXIS2_PLACEMENT_3D ( 'NONE', #40745, #21416, #47600 ) ;
#16884 = CARTESIAN_POINT ( 'NONE',  ( 10.00000000000000000, 59.46389618801964616, 49.70050353004912580 ) ) ;
#16885 = ORIENTED_EDGE ( 'NONE', *, *, #32644, .F. ) ;
#16886 = FACE_OUTER_BOUND ( 'NONE', #22778, .T. ) ;
#16887 = ORIENTED_EDGE ( 'NONE', *, *, #13504, .F. ) ;
#16888 = CARTESIAN_POINT ( 'NONE',  ( 5.000000000000002665, -15.33399622253540961, 80.55351364060584274 ) ) ;
#16889 = DIRECTION ( 'NONE',  ( 0.000000000000000000, -0.9945218953682741780, 0.1045284632676447972 ) ) ;
#16890 = DIRECTION ( 'NONE',  ( -1.000000000000000000, 0.000000000000000000, 0.000000000000000000 ) ) ;
#16891 = CIRCLE ( 'NONE', #9066, 16.00000000000000000 ) ;
#16892 = ORIENTED_EDGE ( 'NONE', *, *, #41234, .T. ) ;
#16893 = DIRECTION ( 'NONE',  ( -1.000000000000000000, -0.000000000000000000, 0.000000000000000000 ) ) ;
#16894 = ORIENTED_EDGE ( 'NONE', *, *, #4744, .T. ) ;
#16895 = DIRECTION ( 'NONE',  ( 0.000000000000000000, 0.8526401643540897357, 0.5224985647159527957 ) ) ;
#16896 = LINE ( 'NONE', #20809, #21183 ) ;
#16897 = AXIS2_PLACEMENT_3D ( 'NONE', #35675, #2148, #17781 ) ;
#16898 = CARTESIAN_POINT ( 'NONE',  ( 7.468086116107294004, -12.33868914344945189, 0.000000000000000000 ) ) ;
#16899 = EDGE_LOOP ( 'NONE', ( #27921, #7087, #29702, #3125 ) ) ;
#16900 = ORIENTED_EDGE ( 'NONE', *, *, #44715, .F. ) ;
#16901 = CARTESIAN_POINT ( 'NONE',  ( 10.00000000000000000, 20.41045688087824317, 72.35160999960824313 ) ) ;
#16902 = DIRECTION ( 'NONE',  ( 0.000000000000000000, 0.8910065241883691201, -0.4539904997395446951 ) ) ;
#16903 = ORIENTED_EDGE ( 'NONE', *, *, #27385, .F. ) ;
#16904 = EDGE_CURVE ( 'NONE', #40015, #19091, #21859, .T. ) ;
#16905 = FACE_OUTER_BOUND ( 'NONE', #13206, .T. ) ;
#16906 = CIRCLE ( 'NONE', #37196, 35.50000000000000711 ) ;
#16907 = LINE ( 'NONE', #43092, #5549 ) ;
#16908 = FACE_OUTER_BOUND ( 'NONE', #18595, .T. ) ;
#16909 = DIRECTION ( 'NONE',  ( -1.000000000000000000, -0.000000000000000000, 0.000000000000000000 ) ) ;
#16910 = PLANE ( 'NONE',  #9108 ) ;
#16911 = CARTESIAN_POINT ( 'NONE',  ( -23.42219527698293646, -121.9106984081423803, 2.500000000000000000 ) ) ;
#16912 = CARTESIAN_POINT ( 'NONE',  ( -1.200000000000000030E-05, 16.95692799528845640, -2.500000000000000000 ) ) ;
#16913 = VECTOR ( 'NONE', #11074, 1000.000000000000000 ) ;
#16914 = CARTESIAN_POINT ( 'NONE',  ( 0.000000000000000000, 0.000000000000000000, 0.000000000000000000 ) ) ;
#16915 = DIRECTION ( 'NONE',  ( 0.000000000000000000, 0.000000000000000000, 1.000000000000000000 ) ) ;
#16916 = CARTESIAN_POINT ( 'NONE',  ( 6.000000000000000000, 71.87247863392471459, -39.47590169984771080 ) ) ;
#16917 = EDGE_CURVE ( 'NONE', #11391, #42540, #26191, .T. ) ;
#16918 = VECTOR ( 'NONE', #36979, 1000.000000000000000 ) ;
#16919 = PLANE ( 'NONE',  #3805 ) ;
#16920 = CARTESIAN_POINT ( 'NONE',  ( 10.00000000000000000, -36.88895765772637247, 6.736453364083436313 ) ) ;
#16921 = ADVANCED_FACE ( 'NONE', ( #48057 ), #26018, .T. ) ;
#16922 = ORIENTED_EDGE ( 'NONE', *, *, #5255, .F. ) ;
#16923 = EDGE_CURVE ( 'NONE', #17280, #32168, #44389, .T. ) ;
#16924 = ORIENTED_EDGE ( 'NONE', *, *, #16531, .T. ) ;
#16925 = VECTOR ( 'NONE', #941, 1000.000000000000114 ) ;
#16926 = DIRECTION ( 'NONE',  ( -1.000000000000000000, 0.000000000000000000, -0.000000000000000000 ) ) ;
#16927 = CARTESIAN_POINT ( 'NONE',  ( 0.000000000000000000, -120.0000000000000000, 2.500000000000000000 ) ) ;
#16928 = EDGE_CURVE ( 'NONE', #1474, #6091, #18674, .T. ) ;
#16929 = EDGE_CURVE ( 'NONE', #47410, #31423, #48295, .T. ) ;
#16930 = DIRECTION ( 'NONE',  ( 0.000000000000000000, 0.000000000000000000, 1.000000000000000000 ) ) ;
#16931 = ORIENTED_EDGE ( 'NONE', *, *, #41221, .F. ) ;
#16932 = ORIENTED_EDGE ( 'NONE', *, *, #2858, .F. ) ;
#16933 = AXIS2_PLACEMENT_3D ( 'NONE', #3824, #48365, #32709 ) ;
#16934 = CARTESIAN_POINT ( 'NONE',  ( 11.99999999999999822, -78.73519480814969995, 22.90783923731599359 ) ) ;
#16935 = FACE_OUTER_BOUND ( 'NONE', #4840, .T. ) ;
#16936 = AXIS2_PLACEMENT_3D ( 'NONE', #20568, #13952, #35508 ) ;
#16937 = ORIENTED_EDGE ( 'NONE', *, *, #42994, .T. ) ;
#16938 = CARTESIAN_POINT ( 'NONE',  ( 0.000000000000000000, 72.35432306680485226, -20.40083707022909110 ) ) ;
#16939 = AXIS2_PLACEMENT_3D ( 'NONE', #23455, #20031, #5355 ) ;
#16940 = LINE ( 'NONE', #31895, #32841 ) ;
#16941 = VERTEX_POINT ( 'NONE', #15018 ) ;
#16942 = CARTESIAN_POINT ( 'NONE',  ( 12.00000000000000000, 22.07842321921480533, -8.187992925817425771 ) ) ;
#16943 = ORIENTED_EDGE ( 'NONE', *, *, #35910, .T. ) ;
#16944 = DIRECTION ( 'NONE',  ( 1.000000000000000000, 0.000000000000000000, -0.000000000000000000 ) ) ;
#16945 = EDGE_LOOP ( 'NONE', ( #35652, #28531, #24276, #41690 ) ) ;
#16946 = FACE_OUTER_BOUND ( 'NONE', #5, .T. ) ;
#16947 = DIRECTION ( 'NONE',  ( -0.000000000000000000, -0.000000000000000000, 1.000000000000000000 ) ) ;
#16948 = ADVANCED_FACE ( 'NONE', ( #29935 ), #44872, .F. ) ;
#16950 = ORIENTED_EDGE ( 'NONE', *, *, #19488, .T. ) ;
#16949 = CARTESIAN_POINT ( 'NONE',  ( -3.000000000000000000, 18.84667830672579925, 18.68964196561269020 ) ) ;
#16951 = EDGE_CURVE ( 'NONE', #42453, #25698, #5092, .T. ) ;
#16952 = ORIENTED_EDGE ( 'NONE', *, *, #25908, .T. ) ;
#16953 = FACE_OUTER_BOUND ( 'NONE', #16899, .T. ) ;
#16954 = EDGE_LOOP ( 'NONE', ( #31269, #18842, #10686, #47162 ) ) ;
#16955 = DIRECTION ( 'NONE',  ( -0.000000000000000000, -0.000000000000000000, -1.000000000000000000 ) ) ;
#16956 = VERTEX_POINT ( 'NONE', #21383 ) ;
#16957 = EDGE_CURVE ( 'NONE', #36861, #36640, #36322, .T. ) ;
#16958 = CARTESIAN_POINT ( 'NONE',  ( 10.00000000000000000, -36.13751322684404244, -21.40280677340410165 ) ) ;
#16959 = CARTESIAN_POINT ( 'NONE',  ( -3.000000000000000000, 23.50000000000000000, -1.500000000000001332 ) ) ;
#16960 = DIRECTION ( 'NONE',  ( 1.000000000000000000, 0.000000000000000000, 0.000000000000000000 ) ) ;
#16961 = ORIENTED_EDGE ( 'NONE', *, *, #13271, .T. ) ;
#16962 = CARTESIAN_POINT ( 'NONE',  ( 15.00000000000000000, -4.261787119645322974, -26.19803753235774835 ) ) ;
#16963 = ADVANCED_FACE ( 'NONE', ( #32641 ), #3019, .T. ) ;
#16964 = FACE_OUTER_BOUND ( 'NONE', #10638, .T. ) ;
#16965 = CARTESIAN_POINT ( 'NONE',  ( 15.00000000000000000, -23.29833615347109088, -3.418703333116486665 ) ) ;
#16966 = DIRECTION ( 'NONE',  ( 1.000000000000000000, -0.000000000000000000, 0.000000000000000000 ) ) ;
#16967 = DIRECTION ( 'NONE',  ( 1.000000000000000000, 0.000000000000000000, 0.000000000000000000 ) ) ;
#16968 = VECTOR ( 'NONE', #15745, 1000.000000000000000 ) ;
#16969 = CARTESIAN_POINT ( 'NONE',  ( 0.000000000000000000, 26.50000000000000711, 1.500000000000000000 ) ) ;
#16970 = DIRECTION ( 'NONE',  ( 0.000000000000000000, 0.000000000000000000, 1.000000000000000000 ) ) ;
#16971 = LINE ( 'NONE', #9148, #31850 ) ;
#16972 = AXIS2_PLACEMENT_3D ( 'NONE', #18814, #18344, #26180 ) ;
#16973 = LINE ( 'NONE', #25029, #47103 ) ;
#16974 = LINE ( 'NONE', #31931, #40980 ) ;
#16975 = ADVANCED_FACE ( 'NONE', ( #40252 ), #21636, .T. ) ;
#16976 = EDGE_CURVE ( 'NONE', #9769, #28195, #25535, .T. ) ;
#16977 = DIRECTION ( 'NONE',  ( 1.000000000000000000, 0.000000000000000000, 0.000000000000000000 ) ) ;
#16978 = CIRCLE ( 'NONE', #25562, 31.99999999999999289 ) ;
#16979 = VERTEX_POINT ( 'NONE', #41681 ) ;
#16980 = DIRECTION ( 'NONE',  ( 0.8774505977381971134, 0.4796670183876317051, -0.000000000000000000 ) ) ;
#16981 = LINE ( 'NONE', #18167, #15850 ) ;
#16982 = ORIENTED_EDGE ( 'NONE', *, *, #30067, .T. ) ;
#16983 = EDGE_CURVE ( 'NONE', #26733, #30959, #19624, .T. ) ;
#16984 = CIRCLE ( 'NONE', #39647, 31.99999999999999289 ) ;
#16985 = DIRECTION ( 'NONE',  ( 0.000000000000000000, 0.000000000000000000, 1.000000000000000000 ) ) ;
#16986 = VERTEX_POINT ( 'NONE', #31161 ) ;
#16987 = ORIENTED_EDGE ( 'NONE', *, *, #32284, .T. ) ;
#16988 = ORIENTED_EDGE ( 'NONE', *, *, #38930, .F. ) ;
#16989 = AXIS2_PLACEMENT_3D ( 'NONE', #46584, #31174, #27984 ) ;
#16990 = DIRECTION ( 'NONE',  ( -0.7950889364178781449, 0.6064928550163533050, 0.000000000000000000 ) ) ;
#16991 = CARTESIAN_POINT ( 'NONE',  ( 0.000000000000000000, 59.03961581697465277, -46.53671651293886669 ) ) ;
#16993 = VERTEX_POINT ( 'NONE', #23079 ) ;
#16992 = LINE ( 'NONE', #31948, #13686 ) ;
#16994 = EDGE_LOOP ( 'NONE', ( #22606, #17002, #45762, #17637 ) ) ;
#16995 = CIRCLE ( 'NONE', #32622, 42.00000000000000000 ) ;
#16996 = DIRECTION ( 'NONE',  ( 0.000000000000000000, 0.000000000000000000, 1.000000000000000000 ) ) ;
#16997 = ORIENTED_EDGE ( 'NONE', *, *, #43345, .F. ) ;
#16998 = DIRECTION ( 'NONE',  ( 1.000000000000000000, -0.000000000000000000, 0.000000000000000000 ) ) ;
#16999 = CARTESIAN_POINT ( 'NONE',  ( 11.99999999999999822, 75.16055320797030959, 18.89407956138283851 ) ) ;
#17000 = LINE ( 'NONE', #27307, #46240 ) ;
#17001 = EDGE_CURVE ( 'NONE', #43248, #18614, #567, .T. ) ;
#17002 = ORIENTED_EDGE ( 'NONE', *, *, #28792, .T. ) ;
#17003 = VECTOR ( 'NONE', #15702, 1000.000000000000000 ) ;
#17004 = ORIENTED_EDGE ( 'NONE', *, *, #46085, .F. ) ;
#17005 = DIRECTION ( 'NONE',  ( 0.000000000000000000, 0.7604059656000322631, -0.6494480483301821039 ) ) ;
#17006 = EDGE_LOOP ( 'NONE', ( #23419, #31960, #37973, #1005 ) ) ;
#17007 = FACE_BOUND ( 'NONE', #30756, .T. ) ;
#17008 = EDGE_CURVE ( 'NONE', #28298, #34997, #21507, .T. ) ;
#17009 = CARTESIAN_POINT ( 'NONE',  ( 12.00000000000000000, 8.688484142253932063, -21.88630264137371384 ) ) ;
#17010 = FACE_OUTER_BOUND ( 'NONE', #38058, .T. ) ;
#17011 = DIRECTION ( 'NONE',  ( 0.000000000000000000, 0.000000000000000000, -1.000000000000000000 ) ) ;
#17012 = CARTESIAN_POINT ( 'NONE',  ( 10.00000000000000000, 35.92658777277525672, -10.74501242461245809 ) ) ;
#17013 = ADVANCED_FACE ( 'NONE', ( #19871 ), #38491, .T. ) ;
#17014 = DIRECTION ( 'NONE',  ( -1.000000000000000000, 0.000000000000000000, 0.000000000000000000 ) ) ;
#17015 = DIRECTION ( 'NONE',  ( -1.000000000000000000, 0.000000000000000000, 0.000000000000000000 ) ) ;
#17016 = DIRECTION ( 'NONE',  ( -1.000000000000000000, 0.000000000000000000, 0.000000000000000000 ) ) ;
#17017 = DIRECTION ( 'NONE',  ( -1.000000000000000000, 0.000000000000000000, 0.000000000000000000 ) ) ;
#17018 = CARTESIAN_POINT ( 'NONE',  ( 0.000000000000000000, 0.000000000000000000, 0.000000000000000000 ) ) ;
#17019 = VERTEX_POINT ( 'NONE', #34318 ) ;
#17020 = ORIENTED_EDGE ( 'NONE', *, *, #32797, .T. ) ;
#17021 = DIRECTION ( 'NONE',  ( -1.000000000000000000, 0.000000000000000000, 0.000000000000000000 ) ) ;
#17022 = DIRECTION ( 'NONE',  ( -1.000000000000000000, 0.000000000000000000, 0.000000000000000000 ) ) ;
#17023 = DIRECTION ( 'NONE',  ( 0.000000000000000000, 0.000000000000000000, 1.000000000000000000 ) ) ;
#17024 = EDGE_CURVE ( 'NONE', #10193, #32354, #47335, .T. ) ;
#17025 = EDGE_CURVE ( 'NONE', #9834, #45908, #11392, .T. ) ;
#17026 = DIRECTION ( 'NONE',  ( 0.9135454576426059736, -0.4067366430757887730, 0.000000000000000000 ) ) ;
#17027 = CARTESIAN_POINT ( 'NONE',  ( 15.00000000000000000, -3.948201729842355068, -23.21447184625292692 ) ) ;
#17028 = DIRECTION ( 'NONE',  ( 0.000000000000000000, -0.4539904997395542430, 0.8910065241883641241 ) ) ;
#17029 = CARTESIAN_POINT ( 'NONE',  ( -12.50000000000000000, -107.5000000000000000, 2.500000000000000000 ) ) ;
#17030 = EDGE_CURVE ( 'NONE', #46829, #15966, #46566, .T. ) ;
#17031 = VERTEX_POINT ( 'NONE', #11359 ) ;
#17032 = CARTESIAN_POINT ( 'NONE',  ( 0.000000000000000000, 0.000000000000000000, 125.0000000000000000 ) ) ;
#17033 = VECTOR ( 'NONE', #44604, 1000.000000000000000 ) ;
#17034 = ORIENTED_EDGE ( 'NONE', *, *, #43357, .F. ) ;
#17035 = SURFACE_SIDE_STYLE ('',( #34917 ) ) ;
#17036 = AXIS2_PLACEMENT_3D ( 'NONE', #25356, #40063, #13630 ) ;
#17037 = DIRECTION ( 'NONE',  ( 0.000000000000000000, -0.8090169943749497827, -0.5877852522924698064 ) ) ;
#17038 = VERTEX_POINT ( 'NONE', #34813 ) ;
#17039 = ORIENTED_EDGE ( 'NONE', *, *, #31071, .T. ) ;
#17040 = EDGE_CURVE ( 'NONE', #41560, #21364, #32481, .T. ) ;
#17041 = ORIENTED_EDGE ( 'NONE', *, *, #40122, .T. ) ;
#17042 = ORIENTED_EDGE ( 'NONE', *, *, #27768, .F. ) ;
#17043 = DIRECTION ( 'NONE',  ( 0.000000000000000000, 0.000000000000000000, -1.000000000000000000 ) ) ;
#17044 = PRODUCT_DEFINITION_FORMATION_WITH_SPECIFIED_SOURCE ( 'ANY', '', #10492, .NOT_KNOWN. ) ;
#17045 = EDGE_LOOP ( 'NONE', ( #23014, #14468, #25470, #43197 ) ) ;
#17046 = CIRCLE ( 'NONE', #21734, 82.00000000000000000 ) ;
#17047 = ORIENTED_EDGE ( 'NONE', *, *, #19045, .T. ) ;
#17048 = CYLINDRICAL_SURFACE ( 'NONE', #23417, 77.49899999999999523 ) ;
#17049 = FACE_OUTER_BOUND ( 'NONE', #21792, .T. ) ;
#17050 = ORIENTED_EDGE ( 'NONE', *, *, #13967, .T. ) ;
#17051 = ORIENTED_EDGE ( 'NONE', *, *, #1289, .F. ) ;
#17052 = ORIENTED_EDGE ( 'NONE', *, *, #18091, .T. ) ;
#17053 = CARTESIAN_POINT ( 'NONE',  ( 12.00000000000000000, -0.9646360437375368635, -23.52805723605589705 ) ) ;
#17055 = ORIENTED_EDGE ( 'NONE', *, *, #31414, .F. ) ;
#17054 = DIRECTION ( 'NONE',  ( -1.000000000000000000, 0.000000000000000000, -0.000000000000000000 ) ) ;
#17056 = DIRECTION ( 'NONE',  ( -1.000000000000000000, -0.000000000000000000, -0.000000000000000000 ) ) ;
#17057 = ORIENTED_EDGE ( 'NONE', *, *, #14549, .T. ) ;
#17058 = ORIENTED_EDGE ( 'NONE', *, *, #6599, .F. ) ;
#17059 = DIRECTION ( 'NONE',  ( 0.000000000000000000, 0.000000000000000000, 1.000000000000000000 ) ) ;
#17060 = EDGE_LOOP ( 'NONE', ( #34937, #3438, #45350, #9053 ) ) ;
#17061 = LINE ( 'NONE', #46207, #11099 ) ;
#17062 = CARTESIAN_POINT ( 'NONE',  ( 12.50000000000000000, -120.0000000000000000, 40.00000000000000711 ) ) ;
#17064 = EDGE_CURVE ( 'NONE', #35099, #2146, #5132, .T. ) ;
#17063 = STYLED_ITEM ( 'NONE', ( #20831 ), #35626 ) ;
#17065 = DIRECTION ( 'NONE',  ( -1.000000000000000000, -0.000000000000000000, -0.000000000000000000 ) ) ;
#17066 = CARTESIAN_POINT ( 'NONE',  ( -42.50000000000000000, 0.000000000000000000, 0.000000000000000000 ) ) ;
#17067 = FACE_OUTER_BOUND ( 'NONE', #8789, .T. ) ;
#17068 = EDGE_CURVE ( 'NONE', #36858, #6148, #23317, .T. ) ;
#17069 = AXIS2_PLACEMENT_3D ( 'NONE', #6470, #32186, #17720 ) ;
#17070 = EDGE_LOOP ( 'NONE', ( #21467, #603, #21588, #8911 ) ) ;
#17071 = EDGE_CURVE ( 'NONE', #7858, #4059, #26751, .T. ) ;
#17072 = DIRECTION ( 'NONE',  ( 0.000000000000000000, 0.000000000000000000, 1.000000000000000000 ) ) ;
#17073 = EDGE_CURVE ( 'NONE', #37535, #13263, #8616, .T. ) ;
#17074 = DIRECTION ( 'NONE',  ( -1.000000000000000000, 0.000000000000000000, 0.000000000000000000 ) ) ;
#17075 = VERTEX_POINT ( 'NONE', #33841 ) ;
#17076 = EDGE_CURVE ( 'NONE', #24143, #25916, #11586, .T. ) ;
#17077 = DIRECTION ( 'NONE',  ( -1.000000000000000000, 0.000000000000000000, 0.000000000000000000 ) ) ;
#17078 = ORIENTED_EDGE ( 'NONE', *, *, #14320, .F. ) ;
#17079 = CARTESIAN_POINT ( 'NONE',  ( 0.000000000000000000, 51.29473840253223216, 63.97538442413444670 ) ) ;
#17080 = CARTESIAN_POINT ( 'NONE',  ( -10.00000000000000000, 0.000000000000000000, 0.000000000000000000 ) ) ;
#17081 = DIRECTION ( 'NONE',  ( 0.000000000000000000, 0.1564344650402244852, 0.9876883405951387696 ) ) ;
#17082 = ORIENTED_EDGE ( 'NONE', *, *, #5301, .F. ) ;
#17083 = AXIS2_PLACEMENT_3D ( 'NONE', #55, #29925, #37509 ) ;
#17084 = CARTESIAN_POINT ( 'NONE',  ( 11.99999999999999822, 77.32052557432841411, 5.256550761633121738 ) ) ;
#17085 = ADVANCED_FACE ( 'NONE', ( #4716 ), #37521, .T. ) ;
#17086 = CARTESIAN_POINT ( 'NONE',  ( 10.00000000000000000, -37.01155633439063308, 6.555932627142289526 ) ) ;
#17087 = DIRECTION ( 'NONE',  ( 0.000000000000000000, 1.000000000000000000, 3.469446951953614189E-15 ) ) ;
#17088 = ORIENTED_EDGE ( 'NONE', *, *, #1215, .T. ) ;
#17089 = DIRECTION ( 'NONE',  ( 0.000000000000000000, 0.000000000000000000, 1.000000000000000000 ) ) ;
#17090 = DIRECTION ( 'NONE',  ( -0.6516173805718079581, 0.7585478161175706058, 0.000000000000000000 ) ) ;
#17091 = CARTESIAN_POINT ( 'NONE',  ( 10.00000000000000000, 50.95692526931414790, -58.39081064771693974 ) ) ;
#17092 = EDGE_CURVE ( 'NONE', #39765, #24524, #1299, .T. ) ;
#17093 = DIRECTION ( 'NONE',  ( -1.000000000000000000, 0.000000000000000000, 0.000000000000000000 ) ) ;
#17094 =( NAMED_UNIT ( * ) SI_UNIT ( $, .STERADIAN. ) SOLID_ANGLE_UNIT ( ) );
#17095 = ORIENTED_EDGE ( 'NONE', *, *, #43811, .F. ) ;
#17096 = ORIENTED_EDGE ( 'NONE', *, *, #34137, .F. ) ;
#17097 = EDGE_CURVE ( 'NONE', #35782, #4856, #15268, .T. ) ;
#17098 = VECTOR ( 'NONE', #1227, 1000.000000000000000 ) ;
#17099 = ORIENTED_EDGE ( 'NONE', *, *, #24428, .T. ) ;
#17100 = AXIS2_PLACEMENT_3D ( 'NONE', #27646, #42583, #20286 ) ;
#17101 = VECTOR ( 'NONE', #17796, 1000.000000000000114 ) ;
#17102 = CYLINDRICAL_SURFACE ( 'NONE', #1494, 16.00000000000000000 ) ;
#17103 = CARTESIAN_POINT ( 'NONE',  ( 10.00000000000000000, 73.72996012237460661, -14.67089635893632504 ) ) ;
#17104 = AXIS2_PLACEMENT_3D ( 'NONE', #33846, #23086, #26521 ) ;
#17105 = ORIENTED_EDGE ( 'NONE', *, *, #45881, .T. ) ;
#17106 = ADVANCED_FACE ( 'NONE', ( #22835 ), #37764, .T. ) ;
#17107 = CARTESIAN_POINT ( 'NONE',  ( 0.000000000000000000, 0.000000000000000000, 0.000000000000000000 ) ) ;
#17108 = ORIENTED_EDGE ( 'NONE', *, *, #3596, .T. ) ;
#17109 = ORIENTED_EDGE ( 'NONE', *, *, #28524, .F. ) ;
#17110 = ORIENTED_EDGE ( 'NONE', *, *, #27257, .F. ) ;
#17111 = VERTEX_POINT ( 'NONE', #5685 ) ;
#17112 = EDGE_CURVE ( 'NONE', #28620, #29568, #31654, .T. ) ;
#17113 = DIRECTION ( 'NONE',  ( 0.000000000000000000, 1.000000000000000000, 3.469446951953614978E-15 ) ) ;
#17114 = ORIENTED_EDGE ( 'NONE', *, *, #10678, .T. ) ;
#17115 = CARTESIAN_POINT ( 'NONE',  ( 0.000000000000000000, 37.01155633439068282, -6.555932627142014191 ) ) ;
#17116 = ORIENTED_EDGE ( 'NONE', *, *, #10228, .T. ) ;
#17117 = ADVANCED_FACE ( 'NONE', ( #20860 ), #9580, .T. ) ;
#17118 = DIRECTION ( 'NONE',  ( 0.000000000000000000, -0.6494480483301739993, -0.7604059656000390355 ) ) ;
#17119 = PLANE ( 'NONE',  #41095 ) ;
#17120 = DIRECTION ( 'NONE',  ( 0.000000000000000000, -0.8090169943749531134, 0.5877852522924653655 ) ) ;
#17121 = VERTEX_POINT ( 'NONE', #17167 ) ;
#17122 = EDGE_CURVE ( 'NONE', #36907, #17574, #17620, .T. ) ;
#17123 = DIRECTION ( 'NONE',  ( 0.000000000000000000, 0.000000000000000000, -1.000000000000000000 ) ) ;
#17124 = ORIENTED_EDGE ( 'NONE', *, *, #8119, .T. ) ;
#17125 = ORIENTED_EDGE ( 'NONE', *, *, #3010, .F. ) ;
#17126 = DIRECTION ( 'NONE',  ( 0.000000000000000000, 0.000000000000000000, 1.000000000000000000 ) ) ;
#17127 = DIRECTION ( 'NONE',  ( 0.000000000000000000, 0.000000000000000000, 1.000000000000000000 ) ) ;
#17128 = PLANE ( 'NONE',  #37369 ) ;
#17129 = ORIENTED_EDGE ( 'NONE', *, *, #34471, .T. ) ;
#17130 = VERTEX_POINT ( 'NONE', #2243 ) ;
#17131 = EDGE_CURVE ( 'NONE', #7846, #12203, #16704, .T. ) ;
#17132 = CARTESIAN_POINT ( 'NONE',  ( 0.000000000000000000, 0.000000000000000000, 0.000000000000000000 ) ) ;
#17133 = CARTESIAN_POINT ( 'NONE',  ( 10.00000000000000000, -76.41127070299262414, -12.93880638057396304 ) ) ;
#17134 = EDGE_LOOP ( 'NONE', ( #15165, #39846, #624, #1907 ) ) ;
#17135 = AXIS2_PLACEMENT_3D ( 'NONE', #896, #15844, #10967 ) ;
#17136 = CYLINDRICAL_SURFACE ( 'NONE', #40236, 42.00000000000000000 ) ;
#17137 = DIRECTION ( 'NONE',  ( 1.000000000000000000, 0.000000000000000000, 0.000000000000000000 ) ) ;
#17138 = CARTESIAN_POINT ( 'NONE',  ( 6.000000000000000000, -15.33399622253424432, -80.55351364060604169 ) ) ;
#17139 = LINE ( 'NONE', #28397, #33586 ) ;
#17140 = FACE_OUTER_BOUND ( 'NONE', #7910, .T. ) ;
#17141 = CARTESIAN_POINT ( 'NONE',  ( 10.00000000000000000, -33.80338159004296017, 16.23288003029484727 ) ) ;
#17142 = AXIS2_PLACEMENT_3D ( 'NONE', #30208, #7909, #22842 ) ;
#17143 = CARTESIAN_POINT ( 'NONE',  ( 10.00000000000000000, -37.58145647212455032, 0.6853352020789044152 ) ) ;
#17144 = DIRECTION ( 'NONE',  ( -1.000000000000000000, 0.000000000000000000, 0.000000000000000000 ) ) ;
#17145 = CARTESIAN_POINT ( 'NONE',  ( -2.981742216678212820, 0.000000000000000000, 0.000000000000000000 ) ) ;
#17146 =( NAMED_UNIT ( * ) SI_UNIT ( $, .STERADIAN. ) SOLID_ANGLE_UNIT ( ) );
#17147 = CARTESIAN_POINT ( 'NONE',  ( -2.499999999999997780, 8.494897427831771708, 0.000000000000000000 ) ) ;
#17148 = CYLINDRICAL_SURFACE ( 'NONE', #9960, 16.00000000000000000 ) ;
#17149 = VERTEX_POINT ( 'NONE', #16942 ) ;
#17150 = DIRECTION ( 'NONE',  ( 0.000000000000000000, 0.9876883405951382144, -0.1564344650402276493 ) ) ;
#17151 = CYLINDRICAL_SURFACE ( 'NONE', #14327, 35.50000000000000711 ) ;
#17152 = CARTESIAN_POINT ( 'NONE',  ( 10.00000000000000000, -44.88180994100329713, -63.18004540533077318 ) ) ;
#17153 = ORIENTED_EDGE ( 'NONE', *, *, #24692, .F. ) ;
#17154 = VERTEX_POINT ( 'NONE', #32124 ) ;
#17155 = VECTOR ( 'NONE', #10827, 1000.000000000000000 ) ;
#17156 = AXIS2_PLACEMENT_3D ( 'NONE', #10188, #10912, #20968 ) ;
#17157 = LINE ( 'NONE', #13748, #39049 ) ;
#17158 = VERTEX_POINT ( 'NONE', #21079 ) ;
#17159 = CARTESIAN_POINT ( 'NONE',  ( 11.99999999999999822, 69.42325613327440692, 34.44570377933622041 ) ) ;
#17160 = VECTOR ( 'NONE', #26559, 1000.000000000000000 ) ;
#17161 = VERTEX_POINT ( 'NONE', #39217 ) ;
#17162 = DIRECTION ( 'NONE',  ( -1.000000000000000000, -0.000000000000000000, 0.000000000000000000 ) ) ;
#17163 = CARTESIAN_POINT ( 'NONE',  ( 21.85433023846371370, -135.0628101570779620, 5.500000000000000000 ) ) ;
#17164 = CARTESIAN_POINT ( 'NONE',  ( 10.00000000000000000, 80.55351364060609853, -15.33399622253395478 ) ) ;
#17165 = EDGE_LOOP ( 'NONE', ( #38644, #546, #43154, #27375 ) ) ;
#17166 = EDGE_CURVE ( 'NONE', #30366, #16979, #5942, .T. ) ;
#17167 = CARTESIAN_POINT ( 'NONE',  ( 0.000000000000000000, 15.33399622253481986, 80.55351364060595643 ) ) ;
#17168 = ORIENTED_EDGE ( 'NONE', *, *, #35791, .F. ) ;
#17169 = EDGE_CURVE ( 'NONE', #38560, #7173, #31407, .T. ) ;
#17170 = CARTESIAN_POINT ( 'NONE',  ( 11.99999999999999822, 79.10210256391397365, -21.60688246758502729 ) ) ;
#17171 = DIRECTION ( 'NONE',  ( 0.000000000000000000, -0.8910065241883626808, -0.4539904997395568520 ) ) ;
#17172 = DIRECTION ( 'NONE',  ( 0.000000000000000000, -0.1564344650402170744, -0.9876883405951398798 ) ) ;
#17173 = CYLINDRICAL_SURFACE ( 'NONE', #37512, 82.00000000000000000 ) ;
#17174 = DIRECTION ( 'NONE',  ( 0.000000000000000000, 0.000000000000000000, 1.000000000000000000 ) ) ;
#17175 = EDGE_LOOP ( 'NONE', ( #19568, #26734, #32125, #16386 ) ) ;
#17176 = DIRECTION ( 'NONE',  ( 0.000000000000000000, 0.000000000000000000, 1.000000000000000000 ) ) ;
#17177 = VERTEX_POINT ( 'NONE', #28436 ) ;
#17178 = ORIENTED_EDGE ( 'NONE', *, *, #9821, .F. ) ;
#17179 = EDGE_CURVE ( 'NONE', #4059, #14947, #42896, .T. ) ;
#17180 = CARTESIAN_POINT ( 'NONE',  ( 0.000000000000000000, 0.000000000000000000, 0.000000000000000000 ) ) ;
#17181 = CARTESIAN_POINT ( 'NONE',  ( 11.99999999999999822, 77.32052557432841411, 5.256550761633121738 ) ) ;
#17182 = ADVANCED_FACE ( 'NONE', ( #46807 ), #42658, .T. ) ;
#17183 = DIRECTION ( 'NONE',  ( -0.000000000000000000, -0.000000000000000000, -1.000000000000000000 ) ) ;
#17184 = CARTESIAN_POINT ( 'NONE',  ( -3.000000000000000000, 6.762365576493643893, -25.66652317338391853 ) ) ;
#17185 = EDGE_LOOP ( 'NONE', ( #971, #18847, #39714, #2089 ) ) ;
#17186 = CARTESIAN_POINT ( 'NONE',  ( 5.000000000000000000, 74.74816331893477184, -33.71516098798660011 ) ) ;
#17187 = DIRECTION ( 'NONE',  ( 0.000000000000000000, -0.7431448254773954654, 0.6691306063588569053 ) ) ;
#17188 = LINE ( 'NONE', #40213, #4800 ) ;
#17189 = CARTESIAN_POINT ( 'NONE',  ( 0.000000000000000000, -46.53671651293907274, -59.03961581697448935 ) ) ;
#17191 = AXIS2_PLACEMENT_3D ( 'NONE', #15640, #41841, #15172 ) ;
#17190 = LINE ( 'NONE', #13533, #14575 ) ;
#17192 = ORIENTED_EDGE ( 'NONE', *, *, #31810, .T. ) ;
#17193 = AXIS2_PLACEMENT_3D ( 'NONE', #6709, #21380, #32640 ) ;
#17194 = LINE ( 'NONE', #24559, #29356 ) ;
#17195 =( NAMED_UNIT ( * ) PLANE_ANGLE_UNIT ( ) SI_UNIT ( $, .RADIAN. ) );
#17196 = CARTESIAN_POINT ( 'NONE',  ( 26.47460221209471598, -121.8961639463267090, 5.500000000000000000 ) ) ;
#17197 = LINE ( 'NONE', #23170, #44148 ) ;
#17198 = DIRECTION ( 'NONE',  ( 1.000000000000000000, -0.000000000000000000, 0.000000000000000000 ) ) ;
#17199 = DIRECTION ( 'NONE',  ( -0.000000000000000000, -0.000000000000000000, -1.000000000000000000 ) ) ;
#17200 = ORIENTED_EDGE ( 'NONE', *, *, #21251, .T. ) ;
#17201 = AXIS2_PLACEMENT_3D ( 'NONE', #17486, #39783, #14562 ) ;
#17202 = EDGE_LOOP ( 'NONE', ( #19674, #25042, #4358, #15131 ) ) ;
#17203 = DIRECTION ( 'NONE',  ( 0.000000000000000000, 0.000000000000000000, 1.000000000000000000 ) ) ;
#17204 = ORIENTED_EDGE ( 'NONE', *, *, #25075, .F. ) ;
#17205 = DIRECTION ( 'NONE',  ( 0.000000000000000000, 0.000000000000000000, -1.000000000000000000 ) ) ;
#17206 = FACE_OUTER_BOUND ( 'NONE', #35234, .T. ) ;
#17207 = ORIENTED_EDGE ( 'NONE', *, *, #41842, .F. ) ;
#17208 = EDGE_CURVE ( 'NONE', #26919, #1546, #2773, .T. ) ;
#17209 = EDGE_CURVE ( 'NONE', #12329, #24320, #40320, .T. ) ;
#17210 = DIRECTION ( 'NONE',  ( 0.000000000000000000, 0.000000000000000000, 1.000000000000000000 ) ) ;
#17211 = ORIENTED_EDGE ( 'NONE', *, *, #9629, .F. ) ;
#17212 = ORIENTED_EDGE ( 'NONE', *, *, #12001, .T. ) ;
#17213 = ADVANCED_FACE ( 'NONE', ( #39715 ), #17404, .F. ) ;
#17214 = VECTOR ( 'NONE', #7238, 1000.000000000000000 ) ;
#17215 = DIRECTION ( 'NONE',  ( 0.000000000000000000, -0.1564344650402168801, -0.9876883405951399908 ) ) ;
#17216 = ORIENTED_EDGE ( 'NONE', *, *, #10539, .T. ) ;
#17217 = VECTOR ( 'NONE', #9831, 1000.000000000000000 ) ;
#17218 = DIRECTION ( 'NONE',  ( -0.7273375899149793211, 0.6862798483830554463, 0.000000000000000000 ) ) ;
#17219 = CARTESIAN_POINT ( 'NONE',  ( 0.000000000000000000, 37.01155633439059756, 6.555932627142549762 ) ) ;
#17220 = VECTOR ( 'NONE', #27811, 999.9999999999998863 ) ;
#17221 = AXIS2_PLACEMENT_3D ( 'NONE', #28684, #2719, #44081 ) ;
#17222 = ORIENTED_EDGE ( 'NONE', *, *, #29086, .T. ) ;
#17223 = DIRECTION ( 'NONE',  ( -1.000000000000000000, 0.000000000000000000, 0.000000000000000000 ) ) ;
#17224 = EDGE_CURVE ( 'NONE', #32354, #35720, #41857, .T. ) ;
#17225 = EDGE_LOOP ( 'NONE', ( #18899, #6210, #38431, #10051 ) ) ;
#17226 = AXIS2_PLACEMENT_3D ( 'NONE', #22550, #36983, #11776 ) ;
#17227 = EDGE_CURVE ( 'NONE', #29462, #48127, #35548, .T. ) ;
#17228 = EDGE_CURVE ( 'NONE', #23138, #21614, #9800, .T. ) ;
#17229 = DIRECTION ( 'NONE',  ( 0.000000000000000000, -0.8090169943749508930, 0.5877852522924682521 ) ) ;
#17230 = FACE_OUTER_BOUND ( 'NONE', #4878, .T. ) ;
#17231 = AXIS2_PLACEMENT_3D ( 'NONE', #36035, #5961, #24547 ) ;
#17232 = DIRECTION ( 'NONE',  ( -1.000000000000000000, -0.000000000000000000, -0.000000000000000000 ) ) ;
#17233 = VERTEX_POINT ( 'NONE', #35053 ) ;
#17234 = CIRCLE ( 'NONE', #15670, 82.00000000000000000 ) ;
#17235 = CARTESIAN_POINT ( 'NONE',  ( 10.00000000000000000, 0.000000000000000000, 0.000000000000000000 ) ) ;
#17236 = ORIENTED_EDGE ( 'NONE', *, *, #7008, .T. ) ;
#17237 = CARTESIAN_POINT ( 'NONE',  ( 10.00000000000000000, 0.000000000000000000, 0.000000000000000000 ) ) ;
#17238 = DIRECTION ( 'NONE',  ( -1.000000000000000000, 0.000000000000000000, 0.000000000000000000 ) ) ;
#17239 = CARTESIAN_POINT ( 'NONE',  ( 0.000000000000000000, -71.27951684758005513, -30.41916302227188851 ) ) ;
#17240 = CARTESIAN_POINT ( 'NONE',  ( 0.000000000000000000, 0.000000000000000000, 0.000000000000000000 ) ) ;
#17241 = DIRECTION ( 'NONE',  ( -1.000000000000000000, -0.000000000000000000, 0.000000000000000000 ) ) ;
#17242 = CARTESIAN_POINT ( 'NONE',  ( 10.00000000000000000, 6.736453364083557105, 36.88895765772635826 ) ) ;
#17243 = DIRECTION ( 'NONE',  ( 0.000000000000000000, 0.000000000000000000, 1.000000000000000000 ) ) ;
#17245 = EDGE_CURVE ( 'NONE', #43246, #31534, #12793, .T. ) ;
#17244 = CARTESIAN_POINT ( 'NONE',  ( 11.99999999999999822, 68.67312586194995561, 35.91791733033500122 ) ) ;
#17246 = CARTESIAN_POINT ( 'NONE',  ( 11.99999999999999822, -12.93880638057369659, 76.41127070299266677 ) ) ;
#17247 = LINE ( 'NONE', #32444, #39563 ) ;
#17248 = VERTEX_POINT ( 'NONE', #38984 ) ;
#17249 = ORIENTED_EDGE ( 'NONE', *, *, #46752, .T. ) ;
#17250 = CYLINDRICAL_SURFACE ( 'NONE', #27066, 31.99999999999998579 ) ;
#17251 = CARTESIAN_POINT ( 'NONE',  ( 10.00000000000000000, -68.26794271651286294, 31.47745569255117104 ) ) ;
#17252 = PLANE ( 'NONE',  #37013 ) ;
#17253 = DIRECTION ( 'NONE',  ( 0.000000000000000000, 0.000000000000000000, 1.000000000000000000 ) ) ;
#17254 = VECTOR ( 'NONE', #7201, 1000.000000000000000 ) ;
#17255 = ORIENTED_EDGE ( 'NONE', *, *, #27919, .F. ) ;
#17256 = CARTESIAN_POINT ( 'NONE',  ( 5.999999999999999112, 50.23322058963348979, 64.81221759200361987 ) ) ;
#17257 = CARTESIAN_POINT ( 'NONE',  ( 0.000000000000000000, 0.000000000000000000, 0.000000000000000000 ) ) ;
#17258 = VECTOR ( 'NONE', #31283, 1000.000000000000114 ) ;
#17259 = ORIENTED_EDGE ( 'NONE', *, *, #8053, .F. ) ;
#17260 = CARTESIAN_POINT ( 'NONE',  ( 50.00005079999999680, 1.530808498934191521E-15, -12.50000000000000000 ) ) ;
#17261 = AXIS2_PLACEMENT_3D ( 'NONE', #44891, #18459, #11844 ) ;
#17262 = AXIS2_PLACEMENT_3D ( 'NONE', #40371, #21024, #9772 ) ;
#17263 = ORIENTED_EDGE ( 'NONE', *, *, #33531, .T. ) ;
#17264 = DIRECTION ( 'NONE',  ( -1.000000000000000000, 0.000000000000000000, 0.000000000000000000 ) ) ;
#17265 = VECTOR ( 'NONE', #2204, 1000.000000000000000 ) ;
#17266 = ORIENTED_EDGE ( 'NONE', *, *, #1665, .T. ) ;
#17267 = VECTOR ( 'NONE', #28870, 1000.000000000000000 ) ;
#17268 = ADVANCED_FACE ( 'NONE', ( #5445 ), #24281, .T. ) ;
#17269 = AXIS2_PLACEMENT_3D ( 'NONE', #2156, #31302, #39615 ) ;
#17270 = VERTEX_POINT ( 'NONE', #7120 ) ;
#17271 = EDGE_CURVE ( 'NONE', #16099, #29948, #24995, .T. ) ;
#17272 = DIRECTION ( 'NONE',  ( -0.000000000000000000, -0.000000000000000000, -1.000000000000000000 ) ) ;
#17273 = VERTEX_POINT ( 'NONE', #37221 ) ;
#17274 = ADVANCED_FACE ( 'NONE', ( #36256 ), #43611, .T. ) ;
#17275 = VERTEX_POINT ( 'NONE', #21576 ) ;
#17276 = DIRECTION ( 'NONE',  ( -1.000000000000000000, -0.000000000000000000, 0.000000000000000000 ) ) ;
#17278 = ORIENTED_EDGE ( 'NONE', *, *, #22459, .F. ) ;
#17277 = DIRECTION ( 'NONE',  ( -1.000000000000000000, -0.000000000000000000, -0.000000000000000000 ) ) ;
#17279 = VERTEX_POINT ( 'NONE', #29145 ) ;
#17280 = VERTEX_POINT ( 'NONE', #36496 ) ;
#17281 = ORIENTED_EDGE ( 'NONE', *, *, #21784, .F. ) ;
#17282 = EDGE_CURVE ( 'NONE', #11314, #15196, #34807, .T. ) ;
#17283 = ADVANCED_FACE ( 'NONE', ( #13985 ), #11075, .T. ) ;
#17284 = CARTESIAN_POINT ( 'NONE',  ( 10.00000000000000000, -4.992566952384716927, -37.16516213103282951 ) ) ;
#17285 = DIRECTION ( 'NONE',  ( 1.000000000000000000, 0.000000000000000000, 0.000000000000000000 ) ) ;
#17286 = CIRCLE ( 'NONE', #6377, 37.49900000000000233 ) ;
#17287 = DIRECTION ( 'NONE',  ( -1.000000000000000000, 0.000000000000000000, 0.000000000000000000 ) ) ;
#17289 = VERTEX_POINT ( 'NONE', #2958 ) ;
#17288 = CIRCLE ( 'NONE', #23549, 31.99999999999999289 ) ;
#17290 = VERTEX_POINT ( 'NONE', #17885 ) ;
#17291 = CARTESIAN_POINT ( 'NONE',  ( 0.000000000000000000, -6.736453364083290651, -36.88895765772640090 ) ) ;
#17292 = VERTEX_POINT ( 'NONE', #43841 ) ;
#17293 = DIRECTION ( 'NONE',  ( -1.000000000000000000, 0.000000000000000000, -0.000000000000000000 ) ) ;
#17294 = ORIENTED_EDGE ( 'NONE', *, *, #19001, .F. ) ;
#17295 = CIRCLE ( 'NONE', #12640, 31.99999999999998934 ) ;
#17296 = DIRECTION ( 'NONE',  ( -1.000000000000000000, -0.000000000000000000, -0.000000000000000000 ) ) ;
#17297 = FACE_BOUND ( 'NONE', #35731, .T. ) ;
#17298 = DIRECTION ( 'NONE',  ( 0.000000000000000000, 0.000000000000000000, -1.000000000000000000 ) ) ;
#17299 = CARTESIAN_POINT ( 'NONE',  ( 0.000000000000000000, 30.80686688397010542, 21.53537804866092387 ) ) ;
#17300 = VECTOR ( 'NONE', #14628, 1000.000000000000000 ) ;
#17301 = DIRECTION ( 'NONE',  ( 0.000000000000000000, 0.9238795325112877377, -0.3826834323650873948 ) ) ;
#17302 = ADVANCED_FACE ( 'NONE', ( #47990 ), #36971, .T. ) ;
#17303 = DIRECTION ( 'NONE',  ( -1.000000000000000000, 0.000000000000000000, -0.000000000000000000 ) ) ;
#17304 = ORIENTED_EDGE ( 'NONE', *, *, #11208, .T. ) ;
#17305 = AXIS2_PLACEMENT_3D ( 'NONE', #43683, #40018, #21402 ) ;
#17306 = CARTESIAN_POINT ( 'NONE',  ( 11.99999999999999822, 14.67089635893819377, -73.72996012237423713 ) ) ;
#17307 = VERTEX_POINT ( 'NONE', #6406 ) ;
#17308 = AXIS2_PLACEMENT_3D ( 'NONE', #23740, #28141, #46988 ) ;
#17309 = CARTESIAN_POINT ( 'NONE',  ( 0.000000000000000000, 0.000000000000000000, 0.000000000000000000 ) ) ;
#17310 = CARTESIAN_POINT ( 'NONE',  ( -3.000000000000000000, 5.835314593368477354, 22.81335362449854642 ) ) ;
#17311 = DIRECTION ( 'NONE',  ( 0.000000000000000000, 0.000000000000000000, 1.000000000000000000 ) ) ;
#17312 = DIRECTION ( 'NONE',  ( 1.000000000000000000, -0.000000000000000000, 0.000000000000000000 ) ) ;
#17313 = CARTESIAN_POINT ( 'NONE',  ( 0.000000000000000000, 68.26794271651262136, 31.47745569255165066 ) ) ;
#17314 = FACE_OUTER_BOUND ( 'NONE', #1939, .T. ) ;
#17315 = ORIENTED_EDGE ( 'NONE', *, *, #44478, .F. ) ;
#17316 = CARTESIAN_POINT ( 'NONE',  ( -3.000000000000000000, 14.60985201121729737, -18.46759930825687945 ) ) ;
#17317 = CARTESIAN_POINT ( 'NONE',  ( -12.40464318976454727, 10.41032311384371667, -45.00000000000000000 ) ) ;
#17318 = CARTESIAN_POINT ( 'NONE',  ( 11.99999999999999822, 8.830959090342393125, 74.65491531819122883 ) ) ;
#17319 = CARTESIAN_POINT ( 'NONE',  ( 12.00000000000000000, -0.9646360437375368635, -23.52805723605589705 ) ) ;
#17320 = PRESENTATION_STYLE_ASSIGNMENT (( #16615 ) ) ;
#17321 = VERTEX_POINT ( 'NONE', #47286 ) ;
#17322 = ORIENTED_EDGE ( 'NONE', *, *, #34310, .T. ) ;
#17323 = ORIENTED_EDGE ( 'NONE', *, *, #26246, .T. ) ;
#17324 = CIRCLE ( 'NONE', #34507, 82.00000000000000000 ) ;
#17325 = CIRCLE ( 'NONE', #24362, 37.49900000000000233 ) ;
#17326 = VERTEX_POINT ( 'NONE', #29635 ) ;
#17327 = AXIS2_PLACEMENT_3D ( 'NONE', #12553, #27491, #12796 ) ;
#17328 = EDGE_CURVE ( 'NONE', #28782, #37765, #12650, .T. ) ;
#17329 = DIRECTION ( 'NONE',  ( 0.000000000000000000, 0.000000000000000000, 1.000000000000000000 ) ) ;
#17330 = CARTESIAN_POINT ( 'NONE',  ( 11.99999999999999822, 39.47590169984846398, 71.87247863392425984 ) ) ;
#17331 = ORIENTED_EDGE ( 'NONE', *, *, #33257, .T. ) ;
#17332 = EDGE_CURVE ( 'NONE', #7964, #5993, #36837, .T. ) ;
#17333 = VECTOR ( 'NONE', #37064, 1000.000000000000000 ) ;
#17334 = ADVANCED_FACE ( 'NONE', ( #40904 ), #3693, .T. ) ;
#17335 = CARTESIAN_POINT ( 'NONE',  ( 10.00000000000000000, 11.30684508768452545, -76.66974797899825944 ) ) ;
#17336 = VECTOR ( 'NONE', #33002, 1000.000000000000000 ) ;
#17337 = VERTEX_POINT ( 'NONE', #18380 ) ;
#17338 = VERTEX_POINT ( 'NONE', #33062 ) ;
#17339 = ORIENTED_EDGE ( 'NONE', *, *, #47420, .T. ) ;
#17340 = EDGE_CURVE ( 'NONE', #21962, #40162, #32360, .T. ) ;
#17341 = CARTESIAN_POINT ( 'NONE',  ( 10.00000000000000000, -35.92658777277517856, 10.74501242461269257 ) ) ;
#17342 = VERTEX_POINT ( 'NONE', #44330 ) ;
#17343 = DIRECTION ( 'NONE',  ( 0.000000000000000000, 0.000000000000000000, 1.000000000000000000 ) ) ;
#17344 = EDGE_CURVE ( 'NONE', #41379, #21334, #10803, .T. ) ;
#17345 = ORIENTED_EDGE ( 'NONE', *, *, #16256, .T. ) ;
#17346 = CYLINDRICAL_SURFACE ( 'NONE', #29858, 16.00000000000000000 ) ;
#17347 = VECTOR ( 'NONE', #12692, 1000.000000000000000 ) ;
#17348 = DIRECTION ( 'NONE',  ( 0.000000000000000000, 0.000000000000000000, 1.000000000000000000 ) ) ;
#17349 = DIRECTION ( 'NONE',  ( -1.000000000000000000, 0.000000000000000000, 0.000000000000000000 ) ) ;
#17350 = VERTEX_POINT ( 'NONE', #28907 ) ;
#17351 = DIRECTION ( 'NONE',  ( -0.02332147558787674158, -0.9997280174009349762, 0.000000000000000000 ) ) ;
#17352 = ORIENTED_EDGE ( 'NONE', *, *, #13185, .F. ) ;
#17353 = VECTOR ( 'NONE', #3541, 1000.000000000000000 ) ;
#17354 = DIRECTION ( 'NONE',  ( 1.000000000000000000, 0.000000000000000000, 0.000000000000000000 ) ) ;
#17355 = ADVANCED_FACE ( 'NONE', ( #28688 ), #33313, .T. ) ;
#17356 = DIRECTION ( 'NONE',  ( 0.000000000000000000, 0.7071067811865487940, -0.7071067811865462405 ) ) ;
#17357 = EDGE_LOOP ( 'NONE', ( #29037, #43784, #26473, #43725 ) ) ;
#17358 = ORIENTED_EDGE ( 'NONE', *, *, #47210, .F. ) ;
#17359 = DIRECTION ( 'NONE',  ( 0.000000000000000000, -0.7071067811865389130, -0.7071067811865561215 ) ) ;
#17360 = DIRECTION ( 'NONE',  ( 0.000000000000000000, -0.3090169943749548342, 0.9510565162951511997 ) ) ;
#17361 = ORIENTED_EDGE ( 'NONE', *, *, #772, .T. ) ;
#17362 = VECTOR ( 'NONE', #38200, 1000.000000000000000 ) ;
#17363 = ORIENTED_EDGE ( 'NONE', *, *, #7083, .F. ) ;
#17364 = DIRECTION ( 'NONE',  ( 1.000000000000000000, 0.000000000000000000, 0.000000000000000000 ) ) ;
#17365 = DIRECTION ( 'NONE',  ( 1.000000000000000000, 0.000000000000000000, 0.000000000000000000 ) ) ;
#17366 = DIRECTION ( 'NONE',  ( -1.000000000000000000, -0.000000000000000000, 0.000000000000000000 ) ) ;
#17367 = DIRECTION ( 'NONE',  ( 0.000000000000000000, 0.000000000000000000, 1.000000000000000000 ) ) ;
#17368 = VECTOR ( 'NONE', #46342, 1000.000000000000000 ) ;
#17369 = FACE_OUTER_BOUND ( 'NONE', #15339, .T. ) ;
#17370 = EDGE_CURVE ( 'NONE', #12813, #20184, #10304, .T. ) ;
#17371 = ORIENTED_EDGE ( 'NONE', *, *, #31569, .T. ) ;
#17372 = DIRECTION ( 'NONE',  ( -1.000000000000000000, 0.000000000000000000, 0.000000000000000000 ) ) ;
#17373 = LINE ( 'NONE', #39910, #5120 ) ;
#17374 = AXIS2_PLACEMENT_3D ( 'NONE', #22150, #37081, #14328 ) ;
#17375 = DIRECTION ( 'NONE',  ( -1.000000000000000000, 0.000000000000000000, 0.000000000000000000 ) ) ;
#17376 = CARTESIAN_POINT ( 'NONE',  ( 10.00000000000000000, 0.000000000000000000, 0.000000000000000000 ) ) ;
#17377 = CARTESIAN_POINT ( 'NONE',  ( 10.00000000000000000, 0.000000000000000000, 0.000000000000000000 ) ) ;
#17378 = CARTESIAN_POINT ( 'NONE',  ( 0.000000000000000000, 0.000000000000000000, 0.000000000000000000 ) ) ;
#17379 = DIRECTION ( 'NONE',  ( -1.000000000000000000, 0.000000000000000000, 0.000000000000000000 ) ) ;
#17380 = VERTEX_POINT ( 'NONE', #6650 ) ;
#17381 = VERTEX_POINT ( 'NONE', #42109 ) ;
#17382 = EDGE_CURVE ( 'NONE', #7173, #24762, #26217, .T. ) ;
#17383 = CARTESIAN_POINT ( 'NONE',  ( 0.000000000000000000, 0.000000000000000000, 0.000000000000000000 ) ) ;
#17384 = VECTOR ( 'NONE', #14433, 1000.000000000000000 ) ;
#17385 = EDGE_CURVE ( 'NONE', #3686, #37417, #34491, .T. ) ;
#17386 = LINE ( 'NONE', #24268, #12826 ) ;
#17387 = VERTEX_POINT ( 'NONE', #30864 ) ;
#17388 = EDGE_CURVE ( 'NONE', #27870, #46797, #38197, .T. ) ;
#17389 = VECTOR ( 'NONE', #542, 1000.000000000000000 ) ;
#17390 = VERTEX_POINT ( 'NONE', #30377 ) ;
#17391 = EDGE_CURVE ( 'NONE', #3376, #45432, #39204, .T. ) ;
#17392 = CYLINDRICAL_SURFACE ( 'NONE', #27345, 82.00000000000000000 ) ;
#17393 = AXIS2_PLACEMENT_3D ( 'NONE', #16843, #27611, #42549 ) ;
#17394 = CARTESIAN_POINT ( 'NONE',  ( 10.00000000000000000, 9.188173127307297960, 40.98264845739753071 ) ) ;
#17395 = CIRCLE ( 'NONE', #33054, 12.79999999999999893 ) ;
#17396 = ORIENTED_EDGE ( 'NONE', *, *, #32174, .F. ) ;
#17397 = CIRCLE ( 'NONE', #19779, 82.00000000000000000 ) ;
#17398 = ORIENTED_EDGE ( 'NONE', *, *, #4039, .T. ) ;
#17399 = ORIENTED_EDGE ( 'NONE', *, *, #36997, .T. ) ;
#17400 = FACE_OUTER_BOUND ( 'NONE', #3437, .T. ) ;
#17401 = AXIS2_PLACEMENT_3D ( 'NONE', #47114, #9918, #40021 ) ;
#17402 = CARTESIAN_POINT ( 'NONE',  ( 12.00000000000000000, 22.07842321921492612, 8.187992925817123790 ) ) ;
#17403 = VERTEX_POINT ( 'NONE', #248 ) ;
#17404 = PLANE ( 'NONE',  #25441 ) ;
#17405 = CIRCLE ( 'NONE', #36972, 82.00000000000000000 ) ;
#17406 = ORIENTED_EDGE ( 'NONE', *, *, #33644, .F. ) ;
#17407 = ORIENTED_EDGE ( 'NONE', *, *, #46634, .T. ) ;
#17408 = CARTESIAN_POINT ( 'NONE',  ( 10.00000000000000000, 73.95703589263975175, 23.16143007188454206 ) ) ;
#17409 = CYLINDRICAL_SURFACE ( 'NONE', #38553, 77.49899999999999523 ) ;
#17410 = CARTESIAN_POINT ( 'NONE',  ( 10.00000000000000000, 0.000000000000000000, 0.000000000000000000 ) ) ;
#17412 = ORIENTED_EDGE ( 'NONE', *, *, #23038, .F. ) ;
#17411 = CARTESIAN_POINT ( 'NONE',  ( 10.00000000000000000, 33.71516098798847594, -74.74816331893393340 ) ) ;
#17413 = EDGE_CURVE ( 'NONE', #25302, #17158, #38424, .T. ) ;
#17414 = DIRECTION ( 'NONE',  ( 1.000000000000000000, 0.000000000000000000, 0.000000000000000000 ) ) ;
#17415 = ORIENTED_EDGE ( 'NONE', *, *, #3021, .F. ) ;
#17416 = DIRECTION ( 'NONE',  ( 1.000000000000000000, -0.000000000000000000, -0.000000000000000000 ) ) ;
#17417 = ORIENTED_EDGE ( 'NONE', *, *, #19584, .F. ) ;
#17418 = ORIENTED_EDGE ( 'NONE', *, *, #40350, .F. ) ;
#17419 = CARTESIAN_POINT ( 'NONE',  ( 10.00000000000000178, 12.24744871391589207, -2.500000000000000000 ) ) ;
#17420 = ORIENTED_EDGE ( 'NONE', *, *, #6306, .F. ) ;
#17421 = DIRECTION ( 'NONE',  ( -1.000000000000000000, 0.000000000000000000, 0.000000000000000000 ) ) ;
#17422 = DIRECTION ( 'NONE',  ( -1.000000000000000000, 0.000000000000000000, 0.000000000000000000 ) ) ;
#17423 = CARTESIAN_POINT ( 'NONE',  ( 0.000000000000000000, -2.956366410621191765, 75.11725578898467859 ) ) ;
#17424 = ORIENTED_EDGE ( 'NONE', *, *, #4208, .F. ) ;
#17425 = DIRECTION ( 'NONE',  ( 1.000000000000000000, 0.000000000000000000, 0.000000000000000000 ) ) ;
#17426 = AXIS2_PLACEMENT_3D ( 'NONE', #26737, #15483, #18427 ) ;
#17427 = DIRECTION ( 'NONE',  ( 0.000000000000000000, 0.000000000000000000, 1.000000000000000000 ) ) ;
#17428 = DIRECTION ( 'NONE',  ( 0.000000000000000000, 0.4539904997395477482, -0.8910065241883674547 ) ) ;
#17429 = AXIS2_PLACEMENT_3D ( 'NONE', #38961, #5418, #1271 ) ;
#17430 = DIRECTION ( 'NONE',  ( -1.000000000000000000, -0.000000000000000000, -0.000000000000000000 ) ) ;
#17431 = EDGE_CURVE ( 'NONE', #43019, #14493, #36077, .T. ) ;
#17432 = ORIENTED_EDGE ( 'NONE', *, *, #21547, .F. ) ;
#17433 = LINE ( 'NONE', #35083, #33238 ) ;
#17434 = CARTESIAN_POINT ( 'NONE',  ( -3.000000000000000000, -22.67460108101783334, 6.353146135317912169 ) ) ;
#17435 = CARTESIAN_POINT ( 'NONE',  ( -3.000000000000000000, -18.13022148937263012, 15.02647892043544608 ) ) ;
#17436 = DIRECTION ( 'NONE',  ( -0.000000000000000000, -0.000000000000000000, -1.000000000000000000 ) ) ;
#17437 = AXIS2_PLACEMENT_3D ( 'NONE', #12443, #258, #41163 ) ;
#17438 = AXIS2_PLACEMENT_3D ( 'NONE', #28810, #40791, #29298 ) ;
#17439 = VERTEX_POINT ( 'NONE', #45792 ) ;
#17440 = DIRECTION ( 'NONE',  ( 0.000000000000000000, -0.3090169943749349057, -0.9510565162951577500 ) ) ;
#17441 = DIRECTION ( 'NONE',  ( 0.000000000000000000, 0.4539904997395413089, 0.8910065241883705633 ) ) ;
#17442 = VECTOR ( 'NONE', #14635, 1000.000000000000000 ) ;
#17443 = ORIENTED_EDGE ( 'NONE', *, *, #30844, .F. ) ;
#17444 = VERTEX_POINT ( 'NONE', #30606 ) ;
#17446 = DIRECTION ( 'NONE',  ( 0.000000000000000000, 0.000000000000000000, 1.000000000000000000 ) ) ;
#17445 = CIRCLE ( 'NONE', #4302, 31.99999999999998579 ) ;
#17447 = VECTOR ( 'NONE', #15517, 1000.000000000000000 ) ;
#17448 = VERTEX_POINT ( 'NONE', #41156 ) ;
#17449 = EDGE_CURVE ( 'NONE', #21422, #42780, #15925, .T. ) ;
#17450 = CARTESIAN_POINT ( 'NONE',  ( 10.00000000000000000, -16.65560815589383381, -38.55633173627028754 ) ) ;
#17451 = AXIS2_PLACEMENT_3D ( 'NONE', #30418, #554, #4944 ) ;
#17452 = ADVANCED_FACE ( 'NONE', ( #22774 ), #512, .T. ) ;
#17453 = DIRECTION ( 'NONE',  ( -1.000000000000000000, 0.000000000000000000, -0.000000000000000000 ) ) ;
#17454 = AXIS2_PLACEMENT_3D ( 'NONE', #6941, #28964, #32638 ) ;
#17455 = ORIENTED_EDGE ( 'NONE', *, *, #45822, .F. ) ;
#17456 = EDGE_CURVE ( 'NONE', #12155, #17273, #735, .T. ) ;
#17457 = CYLINDRICAL_SURFACE ( 'NONE', #27748, 42.00000000000000000 ) ;
#17459 = EDGE_CURVE ( 'NONE', #14267, #40188, #5591, .T. ) ;
#17458 = ORIENTED_EDGE ( 'NONE', *, *, #6695, .F. ) ;
#17460 = VERTEX_POINT ( 'NONE', #7 ) ;
#17461 = VECTOR ( 'NONE', #5364, 1000.000000000000000 ) ;
#17462 = CARTESIAN_POINT ( 'NONE',  ( 11.99999999999999822, -54.21277698773713638, 55.38113227695764351 ) ) ;
#17463 = CARTESIAN_POINT ( 'NONE',  ( 10.00000000000000000, 30.00120703465205452, 22.64427369931179967 ) ) ;
#17464 = AXIS2_PLACEMENT_3D ( 'NONE', #23828, #19648, #42425 ) ;
#17465 = VECTOR ( 'NONE', #6540, 1000.000000000000000 ) ;
#17466 = DIRECTION ( 'NONE',  ( 0.000000000000000000, 0.000000000000000000, 1.000000000000000000 ) ) ;
#17467 = VECTOR ( 'NONE', #39696, 1000.000000000000000 ) ;
#17468 = ORIENTED_EDGE ( 'NONE', *, *, #37371, .F. ) ;
#17469 = CARTESIAN_POINT ( 'NONE',  ( 5.000000000000000000, -27.74655509720725988, 77.16300072079653205 ) ) ;
#17470 = VERTEX_POINT ( 'NONE', #4659 ) ;
#17471 = ORIENTED_EDGE ( 'NONE', *, *, #1150, .T. ) ;
#17472 = EDGE_CURVE ( 'NONE', #37298, #12589, #41880, .T. ) ;
#17473 = DIRECTION ( 'NONE',  ( -1.000000000000000000, -0.000000000000000000, -0.000000000000000000 ) ) ;
#17474 = LINE ( 'NONE', #48067, #10856 ) ;
#17475 = DIRECTION ( 'NONE',  ( -1.000000000000000000, -0.000000000000000000, -0.000000000000000000 ) ) ;
#17476 = CIRCLE ( 'NONE', #33894, 32.50000000000000000 ) ;
#17477 = CIRCLE ( 'NONE', #46387, 82.00000000000000000 ) ;
#17478 = ORIENTED_EDGE ( 'NONE', *, *, #42634, .T. ) ;
#17479 = FACE_OUTER_BOUND ( 'NONE', #41847, .T. ) ;
#17480 = ORIENTED_EDGE ( 'NONE', *, *, #4613, .F. ) ;
#17481 = ORIENTED_EDGE ( 'NONE', *, *, #11694, .T. ) ;
#17482 = CIRCLE ( 'NONE', #22941, 31.99999999999999289 ) ;
#17483 = CARTESIAN_POINT ( 'NONE',  ( 2.117611129180199558, -93.54218975225703048, 5.500000000000000000 ) ) ;
#17484 = AXIS2_PLACEMENT_3D ( 'NONE', #40632, #32796, #47723 ) ;
#17485 = FACE_OUTER_BOUND ( 'NONE', #27153, .T. ) ;
#17486 = CARTESIAN_POINT ( 'NONE',  ( 0.000000000000000000, 72.35160999960817207, 20.41045688087850607 ) ) ;
#17487 = CARTESIAN_POINT ( 'NONE',  ( -2.500000000000000000, 16.00000000000000000, -10.00000000000000178 ) ) ;
#17488 = CARTESIAN_POINT ( 'NONE',  ( 11.99999999999999822, -55.38113227695745167, -54.21277698773732823 ) ) ;
#17489 = AXIS2_PLACEMENT_3D ( 'NONE', #34809, #24278, #1294 ) ;
#17490 = CARTESIAN_POINT ( 'NONE',  ( 0.000000000000000000, 6.555932627142418312, 37.01155633439060466 ) ) ;
#17491 = DIRECTION ( 'NONE',  ( -1.000000000000000000, 0.000000000000000000, 0.000000000000000000 ) ) ;
#17492 = LINE ( 'NONE', #25314, #24633 ) ;
#17493 = DIRECTION ( 'NONE',  ( 0.000000000000000000, -0.9969173337331271867, -0.07845909572785571273 ) ) ;
#17494 = DIRECTION ( 'NONE',  ( -1.000000000000000000, -0.000000000000000000, 0.000000000000000000 ) ) ;
#17495 = VERTEX_POINT ( 'NONE', #45290 ) ;
#17496 = EDGE_LOOP ( 'NONE', ( #16630, #22279, #35561, #34261 ) ) ;
#17497 = FACE_OUTER_BOUND ( 'NONE', #13736, .T. ) ;
#17498 = EDGE_CURVE ( 'NONE', #31053, #26390, #7611, .T. ) ;
#17499 = CARTESIAN_POINT ( 'NONE',  ( 0.000000000000000000, 0.000000000000000000, 0.000000000000000000 ) ) ;
#17500 = CARTESIAN_POINT ( 'NONE',  ( 11.99999999999999822, -76.66974797899830207, -11.30684508768420571 ) ) ;
#17501 = ADVANCED_FACE ( 'NONE', ( #11533 ), #15445, .T. ) ;
#17502 = DIRECTION ( 'NONE',  ( -1.000000000000000000, 0.000000000000000000, -0.000000000000000000 ) ) ;
#17503 = CIRCLE ( 'NONE', #24533, 82.00000000000000000 ) ;
#17504 = AXIS2_PLACEMENT_3D ( 'NONE', #32833, #6426, #14248 ) ;
#17505 = CARTESIAN_POINT ( 'NONE',  ( 10.00000000000000000, 22.74946021919175720, -29.81001611430984255 ) ) ;
#17506 = DIRECTION ( 'NONE',  ( 0.000000000000000000, 0.000000000000000000, -1.000000000000000000 ) ) ;
#17507 = ORIENTED_EDGE ( 'NONE', *, *, #30550, .F. ) ;
#17508 = AXIS2_PLACEMENT_3D ( 'NONE', #33739, #15633, #7574 ) ;
#17510 = CIRCLE ( 'NONE', #23771, 16.00000000000000000 ) ;
#17509 = DIRECTION ( 'NONE',  ( -1.000000000000000000, -0.000000000000000000, -0.000000000000000000 ) ) ;
#17511 = CIRCLE ( 'NONE', #46457, 82.00000000000000000 ) ;
#17512 = ADVANCED_FACE ( 'NONE', ( #11293 ), #37469, .F. ) ;
#17513 = DIRECTION ( 'NONE',  ( -1.000000000000000000, 0.000000000000000000, -0.000000000000000000 ) ) ;
#17514 = ADVANCED_FACE ( 'NONE', ( #34029, #41622 ), #8086, .F. ) ;
#17515 = EDGE_CURVE ( 'NONE', #19820, #27599, #27925, .T. ) ;
#17516 = VERTEX_POINT ( 'NONE', #42348 ) ;
#17517 = ORIENTED_EDGE ( 'NONE', *, *, #45336, .T. ) ;
#17518 = AXIS2_PLACEMENT_3D ( 'NONE', #7157, #40689, #14515 ) ;
#17519 = VECTOR ( 'NONE', #19776, 1000.000000000000000 ) ;
#17520 = VECTOR ( 'NONE', #23188, 1000.000000000000114 ) ;
#17521 = EDGE_CURVE ( 'NONE', #43442, #27549, #21225, .T. ) ;
#17522 = CARTESIAN_POINT ( 'NONE',  ( 5.000000000000000000, -36.13751322684404244, -21.40280677340410165 ) ) ;
#17523 = ORIENTED_EDGE ( 'NONE', *, *, #22101, .F. ) ;
#17524 = AXIS2_PLACEMENT_3D ( 'NONE', #12472, #1213, #19791 ) ;
#17525 = ORIENTED_EDGE ( 'NONE', *, *, #5376, .T. ) ;
#17526 = DIRECTION ( 'NONE',  ( 0.000000000000000000, -0.4539904997395540764, 0.8910065241883642351 ) ) ;
#17528 = VERTEX_POINT ( 'NONE', #5629 ) ;
#17527 = DIRECTION ( 'NONE',  ( -1.000000000000000000, -0.000000000000000000, 0.000000000000000000 ) ) ;
#17529 = EDGE_CURVE ( 'NONE', #15797, #38112, #7944, .T. ) ;
#17530 = ORIENTED_EDGE ( 'NONE', *, *, #4499, .T. ) ;
#17531 = EDGE_LOOP ( 'NONE', ( #23819, #38118, #20627, #32646 ) ) ;
#17532 = AXIS2_PLACEMENT_3D ( 'NONE', #14990, #12462, #37256 ) ;
#17533 = ORIENTED_EDGE ( 'NONE', *, *, #25012, .F. ) ;
#17534 = CYLINDRICAL_SURFACE ( 'NONE', #655, 31.99999999999999289 ) ;
#17535 = DIRECTION ( 'NONE',  ( 0.000000000000000000, 0.000000000000000000, -1.000000000000000000 ) ) ;
#17537 = FACE_OUTER_BOUND ( 'NONE', #10294, .T. ) ;
#17536 = AXIS2_PLACEMENT_3D ( 'NONE', #28394, #9794, #20090 ) ;
#17538 = ORIENTED_EDGE ( 'NONE', *, *, #37952, .T. ) ;
#17539 = ORIENTED_EDGE ( 'NONE', *, *, #3755, .T. ) ;
#17540 = VERTEX_POINT ( 'NONE', #1240 ) ;
#17541 = CARTESIAN_POINT ( 'NONE',  ( 10.00000000000000000, 16.23288003029543347, -33.80338159004267595 ) ) ;
#17542 = AXIS2_PLACEMENT_3D ( 'NONE', #11879, #22885, #45173 ) ;
#17543 = CARTESIAN_POINT ( 'NONE',  ( 0.000000000000000000, 0.000000000000000000, 0.000000000000000000 ) ) ;
#17544 = AXIS2_PLACEMENT_3D ( 'NONE', #46353, #20395, #17203 ) ;
#17545 = FACE_BOUND ( 'NONE', #48162, .T. ) ;
#17546 = LINE ( 'NONE', #33208, #37815 ) ;
#17547 = DIRECTION ( 'NONE',  ( 0.000000000000000000, 0.000000000000000000, -1.000000000000000000 ) ) ;
#17548 = EDGE_CURVE ( 'NONE', #42392, #46674, #118, .T. ) ;
#17549 = CARTESIAN_POINT ( 'NONE',  ( 0.000000000000000000, -65.58780272294048075, -36.73666225445966660 ) ) ;
#17550 = CARTESIAN_POINT ( 'NONE',  ( -1.499592026101402853, -119.9650177866181764, -2.500000000000000000 ) ) ;
#17551 = EDGE_CURVE ( 'NONE', #47247, #20870, #21986, .T. ) ;
#17552 = VECTOR ( 'NONE', #17527, 1000.000000000000000 ) ;
#17553 = AXIS2_PLACEMENT_3D ( 'NONE', #36472, #37198, #7334 ) ;
#17554 = VERTEX_POINT ( 'NONE', #9062 ) ;
#17555 = CIRCLE ( 'NONE', #23010, 82.00000000000000000 ) ;
#17556 = DIRECTION ( 'NONE',  ( 0.000000000000000000, 0.000000000000000000, 1.000000000000000000 ) ) ;
#17557 = ORIENTED_EDGE ( 'NONE', *, *, #29455, .F. ) ;
#17558 = ADVANCED_FACE ( 'NONE', ( #1717 ), #23997, .T. ) ;
#17559 = CYLINDRICAL_SURFACE ( 'NONE', #43375, 42.00000000000000000 ) ;
#17560 = DIRECTION ( 'NONE',  ( -1.000000000000000000, -0.000000000000000000, 0.000000000000000000 ) ) ;
#17561 = CARTESIAN_POINT ( 'NONE',  ( 12.49999999999999822, -120.0000000000000000, -125.0000000000000000 ) ) ;
#17562 = DIRECTION ( 'NONE',  ( 0.000000000000000000, 0.000000000000000000, 1.000000000000000000 ) ) ;
#17563 = EDGE_CURVE ( 'NONE', #15597, #10015, #13413, .T. ) ;
#17564 = CIRCLE ( 'NONE', #32426, 31.99999999999998934 ) ;
#17565 = DIRECTION ( 'NONE',  ( -1.000000000000000000, 0.000000000000000000, 0.000000000000000000 ) ) ;
#17566 = CARTESIAN_POINT ( 'NONE',  ( 11.99999999999999822, -75.11764819372145041, -2.946379043147127064 ) ) ;
#17567 = CARTESIAN_POINT ( 'NONE',  ( 0.000000000000000000, 0.000000000000000000, 0.000000000000000000 ) ) ;
#17568 = DIRECTION ( 'NONE',  ( 1.000000000000000000, 0.000000000000000000, 0.000000000000000000 ) ) ;
#17569 = CARTESIAN_POINT ( 'NONE',  ( 10.00000000000000000, -2.956366410620109519, -75.11725578898472122 ) ) ;
#17570 = APPLICATION_CONTEXT ( 'automotive_design' ) ;
#17571 = DIRECTION ( 'NONE',  ( 0.000000000000000000, 0.000000000000000000, -1.000000000000000000 ) ) ;
#17572 = EDGE_CURVE ( 'NONE', #17403, #31111, #32181, .T. ) ;
#17573 = ADVANCED_FACE ( 'NONE', ( #35486 ), #1972, .T. ) ;
#17574 = VERTEX_POINT ( 'NONE', #35000 ) ;
#17575 = ORIENTED_EDGE ( 'NONE', *, *, #31573, .F. ) ;
#17576 = VECTOR ( 'NONE', #28335, 1000.000000000000114 ) ;
#17577 = CIRCLE ( 'NONE', #30104, 77.49900000000000944 ) ;
#17578 = ORIENTED_EDGE ( 'NONE', *, *, #1441, .F. ) ;
#17579 = CARTESIAN_POINT ( 'NONE',  ( 0.000000000000000000, 81.96053171279902472, -2.543863470248677316 ) ) ;
#17580 = DIRECTION ( 'NONE',  ( -1.000000000000000000, 0.000000000000000000, -0.000000000000000000 ) ) ;
#17581 = VERTEX_POINT ( 'NONE', #38932 ) ;
#17582 = EDGE_CURVE ( 'NONE', #29949, #15931, #20415, .T. ) ;
#17583 = AXIS2_PLACEMENT_3D ( 'NONE', #18182, #25770, #40709 ) ;
#17584 = AXIS2_PLACEMENT_3D ( 'NONE', #20712, #2340, #2574 ) ;
#17585 = DIRECTION ( 'NONE',  ( -1.000000000000000000, 0.000000000000000000, -0.000000000000000000 ) ) ;
#17586 = ORIENTED_EDGE ( 'NONE', *, *, #41664, .T. ) ;
#17587 = ORIENTED_EDGE ( 'NONE', *, *, #5885, .F. ) ;
#17588 = AXIS2_PLACEMENT_3D ( 'NONE', #12166, #46656, #34898 ) ;
#17589 = EDGE_LOOP ( 'NONE', ( #29382, #22040, #8559, #25460 ) ) ;
#17590 = AXIS2_PLACEMENT_3D ( 'NONE', #46880, #2316, #13580 ) ;
#17591 = CARTESIAN_POINT ( 'NONE',  ( -4.250000000000000000, -13.95926121303099343, 0.000000000000000000 ) ) ;
#17592 = VERTEX_POINT ( 'NONE', #46758 ) ;
#17593 = CARTESIAN_POINT ( 'NONE',  ( 10.00000000000000000, -81.34940948281344220, 10.30890764327356557 ) ) ;
#17594 = EDGE_LOOP ( 'NONE', ( #14186, #18180, #44096, #29101 ) ) ;
#17595 = CARTESIAN_POINT ( 'NONE',  ( 5.999999999999999112, 55.16347631943131802, -60.67117009219074930 ) ) ;
#17596 = CIRCLE ( 'NONE', #22298, 77.49899999999999523 ) ;
#17597 = CARTESIAN_POINT ( 'NONE',  ( 10.00000000000000000, 0.000000000000000000, 0.000000000000000000 ) ) ;
#17598 = LINE ( 'NONE', #21265, #20474 ) ;
#17599 = VERTEX_POINT ( 'NONE', #8801 ) ;
#17600 = LINE ( 'NONE', #32544, #25888 ) ;
#17601 = ORIENTED_EDGE ( 'NONE', *, *, #32927, .F. ) ;
#17602 = ADVANCED_FACE ( 'NONE', ( #46028 ), #9525, .F. ) ;
#17603 = CARTESIAN_POINT ( 'NONE',  ( 11.99999999999999822, 68.27212725128275395, 31.46837873495001503 ) ) ;
#17604 = AXIS2_PLACEMENT_3D ( 'NONE', #48269, #14747, #47540 ) ;
#17605 = DIRECTION ( 'NONE',  ( 0.000000000000000000, 0.000000000000000000, 1.000000000000000000 ) ) ;
#17606 = EDGE_CURVE ( 'NONE', #4059, #45971, #20801, .T. ) ;
#17607 = VERTEX_POINT ( 'NONE', #28375 ) ;
#17608 = ORIENTED_EDGE ( 'NONE', *, *, #11570, .T. ) ;
#17609 = DIRECTION ( 'NONE',  ( 1.000000000000000000, 0.000000000000000000, 0.000000000000000000 ) ) ;
#17610 = CARTESIAN_POINT ( 'NONE',  ( -3.000000000000000000, -10.45096189432344147, 21.10159698893426494 ) ) ;
#17611 = ORIENTED_EDGE ( 'NONE', *, *, #16976, .T. ) ;
#17612 = VERTEX_POINT ( 'NONE', #24716 ) ;
#17613 = ADVANCED_FACE ( 'NONE', ( #1478 ), #20073, .T. ) ;
#17614 = PLANE ( 'NONE',  #25359 ) ;
#17615 = CYLINDRICAL_SURFACE ( 'NONE', #11805, 16.00000000000000000 ) ;
#17616 = CARTESIAN_POINT ( 'NONE',  ( 15.00000000000000000, 23.59884966291538078, 12.14883922797231008 ) ) ;
#17617 = CARTESIAN_POINT ( 'NONE',  ( 10.00000000000000000, -10.74501242461308159, 35.92658777277507909 ) ) ;
#17618 = EDGE_CURVE ( 'NONE', #13751, #34159, #20299, .T. ) ;
#17619 = CYLINDRICAL_SURFACE ( 'NONE', #26307, 16.00000000000000000 ) ;
#17620 = CIRCLE ( 'NONE', #34040, 42.00000000000000000 ) ;
#17621 = VECTOR ( 'NONE', #44152, 1000.000000000000000 ) ;
#17622 = DIRECTION ( 'NONE',  ( 0.000000000000000000, 0.3090169943749482839, -0.9510565162951533091 ) ) ;
#17623 = DIRECTION ( 'NONE',  ( -1.000000000000000000, -0.000000000000000000, -0.000000000000000000 ) ) ;
#17624 = VECTOR ( 'NONE', #11127, 1000.000000000000000 ) ;
#17625 = LINE ( 'NONE', #28879, #11963 ) ;
#17626 = CARTESIAN_POINT ( 'NONE',  ( 10.00000000000000000, 74.18225833017889670, 34.94270380257666631 ) ) ;
#17627 = LINE ( 'NONE', #21292, #26439 ) ;
#17628 = CIRCLE ( 'NONE', #15310, 37.49900000000000944 ) ;
#17629 = CARTESIAN_POINT ( 'NONE',  ( 0.000000000000000000, -0.8299999999999999600, -1.199999999999999956 ) ) ;
#17630 = AXIS2_PLACEMENT_3D ( 'NONE', #5161, #20075, #20300 ) ;
#17631 = ORIENTED_EDGE ( 'NONE', *, *, #32488, .F. ) ;
#17632 = EDGE_CURVE ( 'NONE', #3822, #12857, #47024, .T. ) ;
#17633 = EDGE_CURVE ( 'NONE', #8125, #9625, #25902, .T. ) ;
#17634 = ORIENTED_EDGE ( 'NONE', *, *, #17692, .T. ) ;
#17635 = EDGE_CURVE ( 'NONE', #23818, #41796, #40803, .T. ) ;
#17636 = LINE ( 'NONE', #10289, #28406 ) ;
#17637 = ORIENTED_EDGE ( 'NONE', *, *, #37577, .T. ) ;
#17638 = AXIS2_PLACEMENT_3D ( 'NONE', #8772, #23712, #5127 ) ;
#17639 = AXIS2_PLACEMENT_3D ( 'NONE', #12323, #16465, #38758 ) ;
#17640 = CARTESIAN_POINT ( 'NONE',  ( 11.99999999999999822, 59.46389618801966037, 49.70050353004911159 ) ) ;
#17641 = ORIENTED_EDGE ( 'NONE', *, *, #42083, .F. ) ;
#17642 = EDGE_CURVE ( 'NONE', #38166, #28952, #38464, .T. ) ;
#17643 = AXIS2_PLACEMENT_3D ( 'NONE', #21051, #9802, #20099 ) ;
#17644 = ORIENTED_EDGE ( 'NONE', *, *, #36480, .T. ) ;
#17645 = DIRECTION ( 'NONE',  ( -1.000000000000000000, 0.000000000000000000, 0.000000000000000000 ) ) ;
#17646 = ORIENTED_EDGE ( 'NONE', *, *, #10643, .T. ) ;
#17647 = DIRECTION ( 'NONE',  ( 0.000000000000000000, 0.000000000000000000, 1.000000000000000000 ) ) ;
#17648 = ORIENTED_EDGE ( 'NONE', *, *, #17563, .T. ) ;
#17649 = CARTESIAN_POINT ( 'NONE',  ( -14.87942725330654348, -141.9795960975983178, -5.500000000000000000 ) ) ;
#17650 = CIRCLE ( 'NONE', #45025, 77.49900000000000944 ) ;
#17651 = CARTESIAN_POINT ( 'NONE',  ( 10.00000000000000000, 0.000000000000000000, 0.000000000000000000 ) ) ;
#17652 = CARTESIAN_POINT ( 'NONE',  ( 11.99999999999999822, 69.42325613327489009, -34.44570377933524696 ) ) ;
#17653 = ORIENTED_EDGE ( 'NONE', *, *, #34982, .F. ) ;
#17654 = DIRECTION ( 'NONE',  ( -1.000000000000000000, 0.000000000000000000, 0.000000000000000000 ) ) ;
#17655 = ORIENTED_EDGE ( 'NONE', *, *, #28235, .T. ) ;
#17656 = CIRCLE ( 'NONE', #41934, 37.49900000000000944 ) ;
#17657 = CARTESIAN_POINT ( 'NONE',  ( 11.99999999999999822, 40.65526001592713357, -71.21200624218752750 ) ) ;
#17658 = EDGE_LOOP ( 'NONE', ( #37267, #20679, #19666, #47617 ) ) ;
#17659 = DIRECTION ( 'NONE',  ( 0.000000000000000000, 0.000000000000000000, 1.000000000000000000 ) ) ;
#17660 = AXIS2_PLACEMENT_3D ( 'NONE', #3462, #10819, #11056 ) ;
#17661 = DIRECTION ( 'NONE',  ( 0.000000000000000000, -0.2079116908177532363, 0.9781476007338069101 ) ) ;
#17662 = FACE_OUTER_BOUND ( 'NONE', #23970, .T. ) ;
#17664 = ORIENTED_EDGE ( 'NONE', *, *, #2125, .T. ) ;
#17663 = LINE ( 'NONE', #32596, #32079 ) ;
#17665 = CYLINDRICAL_SURFACE ( 'NONE', #41089, 82.00000000000000000 ) ;
#17666 = EDGE_LOOP ( 'NONE', ( #33980, #13218, #19856, #11600 ) ) ;
#17667 = CIRCLE ( 'NONE', #490, 16.00000000000000000 ) ;
#17668 = CARTESIAN_POINT ( 'NONE',  ( -12.40464318976452596, 10.41032311384371489, 52.00000000000002132 ) ) ;
#17669 = ORIENTED_EDGE ( 'NONE', *, *, #3035, .T. ) ;
#17670 = ORIENTED_EDGE ( 'NONE', *, *, #26627, .F. ) ;
#17671 = CARTESIAN_POINT ( 'NONE',  ( 10.00000000000000000, -36.73666225445845157, -65.58780272294114866 ) ) ;
#17672 = CYLINDRICAL_SURFACE ( 'NONE', #26274, 16.00000000000000000 ) ;
#17673 = ORIENTED_EDGE ( 'NONE', *, *, #23446, .T. ) ;
#17674 = EDGE_CURVE ( 'NONE', #24885, #40287, #20491, .T. ) ;
#17675 = DIRECTION ( 'NONE',  ( -0.000000000000000000, -0.000000000000000000, -1.000000000000000000 ) ) ;
#17676 = CARTESIAN_POINT ( 'NONE',  ( 11.99999999999999822, 74.65374052328648702, 8.840884882375350529 ) ) ;
#17677 = CARTESIAN_POINT ( 'NONE',  ( 10.00000000000000000, -35.47612816024539484, 22.48208911017487921 ) ) ;
#17678 = ORIENTED_EDGE ( 'NONE', *, *, #27524, .T. ) ;
#17679 = CARTESIAN_POINT ( 'NONE',  ( 11.99999999999999822, -50.95692526931372157, 58.39081064771733054 ) ) ;
#17680 = CIRCLE ( 'NONE', #7552, 35.50000000000000711 ) ;
#17681 = EDGE_CURVE ( 'NONE', #5353, #14154, #24942, .T. ) ;
#17682 = DIRECTION ( 'NONE',  ( -1.000000000000000000, 0.000000000000000000, 0.000000000000000000 ) ) ;
#17683 = EDGE_CURVE ( 'NONE', #34659, #24069, #25418, .T. ) ;
#17684 = DIRECTION ( 'NONE',  ( 0.000000000000000000, 0.9510565162951544194, -0.3090169943749447867 ) ) ;
#17685 = VECTOR ( 'NONE', #45029, 1000.000000000000000 ) ;
#17686 = EDGE_CURVE ( 'NONE', #33006, #2837, #47460, .T. ) ;
#17687 = CARTESIAN_POINT ( 'NONE',  ( 10.00000000000000000, 0.8828120875900632436, 37.48860685352291000 ) ) ;
#17688 = ORIENTED_EDGE ( 'NONE', *, *, #2453, .F. ) ;
#17689 = EDGE_CURVE ( 'NONE', #24295, #34363, #10016, .T. ) ;
#17690 = CARTESIAN_POINT ( 'NONE',  ( 0.000000000000000000, -10.96151621346514382, 35.95386929396252640 ) ) ;
#17692 = EDGE_CURVE ( 'NONE', #5492, #897, #14173, .T. ) ;
#17691 = CARTESIAN_POINT ( 'NONE',  ( 11.99999999999999822, 62.20884554314020676, 46.21855187248652896 ) ) ;
#17693 = CYLINDRICAL_SURFACE ( 'NONE', #31886, 77.49899999999999523 ) ;
#17694 = CARTESIAN_POINT ( 'NONE',  ( 0.000000000000000000, -63.18004540533059554, 44.88180994100355292 ) ) ;
#17695 = LINE ( 'NONE', #28229, #1757 ) ;
#17696 = DIRECTION ( 'NONE',  ( -1.000000000000000000, 0.000000000000000000, 0.000000000000000000 ) ) ;
#17697 = ORIENTED_EDGE ( 'NONE', *, *, #26310, .T. ) ;
#17698 = AXIS2_PLACEMENT_3D ( 'NONE', #1655, #23204, #8999 ) ;
#17699 = DIRECTION ( 'NONE',  ( -1.000000000000000000, 0.000000000000000000, 0.000000000000000000 ) ) ;
#17700 = ORIENTED_EDGE ( 'NONE', *, *, #24858, .F. ) ;
#17701 = EDGE_CURVE ( 'NONE', #2295, #32513, #6833, .T. ) ;
#17702 = DIRECTION ( 'NONE',  ( 0.000000000000000000, 0.000000000000000000, 1.000000000000000000 ) ) ;
#17703 = VECTOR ( 'NONE', #28162, 1000.000000000000000 ) ;
#17704 = DIRECTION ( 'NONE',  ( 0.000000000000000000, -0.3090169943749460635, -0.9510565162951539753 ) ) ;
#17705 = VERTEX_POINT ( 'NONE', #3377 ) ;
#17706 = EDGE_CURVE ( 'NONE', #44567, #7073, #47682, .T. ) ;
#17707 = VECTOR ( 'NONE', #15636, 1000.000000000000000 ) ;
#17708 = CARTESIAN_POINT ( 'NONE',  ( 0.000000000000000000, 0.000000000000000000, 0.000000000000000000 ) ) ;
#17709 = ORIENTED_EDGE ( 'NONE', *, *, #10789, .F. ) ;
#17710 = VECTOR ( 'NONE', #3847, 1000.000000000000000 ) ;
#17711 = AXIS2_PLACEMENT_3D ( 'NONE', #17567, #47436, #43758 ) ;
#17712 = EDGE_CURVE ( 'NONE', #39648, #18873, #40042, .T. ) ;
#17713 = DIRECTION ( 'NONE',  ( -1.000000000000000000, 0.000000000000000000, 0.000000000000000000 ) ) ;
#17714 = EDGE_LOOP ( 'NONE', ( #44641, #25966, #47871, #46033 ) ) ;
#17715 = CARTESIAN_POINT ( 'NONE',  ( 10.00000000000000000, 37.48860685352291000, 0.8828120875901893649 ) ) ;
#17716 = CARTESIAN_POINT ( 'NONE',  ( 0.000000000000000000, 23.59884966291538078, -12.14883922797231541 ) ) ;
#17717 = EDGE_LOOP ( 'NONE', ( #23301, #3414, #31840, #6847, #1547, #34435, #7452, #5316, #5776, #21602, #14107, #32789, #35955, #44448, #7037, #28917 ) ) ;
#17718 = CARTESIAN_POINT ( 'NONE',  ( 0.000000000000000000, 81.90746397400387480, 3.894527615418180044 ) ) ;
#17719 = VERTEX_POINT ( 'NONE', #21748 ) ;
#17720 = DIRECTION ( 'NONE',  ( 0.000000000000000000, -0.8910065241883722287, 0.4539904997395382558 ) ) ;
#17721 = DIRECTION ( 'NONE',  ( 0.000000000000000000, -0.5877852522924691403, 0.8090169943749504489 ) ) ;
#17722 = DIRECTION ( 'NONE',  ( 0.000000000000000000, -0.1564344650402172410, -0.9876883405951399908 ) ) ;
#17723 = ADVANCED_FACE ( 'NONE', ( #47927 ), #17346, .T. ) ;
#17724 = AXIS2_PLACEMENT_3D ( 'NONE', #48129, #29531, #30014 ) ;
#17725 = VERTEX_POINT ( 'NONE', #18321 ) ;
#17726 = CARTESIAN_POINT ( 'NONE',  ( 10.00000000000000000, -40.98264845739755913, 9.188173127307164734 ) ) ;
#17727 = EDGE_LOOP ( 'NONE', ( #15665, #32609, #42876, #6754, #30564, #38928, #35149, #34665 ) ) ;
#17728 = VERTEX_POINT ( 'NONE', #18068 ) ;
#17729 = EDGE_CURVE ( 'NONE', #33736, #24721, #7057, .T. ) ;
#17730 = DIRECTION ( 'NONE',  ( 1.000000000000000000, 0.000000000000000000, 0.000000000000000000 ) ) ;
#17731 = CIRCLE ( 'NONE', #21650, 77.49899999999999523 ) ;
#17732 = DIRECTION ( 'NONE',  ( 0.000000000000000000, -0.5877852522924802425, 0.8090169943749422332 ) ) ;
#17733 = DIRECTION ( 'NONE',  ( 0.000000000000000000, 0.9876883405951383255, -0.1564344650402277048 ) ) ;
#17734 = DIRECTION ( 'NONE',  ( -1.000000000000000000, -0.000000000000000000, -0.000000000000000000 ) ) ;
#17735 = ORIENTED_EDGE ( 'NONE', *, *, #22285, .T. ) ;
#17736 = EDGE_CURVE ( 'NONE', #11877, #14823, #40595, .T. ) ;
#17737 = DIRECTION ( 'NONE',  ( 0.000000000000000000, 0.000000000000000000, 1.000000000000000000 ) ) ;
#17738 = LINE ( 'NONE', #46401, #35488 ) ;
#17739 = EDGE_CURVE ( 'NONE', #16528, #39957, #21522, .T. ) ;
#17740 = CARTESIAN_POINT ( 'NONE',  ( 0.000000000000000000, -15.48615015657610527, 39.04073710021338428 ) ) ;
#17741 = DIRECTION ( 'NONE',  ( -1.000000000000000000, 0.000000000000000000, -0.000000000000000000 ) ) ;
#17742 = FACE_OUTER_BOUND ( 'NONE', #35494, .T. ) ;
#17743 = DIRECTION ( 'NONE',  ( 0.000000000000000000, -0.6494480483301903195, 0.7604059656000251577 ) ) ;
#17744 = ORIENTED_EDGE ( 'NONE', *, *, #34142, .T. ) ;
#17745 = AXIS2_PLACEMENT_3D ( 'NONE', #13794, #13536, #3226 ) ;
#17746 = EDGE_LOOP ( 'NONE', ( #30413, #43906, #18019, #11588 ) ) ;
#17748 = EDGE_CURVE ( 'NONE', #2363, #20770, #7180, .T. ) ;
#17747 = FACE_OUTER_BOUND ( 'NONE', #6362, .T. ) ;
#17749 = FACE_OUTER_BOUND ( 'NONE', #16109, .T. ) ;
#17750 = DIRECTION ( 'NONE',  ( -1.000000000000000000, 0.000000000000000000, -0.000000000000000000 ) ) ;
#17751 = DIRECTION ( 'NONE',  ( 0.000000000000000000, 0.4539904997395478037, -0.8910065241883673437 ) ) ;
#17752 = LINE ( 'NONE', #32677, #38100 ) ;
#17753 = CARTESIAN_POINT ( 'NONE',  ( 0.000000000000000000, -33.00180498840035170, -17.80606268964575278 ) ) ;
#17754 = ORIENTED_EDGE ( 'NONE', *, *, #20283, .T. ) ;
#17755 = DIRECTION ( 'NONE',  ( 0.000000000000000000, 0.3090169943749411785, 0.9510565162951556406 ) ) ;
#17756 = DIRECTION ( 'NONE',  ( -1.000000000000000000, -0.000000000000000000, 0.000000000000000000 ) ) ;
#17757 = ORIENTED_EDGE ( 'NONE', *, *, #23951, .T. ) ;
#17758 = VERTEX_POINT ( 'NONE', #29582 ) ;
#17759 = AXIS2_PLACEMENT_3D ( 'NONE', #40726, #14787, #26031 ) ;
#17760 = ORIENTED_EDGE ( 'NONE', *, *, #25070, .F. ) ;
#17761 = ORIENTED_EDGE ( 'NONE', *, *, #22083, .F. ) ;
#17762 = AXIS2_PLACEMENT_3D ( 'NONE', #44246, #37381, #6804 ) ;
#17763 = CARTESIAN_POINT ( 'NONE',  ( 0.000000000000000000, 66.50666863322000211, 39.78640506895628448 ) ) ;
#17764 = ORIENTED_EDGE ( 'NONE', *, *, #22880, .F. ) ;
#17765 = VERTEX_POINT ( 'NONE', #47227 ) ;
#17766 = CARTESIAN_POINT ( 'NONE',  ( 5.000000000000000000, 40.65526001592713357, -71.21200624218752750 ) ) ;
#17767 = LINE ( 'NONE', #25591, #21068 ) ;
#17768 = CARTESIAN_POINT ( 'NONE',  ( 10.00000000000000000, 29.01471420065564644, 76.69515212746024702 ) ) ;
#17769 = EDGE_LOOP ( 'NONE', ( #35719, #22019, #41380, #22120 ) ) ;
#17770 = CARTESIAN_POINT ( 'NONE',  ( 10.00000000000000000, 68.67312586194995561, 35.91791733033500122 ) ) ;
#17771 = VERTEX_POINT ( 'NONE', #36197 ) ;
#17772 = ORIENTED_EDGE ( 'NONE', *, *, #38867, .F. ) ;
#17773 = ORIENTED_EDGE ( 'NONE', *, *, #1767, .F. ) ;
#17774 = CARTESIAN_POINT ( 'NONE',  ( 10.00000000000000000, 0.000000000000000000, 0.000000000000000000 ) ) ;
#17775 = CARTESIAN_POINT ( 'NONE',  ( 0.000000000000000000, 78.73519480814955784, 22.90783923731657268 ) ) ;
#17776 = CIRCLE ( 'NONE', #31892, 31.99999999999998934 ) ;
#17777 = CARTESIAN_POINT ( 'NONE',  ( 0.000000000000000000, 44.88180994100468268, -63.18004540532978552 ) ) ;
#17778 = ORIENTED_EDGE ( 'NONE', *, *, #5539, .T. ) ;
#17779 = VERTEX_POINT ( 'NONE', #44509 ) ;
#17780 = EDGE_LOOP ( 'NONE', ( #29348, #8957, #35898, #44177 ) ) ;
#17781 = DIRECTION ( 'NONE',  ( 0.000000000000000000, 0.000000000000000000, 1.000000000000000000 ) ) ;
#17782 = ORIENTED_EDGE ( 'NONE', *, *, #9387, .T. ) ;
#17783 = ADVANCED_FACE ( 'NONE', ( #32538 ), #10981, .T. ) ;
#17784 = CARTESIAN_POINT ( 'NONE',  ( 0.000000000000000000, 76.66974797899852945, -11.30684508768257679 ) ) ;
#17785 = LINE ( 'NONE', #32953, #7657 ) ;
#17786 = CARTESIAN_POINT ( 'NONE',  ( 0.000000000000000000, 0.000000000000000000, 0.000000000000000000 ) ) ;
#17787 = ORIENTED_EDGE ( 'NONE', *, *, #31954, .T. ) ;
#17788 = CARTESIAN_POINT ( 'NONE',  ( 11.99999999999999822, 72.35432306680485226, -20.40083707022909110 ) ) ;
#17789 = EDGE_CURVE ( 'NONE', #40588, #17873, #27528, .T. ) ;
#17790 = CARTESIAN_POINT ( 'NONE',  ( -26.53422223201112828, -120.6595836127786043, 5.500000000000000000 ) ) ;
#17792 = ADVANCED_FACE ( 'NONE', ( #33491 ), #7301, .F. ) ;
#17791 = DIRECTION ( 'NONE',  ( -1.000000000000000000, 0.000000000000000000, -0.000000000000000000 ) ) ;
#17793 = LINE ( 'NONE', #20501, #2456 ) ;
#17794 = AXIS2_PLACEMENT_3D ( 'NONE', #13999, #32600, #22054 ) ;
#17795 = ORIENTED_EDGE ( 'NONE', *, *, #23652, .F. ) ;
#17797 = ADVANCED_FACE ( 'NONE', ( #48417 ), #19038, .T. ) ;
#17796 = DIRECTION ( 'NONE',  ( 0.3853207896976533209, -0.9227826878668545785, 0.000000000000000000 ) ) ;
#17798 = ORIENTED_EDGE ( 'NONE', *, *, #10609, .F. ) ;
#17799 = VECTOR ( 'NONE', #9096, 1000.000000000000000 ) ;
#17800 = AXIS2_PLACEMENT_3D ( 'NONE', #41812, #19031, #41328 ) ;
#17801 = CARTESIAN_POINT ( 'NONE',  ( 10.00000000000000000, 0.000000000000000000, 0.000000000000000000 ) ) ;
#17802 = EDGE_CURVE ( 'NONE', #28317, #45238, #18793, .T. ) ;
#17803 = CARTESIAN_POINT ( 'NONE',  ( 2.500000000000000000, 16.00000000000000000, 0.000000000000000000 ) ) ;
#17804 = DIRECTION ( 'NONE',  ( 0.000000000000000000, 0.000000000000000000, 1.000000000000000000 ) ) ;
#17805 = CARTESIAN_POINT ( 'NONE',  ( -24.50849501662245444, -109.8101191361138831, 2.500000000000000000 ) ) ;
#17806 = CARTESIAN_POINT ( 'NONE',  ( 2.047646702416564768, -96.54137380445985173, 5.500000000000000000 ) ) ;
#17807 = CARTESIAN_POINT ( 'NONE',  ( 11.99999999999999822, 49.70050353004975818, -59.46389618801909904 ) ) ;
#17808 = CARTESIAN_POINT ( 'NONE',  ( 16.84844760790522855, -103.5491698323862124, 5.500000000000000000 ) ) ;
#17809 = DIRECTION ( 'NONE',  ( -1.000000000000000000, -0.000000000000000000, -0.000000000000000000 ) ) ;
#17810 = LINE ( 'NONE', #18294, #28443 ) ;
#17811 = MECHANICAL_DESIGN_GEOMETRIC_PRESENTATION_REPRESENTATION (  '', ( #14013 ), #30340 ) ;
#17812 = VERTEX_POINT ( 'NONE', #26640 ) ;
#17813 = ORIENTED_EDGE ( 'NONE', *, *, #20064, .F. ) ;
#17814 = VERTEX_POINT ( 'NONE', #37653 ) ;
#17815 = FACE_OUTER_BOUND ( 'NONE', #9706, .T. ) ;
#17816 = PLANE ( 'NONE',  #37872 ) ;
#17817 = VERTEX_POINT ( 'NONE', #23207 ) ;
#17818 = AXIS2_PLACEMENT_3D ( 'NONE', #47642, #16654, #38445 ) ;
#17819 = EDGE_CURVE ( 'NONE', #15509, #8725, #3258, .T. ) ;
#17820 = LINE ( 'NONE', #39872, #35092 ) ;
#17821 = ADVANCED_FACE ( 'NONE', ( #4383 ), #14897, .T. ) ;
#17822 =( GEOMETRIC_REPRESENTATION_CONTEXT ( 3 ) GLOBAL_UNCERTAINTY_ASSIGNED_CONTEXT ( ( #22749 ) ) GLOBAL_UNIT_ASSIGNED_CONTEXT ( ( #5662, #24496, #17146 ) ) REPRESENTATION_CONTEXT ( 'NONE', 'WORKASPACE' ) );
#17823 = ORIENTED_EDGE ( 'NONE', *, *, #23938, .T. ) ;
#17824 = VERTEX_POINT ( 'NONE', #7788 ) ;
#17825 = ORIENTED_EDGE ( 'NONE', *, *, #20163, .T. ) ;
#17826 = VECTOR ( 'NONE', #4546, 1000.000000000000000 ) ;
#17827 = ADVANCED_FACE ( 'NONE', ( #45473 ), #11957, .T. ) ;
#17828 = DIRECTION ( 'NONE',  ( 0.000000000000000000, 0.000000000000000000, 1.000000000000000000 ) ) ;
#17829 = ORIENTED_EDGE ( 'NONE', *, *, #29319, .T. ) ;
#17830 = CARTESIAN_POINT ( 'NONE',  ( -3.000000000000000000, -13.04903810567647682, -19.60159698893442481 ) ) ;
#17831 = ORIENTED_EDGE ( 'NONE', *, *, #3190, .T. ) ;
#17832 = DIRECTION ( 'NONE',  ( -1.000000000000000000, 0.000000000000000000, 0.000000000000000000 ) ) ;
#17833 = DIRECTION ( 'NONE',  ( -1.000000000000000000, 0.000000000000000000, 0.000000000000000000 ) ) ;
#17834 = PRODUCT_DEFINITION_FORMATION_WITH_SPECIFIED_SOURCE ( 'ANY', '', #42918, .NOT_KNOWN. ) ;
#17835 = EDGE_CURVE ( 'NONE', #675, #40605, #3638, .T. ) ;
#17836 = CARTESIAN_POINT ( 'NONE',  ( 10.00000000000000000, 30.00120703465236716, -22.64427369931138756 ) ) ;
#17837 = ORIENTED_EDGE ( 'NONE', *, *, #26188, .F. ) ;
#17838 = EDGE_CURVE ( 'NONE', #20905, #8546, #4606, .T. ) ;
#17839 = CARTESIAN_POINT ( 'NONE',  ( 0.000000000000000000, -58.39081064771713869, -50.95692526931392052 ) ) ;
#17840 = ADVANCED_FACE ( 'NONE', ( #454 ), #15865, .T. ) ;
#17841 = ORIENTED_EDGE ( 'NONE', *, *, #22080, .T. ) ;
#17842 = VECTOR ( 'NONE', #37011, 1000.000000000000000 ) ;
#17843 = LINE ( 'NONE', #14179, #35972 ) ;
#17844 = DIRECTION ( 'NONE',  ( 1.000000000000000000, 0.000000000000000000, 0.000000000000000000 ) ) ;
#17845 = VERTEX_POINT ( 'NONE', #45241 ) ;
#17846 = ORIENTED_EDGE ( 'NONE', *, *, #45335, .T. ) ;
#17847 = DIRECTION ( 'NONE',  ( 0.000000000000000000, 0.000000000000000000, 1.000000000000000000 ) ) ;
#17848 = CARTESIAN_POINT ( 'NONE',  ( -3.000000000000000000, -11.95096189432345390, 23.69967320028757385 ) ) ;
#17849 = ORIENTED_EDGE ( 'NONE', *, *, #15905, .F. ) ;
#17850 = VERTEX_POINT ( 'NONE', #29820 ) ;
#17851 = CYLINDRICAL_SURFACE ( 'NONE', #5819, 31.99999999999998579 ) ;
#17852 = DIRECTION ( 'NONE',  ( 1.000000000000000000, 0.000000000000000000, 0.000000000000000000 ) ) ;
#17853 = DIRECTION ( 'NONE',  ( -1.000000000000000000, -0.000000000000000000, -0.000000000000000000 ) ) ;
#17854 = CARTESIAN_POINT ( 'NONE',  ( 10.00000000000000000, 0.000000000000000000, 0.000000000000000000 ) ) ;
#17855 = EDGE_CURVE ( 'NONE', #43648, #11145, #22837, .T. ) ;
#17856 = CARTESIAN_POINT ( 'NONE',  ( -3.000000000000000000, 23.50000000000000000, -1.500000000000001332 ) ) ;
#17857 = CARTESIAN_POINT ( 'NONE',  ( 0.000000000000000000, -56.15606465355001120, 59.75363087400055662 ) ) ;
#17858 = CARTESIAN_POINT ( 'NONE',  ( 0.000000000000000000, -79.10210256391383155, 21.60688246758558506 ) ) ;
#17859 = CIRCLE ( 'NONE', #22586, 37.49900000000000233 ) ;
#17860 = DIRECTION ( 'NONE',  ( 0.000000000000000000, 0.000000000000000000, 1.000000000000000000 ) ) ;
#17861 = AXIS2_PLACEMENT_3D ( 'NONE', #7020, #25620, #17556 ) ;
#17862 = DIRECTION ( 'NONE',  ( -1.000000000000000000, 0.000000000000000000, 0.000000000000000000 ) ) ;
#17863 = AXIS2_PLACEMENT_3D ( 'NONE', #46632, #27540, #28032 ) ;
#17864 = FACE_OUTER_BOUND ( 'NONE', #35948, .T. ) ;
#17865 = VERTEX_POINT ( 'NONE', #41103 ) ;
#17866 = ORIENTED_EDGE ( 'NONE', *, *, #9513, .T. ) ;
#17867 = ORIENTED_EDGE ( 'NONE', *, *, #30664, .F. ) ;
#17868 = UNCERTAINTY_MEASURE_WITH_UNIT (LENGTH_MEASURE( 1.000000000000000082E-05 ), #38906, 'distance_accuracy_value', 'NONE');
#17869 = DIRECTION ( 'NONE',  ( -1.000000000000000000, 0.000000000000000000, 0.000000000000000000 ) ) ;
#17870 = DIRECTION ( 'NONE',  ( -1.000000000000000000, -0.000000000000000000, -0.000000000000000000 ) ) ;
#17871 = ORIENTED_EDGE ( 'NONE', *, *, #16807, .F. ) ;
#17872 = STYLED_ITEM ( 'NONE', ( #29609 ), #38066 ) ;
#17873 = VERTEX_POINT ( 'NONE', #7560 ) ;
#17874 = ADVANCED_FACE ( 'NONE', ( #22248 ), #22489, .F. ) ;
#17875 = CARTESIAN_POINT ( 'NONE',  ( 10.00000000000000000, -22.48208911017474065, -35.47612816024548721 ) ) ;
#17876 = FACE_OUTER_BOUND ( 'NONE', #35484, .T. ) ;
#17877 = EDGE_CURVE ( 'NONE', #38831, #27191, #30078, .T. ) ;
#17878 = ORIENTED_EDGE ( 'NONE', *, *, #39758, .T. ) ;
#17879 = CARTESIAN_POINT ( 'NONE',  ( 11.99999999999999822, -77.32052557432837148, -5.256550761633681290 ) ) ;
#17880 = EDGE_CURVE ( 'NONE', #33388, #6346, #26406, .T. ) ;
#17881 = CARTESIAN_POINT ( 'NONE',  ( 11.99999999999999822, -68.27212725128254078, -31.46837873495049465 ) ) ;
#17882 = AXIS2_PLACEMENT_3D ( 'NONE', #47212, #7291, #44501 ) ;
#17883 = CARTESIAN_POINT ( 'NONE',  ( -23.97194136764370498, -131.3950000906648938, 5.500000000000000000 ) ) ;
#17884 = EDGE_LOOP ( 'NONE', ( #10596, #28845, #6844, #19741 ) ) ;
#17886 = EDGE_CURVE ( 'NONE', #897, #28171, #22960, .T. ) ;
#17885 = CARTESIAN_POINT ( 'NONE',  ( 6.719258119307965238, -15.35072898742050107, 0.000000000000000000 ) ) ;
#17887 = ORIENTED_EDGE ( 'NONE', *, *, #16160, .T. ) ;
#17888 = AXIS2_PLACEMENT_3D ( 'NONE', #11691, #4111, #4587 ) ;
#17889 = CIRCLE ( 'NONE', #45270, 82.00000000000000000 ) ;
#17890 = DIRECTION ( 'NONE',  ( -1.000000000000000000, -0.000000000000000000, 0.000000000000000000 ) ) ;
#17891 = ORIENTED_EDGE ( 'NONE', *, *, #2976, .T. ) ;
#17892 = CYLINDRICAL_SURFACE ( 'NONE', #14199, 77.49899999999999523 ) ;
#17893 = VERTEX_POINT ( 'NONE', #1658 ) ;
#17894 = EDGE_CURVE ( 'NONE', #37838, #5554, #24175, .T. ) ;
#17895 = LINE ( 'NONE', #13279, #29260 ) ;
#17896 = DIRECTION ( 'NONE',  ( 0.000000000000000000, 0.000000000000000000, -1.000000000000000000 ) ) ;
#17897 = ADVANCED_FACE ( 'NONE', ( #5827 ), #4848, .F. ) ;
#17899 = VERTEX_POINT ( 'NONE', #31536 ) ;
#17898 = DIRECTION ( 'NONE',  ( -1.000000000000000000, -0.000000000000000000, 0.000000000000000000 ) ) ;
#17900 = DIRECTION ( 'NONE',  ( -1.000000000000000000, -0.000000000000000000, -0.000000000000000000 ) ) ;
#17901 = ORIENTED_EDGE ( 'NONE', *, *, #30550, .T. ) ;
#17902 = FACE_OUTER_BOUND ( 'NONE', #46657, .T. ) ;
#17903 = ORIENTED_EDGE ( 'NONE', *, *, #13443, .F. ) ;
#17904 = ORIENTED_EDGE ( 'NONE', *, *, #44548, .F. ) ;
#17905 = DIRECTION ( 'NONE',  ( 0.000000000000000000, 0.000000000000000000, 1.000000000000000000 ) ) ;
#17906 = DIRECTION ( 'NONE',  ( 0.2306669878475637314, 0.9730327541852493711, 0.000000000000000000 ) ) ;
#17907 = CARTESIAN_POINT ( 'NONE',  ( -26.29030328629083968, -123.6496510949466341, -5.500000000000000000 ) ) ;
#17908 = DIRECTION ( 'NONE',  ( -1.000000000000000000, 0.000000000000000000, 0.000000000000000000 ) ) ;
#17909 = CARTESIAN_POINT ( 'NONE',  ( 0.000000000000000000, 0.000000000000000000, 0.000000000000000000 ) ) ;
#17910 = ORIENTED_EDGE ( 'NONE', *, *, #3136, .F. ) ;
#17911 = DIRECTION ( 'NONE',  ( 0.000000000000000000, 0.000000000000000000, -1.000000000000000000 ) ) ;
#17912 = CARTESIAN_POINT ( 'NONE',  ( 11.99999999999999822, -71.27951684758005513, -30.41916302227188851 ) ) ;
#17913 = EDGE_CURVE ( 'NONE', #28068, #26813, #28291, .T. ) ;
#17914 = CARTESIAN_POINT ( 'NONE',  ( 11.99999999999999822, 36.73666225445894185, 65.58780272294090707 ) ) ;
#17915 = LINE ( 'NONE', #3479, #44247 ) ;
#17916 = CARTESIAN_POINT ( 'NONE',  ( -26.41226275915097332, -122.1546173538626761, 2.500000000000000000 ) ) ;
#17917 = LINE ( 'NONE', #28718, #20901 ) ;
#17918 = PLANE ( 'NONE',  #16126 ) ;
#17919 = EDGE_LOOP ( 'NONE', ( #47947, #7787, #26740, #24939 ) ) ;
#17920 = CYLINDRICAL_SURFACE ( 'NONE', #38519, 31.99999999999998579 ) ;
#17921 = LINE ( 'NONE', #37009, #35481 ) ;
#17922 = CARTESIAN_POINT ( 'NONE',  ( -12.50000000000000000, -107.5000000000000000, 40.00000000000000000 ) ) ;
#17923 = DIRECTION ( 'NONE',  ( -1.000000000000000000, -0.000000000000000000, -0.000000000000000000 ) ) ;
#17924 = ORIENTED_EDGE ( 'NONE', *, *, #29336, .F. ) ;
#17925 = ORIENTED_EDGE ( 'NONE', *, *, #9286, .F. ) ;
#17926 = CIRCLE ( 'NONE', #21843, 82.00000000000000000 ) ;
#17927 = DIRECTION ( 'NONE',  ( 1.000000000000000000, 0.000000000000000000, 0.000000000000000000 ) ) ;
#17928 = CIRCLE ( 'NONE', #36685, 15.99999999999999822 ) ;
#17929 = ORIENTED_EDGE ( 'NONE', *, *, #40629, .T. ) ;
#17930 = DIRECTION ( 'NONE',  ( 0.000000000000000000, 0.000000000000000000, -1.000000000000000000 ) ) ;
#17931 = CARTESIAN_POINT ( 'NONE',  ( 0.2325368248550523098, -0.7967600800029647212, -45.00000000000000000 ) ) ;
#17932 = DIRECTION ( 'NONE',  ( 0.000000000000000000, 0.000000000000000000, -1.000000000000000000 ) ) ;
#17933 = VERTEX_POINT ( 'NONE', #34944 ) ;
#17934 = CIRCLE ( 'NONE', #31248, 16.00000000000000000 ) ;
#17935 = CYLINDRICAL_SURFACE ( 'NONE', #11206, 31.99999999999998579 ) ;
#17936 = EDGE_CURVE ( 'NONE', #20591, #19470, #13160, .T. ) ;
#17937 = VERTEX_POINT ( 'NONE', #16123 ) ;
#17938 = ADVANCED_FACE ( 'NONE', ( #9002 ), #20253, .T. ) ;
#17939 = EDGE_CURVE ( 'NONE', #35290, #43648, #13445, .T. ) ;
#17940 = CARTESIAN_POINT ( 'NONE',  ( 11.99999999999999822, 46.11716303203283474, -67.80270845531838120 ) ) ;
#17941 = ADVANCED_FACE ( 'NONE', ( #46454 ), #9473, .T. ) ;
#17942 = DIRECTION ( 'NONE',  ( 0.000000000000000000, 0.8910065241883688980, -0.4539904997395445840 ) ) ;
#17943 = CARTESIAN_POINT ( 'NONE',  ( 0.000000000000000000, -120.0000000000000000, 125.0000000000000000 ) ) ;
#17944 = ORIENTED_EDGE ( 'NONE', *, *, #1164, .T. ) ;
#17945 = DIRECTION ( 'NONE',  ( -1.000000000000000000, 0.000000000000000000, 0.000000000000000000 ) ) ;
#17946 = ORIENTED_EDGE ( 'NONE', *, *, #34124, .T. ) ;
#17947 = DIRECTION ( 'NONE',  ( -1.000000000000000000, 0.000000000000000000, 0.000000000000000000 ) ) ;
#17948 = DIRECTION ( 'NONE',  ( 0.000000000000000000, 0.000000000000000000, 1.000000000000000000 ) ) ;
#17949 = EDGE_CURVE ( 'NONE', #33272, #35412, #20748, .T. ) ;
#17950 = LINE ( 'NONE', #40493, #40028 ) ;
#17951 = CIRCLE ( 'NONE', #43756, 16.00000000000000000 ) ;
#17952 = ORIENTED_EDGE ( 'NONE', *, *, #19323, .T. ) ;
#17953 = VECTOR ( 'NONE', #11585, 1000.000000000000000 ) ;
#17954 = CARTESIAN_POINT ( 'NONE',  ( 0.000000000000000000, 36.73666225445894185, 65.58780272294090707 ) ) ;
#17955 = EDGE_LOOP ( 'NONE', ( #20958, #80, #44289, #32679 ) ) ;
#17956 = ORIENTED_EDGE ( 'NONE', *, *, #32448, .T. ) ;
#17957 = ADVANCED_FACE ( 'NONE', ( #1175 ), #42788, .T. ) ;
#17958 = DIRECTION ( 'NONE',  ( 0.000000000000000000, 0.000000000000000000, 1.000000000000000000 ) ) ;
#17959 = CIRCLE ( 'NONE', #38307, 77.49899999999999523 ) ;
#17960 = DIRECTION ( 'NONE',  ( -1.000000000000000000, 0.000000000000000000, 0.000000000000000000 ) ) ;
#17961 = CARTESIAN_POINT ( 'NONE',  ( 5.822613034544236399, -142.8165987265839760, 2.500000000000000000 ) ) ;
#17962 = DIRECTION ( 'NONE',  ( -1.000000000000000000, 0.000000000000000000, 0.000000000000000000 ) ) ;
#17963 = VERTEX_POINT ( 'NONE', #24406 ) ;
#17964 = CARTESIAN_POINT ( 'NONE',  ( 11.41210121379328335, -99.40233154247455616, 5.500000000000000000 ) ) ;
#17965 = LINE ( 'NONE', #32899, #4946 ) ;
#17966 = AXIS2_PLACEMENT_3D ( 'NONE', #17549, #45197, #41291 ) ;
#17967 = DIRECTION ( 'NONE',  ( 0.000000000000000000, 0.000000000000000000, 1.000000000000000000 ) ) ;
#17968 = DIRECTION ( 'NONE',  ( -1.000000000000000000, 0.000000000000000000, -0.000000000000000000 ) ) ;
#17969 = EDGE_CURVE ( 'NONE', #21334, #24269, #2150, .T. ) ;
#17970 = DIRECTION ( 'NONE',  ( 0.000000000000000000, 0.000000000000000000, -1.000000000000000000 ) ) ;
#17971 = VERTEX_POINT ( 'NONE', #39343 ) ;
#17972 = AXIS2_PLACEMENT_3D ( 'NONE', #15681, #45297, #37479 ) ;
#17973 = CARTESIAN_POINT ( 'NONE',  ( 11.99999999999999822, -51.03279382321125723, 55.19960302592048862 ) ) ;
#17974 = DIRECTION ( 'NONE',  ( -0.000000000000000000, -1.000000000000000000, -0.000000000000000000 ) ) ;
#17975 = CARTESIAN_POINT ( 'NONE',  ( 0.000000000000000000, 40.68715046381943523, -10.41901085202036370 ) ) ;
#17976 = DIRECTION ( 'NONE',  ( -1.000000000000000000, 0.000000000000000000, -0.000000000000000000 ) ) ;
#17977 = EDGE_CURVE ( 'NONE', #40081, #18029, #17061, .T. ) ;
#17978 = DIRECTION ( 'NONE',  ( 0.000000000000000000, 0.4067366430758017626, -0.9135454576426003115 ) ) ;
#17979 = DIRECTION ( 'NONE',  ( 0.000000000000000000, 0.000000000000000000, 1.000000000000000000 ) ) ;
#17980 = ORIENTED_EDGE ( 'NONE', *, *, #4090, .F. ) ;
#17981 = DIRECTION ( 'NONE',  ( -0.000000000000000000, -0.000000000000000000, -1.000000000000000000 ) ) ;
#17982 = LINE ( 'NONE', #21676, #33796 ) ;
#17983 = ORIENTED_EDGE ( 'NONE', *, *, #39391, .F. ) ;
#17984 = ORIENTED_EDGE ( 'NONE', *, *, #6759, .T. ) ;
#17985 = AXIS2_PLACEMENT_3D ( 'NONE', #33900, #26570, #37826 ) ;
#17986 = AXIS2_PLACEMENT_3D ( 'NONE', #44082, #36254, #21078 ) ;
#17987 = EDGE_CURVE ( 'NONE', #4822, #12549, #32017, .T. ) ;
#17988 = EDGE_LOOP ( 'NONE', ( #27292, #40822, #2801, #297 ) ) ;
#17989 = AXIS2_PLACEMENT_3D ( 'NONE', #23881, #39552, #1609 ) ;
#17990 = EDGE_CURVE ( 'NONE', #31583, #24639, #27367, .T. ) ;
#17991 = DIRECTION ( 'NONE',  ( 0.000000000000000000, -0.3826834323650969427, 0.9238795325112837409 ) ) ;
#17992 = ORIENTED_EDGE ( 'NONE', *, *, #35922, .F. ) ;
#17993 = EDGE_CURVE ( 'NONE', #38319, #39373, #23398, .T. ) ;
#17994 = AXIS2_PLACEMENT_3D ( 'NONE', #2100, #17015, #12876 ) ;
#17995 = AXIS2_PLACEMENT_3D ( 'NONE', #4454, #18868, #45307 ) ;
#17996 = VERTEX_POINT ( 'NONE', #12680 ) ;
#17997 = DIRECTION ( 'NONE',  ( 0.3311129884571281101, 0.9435911131814402886, -0.000000000000000000 ) ) ;
#17998 = CIRCLE ( 'NONE', #34422, 35.50000000000000711 ) ;
#17999 = EDGE_CURVE ( 'NONE', #17342, #22498, #43737, .T. ) ;
#18000 = FACE_OUTER_BOUND ( 'NONE', #42819, .T. ) ;
#18002 = ORIENTED_EDGE ( 'NONE', *, *, #17224, .T. ) ;
#18001 = CARTESIAN_POINT ( 'NONE',  ( 0.000000000000000000, 0.000000000000000000, -44.99999999999998579 ) ) ;
#18003 = ORIENTED_EDGE ( 'NONE', *, *, #41503, .F. ) ;
#18004 = CARTESIAN_POINT ( 'NONE',  ( 11.99999999999999822, 65.64334221924964652, -41.19522573413665611 ) ) ;
#18005 = VERTEX_POINT ( 'NONE', #38879 ) ;
#18006 = VERTEX_POINT ( 'NONE', #5339 ) ;
#18007 = VERTEX_POINT ( 'NONE', #11109 ) ;
#18008 = DIRECTION ( 'NONE',  ( -1.000000000000000000, -0.000000000000000000, -0.000000000000000000 ) ) ;
#18009 = DIRECTION ( 'NONE',  ( 0.4279312458752991266, 0.9038112904824847638, 0.000000000000000000 ) ) ;
#18010 = CARTESIAN_POINT ( 'NONE',  ( 5.000000000000002665, 80.28980883073781172, -16.65972982744850839 ) ) ;
#18011 = EDGE_LOOP ( 'NONE', ( #12221, #13320, #43861, #19512 ) ) ;
#18012 = ORIENTED_EDGE ( 'NONE', *, *, #29938, .F. ) ;
#18013 = VERTEX_POINT ( 'NONE', #29470 ) ;
#18014 = DIRECTION ( 'NONE',  ( -1.000000000000000000, 0.000000000000000000, 0.000000000000000000 ) ) ;
#18015 = ORIENTED_EDGE ( 'NONE', *, *, #19659, .T. ) ;
#18016 = PLANE ( 'NONE',  #34243 ) ;
#18017 = CARTESIAN_POINT ( 'NONE',  ( 10.00000000000000000, 54.21277698773752718, -55.38113227695725271 ) ) ;
#18018 = FACE_BOUND ( 'NONE', #32295, .T. ) ;
#18019 = ORIENTED_EDGE ( 'NONE', *, *, #4831, .T. ) ;
#18020 = DIRECTION ( 'NONE',  ( 0.000000000000000000, -0.3090169943749349613, -0.9510565162951576390 ) ) ;
#18021 = CARTESIAN_POINT ( 'NONE',  ( 10.00000000000000000, 0.000000000000000000, 0.000000000000000000 ) ) ;
#18022 = CARTESIAN_POINT ( 'NONE',  ( -3.000000000000000000, 5.835314593368477354, 22.81335362449854642 ) ) ;
#18023 = DIRECTION ( 'NONE',  ( 1.000000000000000000, 0.000000000000000000, 0.000000000000000000 ) ) ;
#18024 = AXIS2_PLACEMENT_3D ( 'NONE', #8641, #23575, #4984 ) ;
#18025 = CARTESIAN_POINT ( 'NONE',  ( 0.000000000000000000, 0.000000000000000000, -44.99999999999998579 ) ) ;
#18026 = EDGE_LOOP ( 'NONE', ( #20723, #16292, #33107, #47275 ) ) ;
#18027 = CIRCLE ( 'NONE', #28205, 15.99999999999999822 ) ;
#18028 = FACE_OUTER_BOUND ( 'NONE', #43256, .T. ) ;
#18029 = VERTEX_POINT ( 'NONE', #39608 ) ;
#18030 = AXIS2_PLACEMENT_3D ( 'NONE', #31429, #20377, #38772 ) ;
#18031 = CIRCLE ( 'NONE', #3176, 82.00000000000000000 ) ;
#18032 = DIRECTION ( 'NONE',  ( -1.000000000000000000, 0.000000000000000000, -0.000000000000000000 ) ) ;
#18033 = EDGE_LOOP ( 'NONE', ( #6606, #10127 ) ) ;
#18034 = CYLINDRICAL_SURFACE ( 'NONE', #8730, 37.49900000000000233 ) ;
#18035 = DIRECTION ( 'NONE',  ( 0.000000000000000000, -0.7071067811865389130, -0.7071067811865561215 ) ) ;
#18036 = DIRECTION ( 'NONE',  ( -1.000000000000000000, -0.000000000000000000, 0.000000000000000000 ) ) ;
#18037 = VECTOR ( 'NONE', #26968, 1000.000000000000000 ) ;
#18038 = PLANE ( 'NONE',  #38115 ) ;
#18039 = FACE_OUTER_BOUND ( 'NONE', #35676, .T. ) ;
#18040 = AXIS2_PLACEMENT_3D ( 'NONE', #41828, #38151, #8518 ) ;
#18041 = DIRECTION ( 'NONE',  ( -1.000000000000000000, 0.000000000000000000, -0.000000000000000000 ) ) ;
#18042 = CARTESIAN_POINT ( 'NONE',  ( 0.000000000000000000, 0.000000000000000000, 0.000000000000000000 ) ) ;
#18043 = DIRECTION ( 'NONE',  ( 0.000000000000000000, -0.8526401643540860720, -0.5224985647159590130 ) ) ;
#18044 = ORIENTED_EDGE ( 'NONE', *, *, #25461, .T. ) ;
#18045 = ORIENTED_EDGE ( 'NONE', *, *, #14149, .F. ) ;
#18046 = ADVANCED_FACE ( 'NONE', ( #26029 ), #28575, .T. ) ;
#18047 = ADVANCED_FACE ( 'NONE', ( #29945 ), #7188, .T. ) ;
#18048 = ORIENTED_EDGE ( 'NONE', *, *, #34137, .T. ) ;
#18049 = LINE ( 'NONE', #39642, #3012 ) ;
#18050 = EDGE_CURVE ( 'NONE', #45066, #30212, #35134, .T. ) ;
#18051 = CARTESIAN_POINT ( 'NONE',  ( 0.000000000000000000, 0.000000000000000000, 0.000000000000000000 ) ) ;
#18052 = ORIENTED_EDGE ( 'NONE', *, *, #29680, .T. ) ;
#18053 = AXIS2_PLACEMENT_3D ( 'NONE', #13296, #42920, #47065 ) ;
#18054 = AXIS2_PLACEMENT_3D ( 'NONE', #16051, #31225, #43192 ) ;
#18055 = EDGE_CURVE ( 'NONE', #45536, #41225, #18451, .T. ) ;
#18056 = PLANE ( 'NONE',  #40578 ) ;
#18057 = VECTOR ( 'NONE', #5889, 1000.000000000000000 ) ;
#18058 = AXIS2_PLACEMENT_3D ( 'NONE', #10197, #43017, #32478 ) ;
#18059 = ORIENTED_EDGE ( 'NONE', *, *, #23995, .F. ) ;
#18060 = ADVANCED_FACE ( 'NONE', ( #28321 ), #24890, .T. ) ;
#18061 = VERTEX_POINT ( 'NONE', #4010 ) ;
#18062 = AXIS2_PLACEMENT_3D ( 'NONE', #18802, #44282, #7070 ) ;
#18063 = CIRCLE ( 'NONE', #29451, 42.00000000000000000 ) ;
#18064 = DIRECTION ( 'NONE',  ( 0.1850432970638667407, -0.9827303690289282967, 0.000000000000000000 ) ) ;
#18065 = ORIENTED_EDGE ( 'NONE', *, *, #43071, .F. ) ;
#18066 = LINE ( 'NONE', #10500, #29403 ) ;
#18067 = EDGE_LOOP ( 'NONE', ( #37669, #12732, #24902, #13676 ) ) ;
#18068 = CARTESIAN_POINT ( 'NONE',  ( 0.000000000000000000, 33.80338159004283938, 16.23288003029508886 ) ) ;
#18069 = VECTOR ( 'NONE', #18621, 1000.000000000000000 ) ;
#18070 = EDGE_CURVE ( 'NONE', #27291, #47457, #8539, .T. ) ;
#18071 = LINE ( 'NONE', #48187, #20755 ) ;
#18072 = DIRECTION ( 'NONE',  ( -1.000000000000000000, -0.000000000000000000, 0.000000000000000000 ) ) ;
#18073 = ORIENTED_EDGE ( 'NONE', *, *, #38676, .F. ) ;
#18074 = ORIENTED_EDGE ( 'NONE', *, *, #22996, .T. ) ;
#18075 = DIRECTION ( 'NONE',  ( -1.000000000000000000, -0.000000000000000000, 0.000000000000000000 ) ) ;
#18076 = AXIS2_PLACEMENT_3D ( 'NONE', #3970, #16371, #7870 ) ;
#18077 = FACE_OUTER_BOUND ( 'NONE', #47363, .T. ) ;
#18078 = VERTEX_POINT ( 'NONE', #6952 ) ;
#18079 = ORIENTED_EDGE ( 'NONE', *, *, #6131, .F. ) ;
#18080 = DIRECTION ( 'NONE',  ( 0.9038112904824853189, -0.4279312458752977388, 0.000000000000000000 ) ) ;
#18081 = DIRECTION ( 'NONE',  ( 1.000000000000000000, 0.000000000000000000, -0.000000000000000000 ) ) ;
#18082 = ORIENTED_EDGE ( 'NONE', *, *, #14822, .F. ) ;
#18083 = VERTEX_POINT ( 'NONE', #7442 ) ;
#18084 = DIRECTION ( 'NONE',  ( 0.000000000000000000, 0.000000000000000000, -1.000000000000000000 ) ) ;
#18085 = DIRECTION ( 'NONE',  ( 0.000000000000000000, 0.000000000000000000, 1.000000000000000000 ) ) ;
#18086 = DIRECTION ( 'NONE',  ( -0.8225049752423776450, -0.5687579148473765889, 0.000000000000000000 ) ) ;
#18087 = DIRECTION ( 'NONE',  ( 1.000000000000000000, 0.000000000000000000, 0.000000000000000000 ) ) ;
#18088 = DIRECTION ( 'NONE',  ( -0.5200609990132993854, -0.8541291221503274356, 0.000000000000000000 ) ) ;
#18090 = AXIS2_PLACEMENT_3D ( 'NONE', #8707, #13357, #23642 ) ;
#18089 = FACE_OUTER_BOUND ( 'NONE', #7498, .T. ) ;
#18091 = EDGE_CURVE ( 'NONE', #8075, #33159, #17934, .T. ) ;
#18092 = CIRCLE ( 'NONE', #3246, 82.00000000000000000 ) ;
#18093 = DIRECTION ( 'NONE',  ( 1.000000000000000000, 0.000000000000000000, 0.000000000000000000 ) ) ;
#18094 = DIRECTION ( 'NONE',  ( 1.000000000000000000, 0.000000000000000000, 0.000000000000000000 ) ) ;
#18095 = EDGE_CURVE ( 'NONE', #32527, #30674, #22628, .T. ) ;
#18096 = DIRECTION ( 'NONE',  ( -1.000000000000000000, 0.000000000000000000, 0.000000000000000000 ) ) ;
#18097 = LINE ( 'NONE', #14201, #11324 ) ;
#18098 = CIRCLE ( 'NONE', #43786, 77.49899999999999523 ) ;
#18099 = CIRCLE ( 'NONE', #11867, 16.00000000000000000 ) ;
#18100 = ADVANCED_FACE ( 'NONE', ( #44879 ), #22372, .F. ) ;
#18101 = DIRECTION ( 'NONE',  ( 0.000000000000000000, 0.9238795325112878487, -0.3826834323650874503 ) ) ;
#18102 = AXIS2_PLACEMENT_3D ( 'NONE', #40559, #41294, #11445 ) ;
#18103 = EDGE_LOOP ( 'NONE', ( #11339, #44279, #3384, #38069 ) ) ;
#18104 = VERTEX_POINT ( 'NONE', #46933 ) ;
#18105 = DIRECTION ( 'NONE',  ( 0.000000000000000000, 0.000000000000000000, 1.000000000000000000 ) ) ;
#18106 = VECTOR ( 'NONE', #45974, 1000.000000000000000 ) ;
#18107 = EDGE_CURVE ( 'NONE', #38875, #15373, #33564, .T. ) ;
#18108 = LINE ( 'NONE', #33046, #32351 ) ;
#18109 = ORIENTED_EDGE ( 'NONE', *, *, #31014, .T. ) ;
#18110 = ADVANCED_FACE ( 'NONE', ( #47168 ), #40722, .T. ) ;
#18111 = EDGE_CURVE ( 'NONE', #46082, #48048, #13399, .T. ) ;
#18112 = DIRECTION ( 'NONE',  ( -1.000000000000000000, -0.000000000000000000, -0.000000000000000000 ) ) ;
#18113 = ORIENTED_EDGE ( 'NONE', *, *, #11770, .F. ) ;
#18114 = CARTESIAN_POINT ( 'NONE',  ( 10.00000000000000000, 77.32052557432849937, -5.256550761632002633 ) ) ;
#18115 = ORIENTED_EDGE ( 'NONE', *, *, #21054, .T. ) ;
#18116 = ADVANCED_FACE ( 'NONE', ( #33611 ), #78, .T. ) ;
#18117 = ORIENTED_EDGE ( 'NONE', *, *, #30904, .T. ) ;
#18118 = CYLINDRICAL_SURFACE ( 'NONE', #16484, 16.00000000000000000 ) ;
#18119 = CYLINDRICAL_SURFACE ( 'NONE', #20644, 37.49900000000000233 ) ;
#18120 = ORIENTED_EDGE ( 'NONE', *, *, #1446, .T. ) ;
#18121 = CARTESIAN_POINT ( 'NONE',  ( -10.43921258969510824, -98.89258801967538659, 5.500000000000000000 ) ) ;
#18122 = CIRCLE ( 'NONE', #22042, 77.49899999999999523 ) ;
#18123 = ORIENTED_EDGE ( 'NONE', *, *, #45043, .T. ) ;
#18124 = CARTESIAN_POINT ( 'NONE',  ( -6.719258119307965238, -15.35072898742050107, 0.000000000000000000 ) ) ;
#18125 = CARTESIAN_POINT ( 'NONE',  ( 11.99999999999999822, 0.000000000000000000, 0.000000000000000000 ) ) ;
#18126 = ORIENTED_EDGE ( 'NONE', *, *, #18278, .T. ) ;
#18127 = CARTESIAN_POINT ( 'NONE',  ( 0.000000000000000000, -12.42422080174614862, -35.38097989696524337 ) ) ;
#18128 = CARTESIAN_POINT ( 'NONE',  ( 10.00000000000000000, -36.88895765772637247, 6.736453364083436313 ) ) ;
#18129 = DIRECTION ( 'NONE',  ( 0.000000000000000000, -0.9238795325112821866, -0.3826834323651006065 ) ) ;
#18130 = CARTESIAN_POINT ( 'NONE',  ( -10.00000000000000000, 0.000000000000000000, 0.000000000000000000 ) ) ;
#18131 = ORIENTED_EDGE ( 'NONE', *, *, #46589, .F. ) ;
#18132 = FACE_BOUND ( 'NONE', #25467, .T. ) ;
#18133 = VERTEX_POINT ( 'NONE', #15026 ) ;
#18134 = ORIENTED_EDGE ( 'NONE', *, *, #41444, .T. ) ;
#18135 = CARTESIAN_POINT ( 'NONE',  ( 15.00000000000000000, -20.55727247249726020, 16.78983467731313084 ) ) ;
#18136 = LINE ( 'NONE', #36989, #10546 ) ;
#18137 = VECTOR ( 'NONE', #11685, 999.9999999999998863 ) ;
#18138 = CARTESIAN_POINT ( 'NONE',  ( 11.99999999999999822, 0.000000000000000000, 0.000000000000000000 ) ) ;
#18139 = CYLINDRICAL_SURFACE ( 'NONE', #46954, 31.99999999999998579 ) ;
#18140 = CARTESIAN_POINT ( 'NONE',  ( -3.000000000000000000, -10.45096189432344147, 21.10159698893426494 ) ) ;
#18141 = ORIENTED_EDGE ( 'NONE', *, *, #42267, .F. ) ;
#18142 = DIRECTION ( 'NONE',  ( -0.000000000000000000, 0.8090169943749426773, 0.5877852522924797984 ) ) ;
#18143 = CARTESIAN_POINT ( 'NONE',  ( 0.000000000000000000, 36.72794159290241822, 65.59268652807223532 ) ) ;
#18144 = CARTESIAN_POINT ( 'NONE',  ( 12.50000000000000000, -132.5000000000000000, -2.500000000000000000 ) ) ;
#18145 = ORIENTED_EDGE ( 'NONE', *, *, #18230, .T. ) ;
#18146 = ADVANCED_FACE ( 'NONE', ( #48069 ), #14554, .T. ) ;
#18147 = DIRECTION ( 'NONE',  ( -0.000000000000000000, 0.1045284632676437703, -0.9945218953682742891 ) ) ;
#18148 = CYLINDRICAL_SURFACE ( 'NONE', #25414, 11.59999999999999787 ) ;
#18149 = DIRECTION ( 'NONE',  ( 0.000000000000000000, -0.8660254037844363761, -0.5000000000000039968 ) ) ;
#18150 = CYLINDRICAL_SURFACE ( 'NONE', #9092, 31.99999999999999289 ) ;
#18151 = AXIS2_PLACEMENT_3D ( 'NONE', #4397, #23221, #30333 ) ;
#18152 = EDGE_CURVE ( 'NONE', #22698, #30560, #20285, .T. ) ;
#18153 = DIRECTION ( 'NONE',  ( -1.000000000000000000, -0.000000000000000000, -0.000000000000000000 ) ) ;
#18154 = DIRECTION ( 'NONE',  ( 0.000000000000000000, 0.000000000000000000, 1.000000000000000000 ) ) ;
#18155 = CARTESIAN_POINT ( 'NONE',  ( 0.000000000000000000, -3.948201729842348850, 23.21447184625293048 ) ) ;
#18156 = DIRECTION ( 'NONE',  ( -1.000000000000000000, -0.000000000000000000, 0.000000000000000000 ) ) ;
#18157 = EDGE_CURVE ( 'NONE', #20008, #31521, #42169, .T. ) ;
#18158 = AXIS2_PLACEMENT_3D ( 'NONE', #29186, #20896, #47072 ) ;
#18159 = ORIENTED_EDGE ( 'NONE', *, *, #40056, .T. ) ;
#18160 = AXIS2_PLACEMENT_3D ( 'NONE', #31478, #38325, #4793 ) ;
#18161 = CARTESIAN_POINT ( 'NONE',  ( 0.000000000000000000, -77.16300072079641836, -27.74655509720751567 ) ) ;
#18162 = ORIENTED_EDGE ( 'NONE', *, *, #46716, .T. ) ;
#18163 = DIRECTION ( 'NONE',  ( 0.000000000000000000, -0.9876883405951393247, 0.1564344650402207104 ) ) ;
#18164 = AXIS2_PLACEMENT_3D ( 'NONE', #47641, #10451, #3094 ) ;
#18165 = APPLICATION_PROTOCOL_DEFINITION ( 'draft international standard', 'automotive_design', 1998, #695 ) ;
#18166 = VECTOR ( 'NONE', #14900, 1000.000000000000000 ) ;
#18167 = CARTESIAN_POINT ( 'NONE',  ( 15.00000000000000000, 20.85821328998756385, 10.92862929874494249 ) ) ;
#18168 = EDGE_LOOP ( 'NONE', ( #7707, #42716, #28256, #2899 ) ) ;
#18169 = EDGE_CURVE ( 'NONE', #19505, #24549, #19400, .T. ) ;
#18170 = EDGE_CURVE ( 'NONE', #26953, #14880, #39833, .T. ) ;
#18171 = AXIS2_PLACEMENT_3D ( 'NONE', #28526, #13587, #39786 ) ;
#18172 = ORIENTED_EDGE ( 'NONE', *, *, #12961, .T. ) ;
#18173 = AXIS2_PLACEMENT_3D ( 'NONE', #39022, #46616, #6219 ) ;
#18174 = LINE ( 'NONE', #33119, #44923 ) ;
#18175 = ORIENTED_EDGE ( 'NONE', *, *, #34532, .T. ) ;
#18176 = PRODUCT_RELATED_PRODUCT_CATEGORY ( 'part', '', ( #36283 ) ) ;
#18177 = ORIENTED_EDGE ( 'NONE', *, *, #4049, .T. ) ;
#18178 = ADVANCED_FACE ( 'NONE', ( #38260 ), #34324, .T. ) ;
#18179 = CARTESIAN_POINT ( 'NONE',  ( 11.99999999999999822, -39.47590169984896846, 71.87247863392398983 ) ) ;
#18180 = ORIENTED_EDGE ( 'NONE', *, *, #37578, .F. ) ;
#18181 = CARTESIAN_POINT ( 'NONE',  ( 10.00000000000000000, 29.81001611431041098, -22.74946021919100403 ) ) ;
#18182 = CARTESIAN_POINT ( 'NONE',  ( 0.000000000000000000, -31.47745569255189224, 68.26794271651249346 ) ) ;
#18183 = ORIENTED_EDGE ( 'NONE', *, *, #18856, .F. ) ;
#18184 = CARTESIAN_POINT ( 'NONE',  ( 10.00000000000000000, 17.80606268964585226, -33.00180498840028775 ) ) ;
#18185 = CIRCLE ( 'NONE', #26022, 31.99999999999999645 ) ;
#18186 = ORIENTED_EDGE ( 'NONE', *, *, #12187, .F. ) ;
#18187 = FACE_OUTER_BOUND ( 'NONE', #23273, .T. ) ;
#18188 = CARTESIAN_POINT ( 'NONE',  ( 0.4301293587033142574, -121.4370068666438556, -2.500000000000000000 ) ) ;
#18189 = CARTESIAN_POINT ( 'NONE',  ( 0.000000000000000000, -68.67312586195022561, 35.91791733033449674 ) ) ;
#18190 = VECTOR ( 'NONE', #9552, 999.9999999999998863 ) ;
#18192 = VERTEX_POINT ( 'NONE', #4965 ) ;
#18191 = CARTESIAN_POINT ( 'NONE',  ( 5.000000000000000000, 77.16300072079700101, -27.74655509720590629 ) ) ;
#18193 = CIRCLE ( 'NONE', #34607, 16.00000000000000000 ) ;
#18194 = ORIENTED_EDGE ( 'NONE', *, *, #43667, .F. ) ;
#18195 = LINE ( 'NONE', #33387, #10744 ) ;
#18196 = ORIENTED_EDGE ( 'NONE', *, *, #26791, .T. ) ;
#18197 = ORIENTED_EDGE ( 'NONE', *, *, #45109, .T. ) ;
#18198 =( REPRESENTATION_RELATIONSHIP ('NONE','NONE', #5957, #31260 ) REPRESENTATION_RELATIONSHIP_WITH_TRANSFORMATION ( #38477 )SHAPE_REPRESENTATION_RELATIONSHIP( ) );
#18199 = CIRCLE ( 'NONE', #24464, 77.49899999999998101 ) ;
#18200 = LINE ( 'NONE', #3523, #25410 ) ;
#18201 = CIRCLE ( 'NONE', #28495, 82.00000000000000000 ) ;
#18202 = CARTESIAN_POINT ( 'NONE',  ( 0.000000000000000000, -0.9646360437372163421, -23.52805723605591126 ) ) ;
#18203 = AXIS2_PLACEMENT_3D ( 'NONE', #457, #15150, #27138 ) ;
#18204 = DIRECTION ( 'NONE',  ( 1.000000000000000000, 0.000000000000000000, 0.000000000000000000 ) ) ;
#18205 = CARTESIAN_POINT ( 'NONE',  ( 0.000000000000000000, 0.000000000000000000, 0.000000000000000000 ) ) ;
#18206 = ORIENTED_EDGE ( 'NONE', *, *, #47482, .F. ) ;
#18207 = DIRECTION ( 'NONE',  ( 0.9918136447140104561, -0.1276937514489679681, 0.000000000000000000 ) ) ;
#18208 = VECTOR ( 'NONE', #39624, 1000.000000000000000 ) ;
#18209 = CYLINDRICAL_SURFACE ( 'NONE', #44775, 16.00000000000000000 ) ;
#18210 = DIRECTION ( 'NONE',  ( -1.000000000000000000, -0.000000000000000000, -0.000000000000000000 ) ) ;
#18211 = CARTESIAN_POINT ( 'NONE',  ( 11.99999999999999822, 50.95692526931414790, -58.39081064771693974 ) ) ;
#18212 = DIRECTION ( 'NONE',  ( 0.000000000000000000, 0.000000000000000000, 1.000000000000000000 ) ) ;
#18213 = ORIENTED_EDGE ( 'NONE', *, *, #19225, .F. ) ;
#18214 = AXIS2_PLACEMENT_3D ( 'NONE', #588, #19185, #23574 ) ;
#18215 = DIRECTION ( 'NONE',  ( 0.000000000000000000, 0.000000000000000000, 1.000000000000000000 ) ) ;
#18216 = LINE ( 'NONE', #9737, #38056 ) ;
#18217 = EDGE_CURVE ( 'NONE', #37702, #17845, #30467, .T. ) ;
#18218 = DIRECTION ( 'NONE',  ( 1.000000000000000000, 0.000000000000000000, 0.000000000000000000 ) ) ;
#18219 = DIRECTION ( 'NONE',  ( -1.000000000000000000, 0.000000000000000000, -0.000000000000000000 ) ) ;
#18220 = EDGE_CURVE ( 'NONE', #10015, #19091, #35900, .T. ) ;
#18221 = CARTESIAN_POINT ( 'NONE',  ( 11.99999999999999822, 71.91182617369230456, -28.89263327155667938 ) ) ;
#18222 = DIRECTION ( 'NONE',  ( -1.000000000000000000, -0.000000000000000000, -0.000000000000000000 ) ) ;
#18223 = FACE_OUTER_BOUND ( 'NONE', #26965, .T. ) ;
#18224 = ORIENTED_EDGE ( 'NONE', *, *, #9119, .T. ) ;
#18225 = DIRECTION ( 'NONE',  ( -1.000000000000000000, 0.000000000000000000, 0.000000000000000000 ) ) ;
#18226 = CARTESIAN_POINT ( 'NONE',  ( 15.00000000000000000, 8.688484142253932063, -21.88630264137371029 ) ) ;
#18227 = ORIENTED_EDGE ( 'NONE', *, *, #3912, .F. ) ;
#18228 = EDGE_CURVE ( 'NONE', #36977, #26066, #23812, .T. ) ;
#18229 = CIRCLE ( 'NONE', #30764, 31.99999999999998579 ) ;
#18230 = EDGE_CURVE ( 'NONE', #8878, #42578, #14813, .T. ) ;
#18231 = ORIENTED_EDGE ( 'NONE', *, *, #48360, .F. ) ;
#18232 = AXIS2_PLACEMENT_3D ( 'NONE', #44411, #37060, #45139 ) ;
#18233 = AXIS2_PLACEMENT_3D ( 'NONE', #31540, #1429, #9477 ) ;
#18234 = VECTOR ( 'NONE', #18544, 1000.000000000000000 ) ;
#18235 = AXIS2_PLACEMENT_3D ( 'NONE', #3830, #12159, #30496 ) ;
#18236 = DIRECTION ( 'NONE',  ( -1.000000000000000000, 0.000000000000000000, -0.000000000000000000 ) ) ;
#18237 = ORIENTED_EDGE ( 'NONE', *, *, #30294, .F. ) ;
#18238 = VECTOR ( 'NONE', #36644, 1000.000000000000000 ) ;
#18239 = ORIENTED_EDGE ( 'NONE', *, *, #23172, .T. ) ;
#18240 = EDGE_CURVE ( 'NONE', #39340, #35947, #27015, .T. ) ;
#18241 = AXIS2_PLACEMENT_3D ( 'NONE', #13264, #1525, #16449 ) ;
#18242 = VECTOR ( 'NONE', #2816, 1000.000000000000000 ) ;
#18243 = DIRECTION ( 'NONE',  ( -1.000000000000000000, 0.000000000000000000, 0.000000000000000000 ) ) ;
#18244 = CIRCLE ( 'NONE', #4187, 82.00000000000000000 ) ;
#18245 = CARTESIAN_POINT ( 'NONE',  ( 11.99999999999999822, 22.90783923731629201, 78.73519480814962890 ) ) ;
#18246 = AXIS2_PLACEMENT_3D ( 'NONE', #5670, #39700, #35531 ) ;
#18248 = EDGE_LOOP ( 'NONE', ( #28783, #10128, #9237, #5025 ) ) ;
#18247 = CARTESIAN_POINT ( 'NONE',  ( 10.00000000000000000, -2.543863470247802905, -81.96053171279903893 ) ) ;
#18249 = ORIENTED_EDGE ( 'NONE', *, *, #12403, .T. ) ;
#18250 = DIRECTION ( 'NONE',  ( -1.000000000000000000, -0.000000000000000000, -0.000000000000000000 ) ) ;
#18251 = ORIENTED_EDGE ( 'NONE', *, *, #25417, .T. ) ;
#18252 = ORIENTED_EDGE ( 'NONE', *, *, #16486, .F. ) ;
#18253 = VECTOR ( 'NONE', #41340, 999.9999999999998863 ) ;
#18254 = CARTESIAN_POINT ( 'NONE',  ( 50.00005079999999680, 0.000000000000000000, 0.000000000000000000 ) ) ;
#18255 = DIRECTION ( 'NONE',  ( 1.000000000000000000, -0.000000000000000000, -0.000000000000000000 ) ) ;
#18256 = FACE_BOUND ( 'NONE', #10232, .T. ) ;
#18257 = EDGE_LOOP ( 'NONE', ( #38121, #44021, #40144, #28603 ) ) ;
#18258 = ORIENTED_EDGE ( 'NONE', *, *, #7567, .F. ) ;
#18259 = DIRECTION ( 'NONE',  ( 0.000000000000000000, -0.5224985647159559043, 0.8526401643540879594 ) ) ;
#18260 = ORIENTED_EDGE ( 'NONE', *, *, #17076, .F. ) ;
#18261 = CARTESIAN_POINT ( 'NONE',  ( 10.00000000000000000, 75.54627589209970040, -17.28742895386005785 ) ) ;
#18262 = DIRECTION ( 'NONE',  ( -1.000000000000000000, 0.000000000000000000, 0.000000000000000000 ) ) ;
#18263 = CARTESIAN_POINT ( 'NONE',  ( 10.00000000000000000, 0.000000000000000000, 0.000000000000000000 ) ) ;
#18264 = CYLINDRICAL_SURFACE ( 'NONE', #37038, 16.00000000000000000 ) ;
#18265 = CARTESIAN_POINT ( 'NONE',  ( 4.999999999999999112, -10.41901085202050581, -40.68715046381939970 ) ) ;
#18266 = DIRECTION ( 'NONE',  ( 0.000000000000000000, 0.9969173337331281859, -0.07845909572784182107 ) ) ;
#18267 = CIRCLE ( 'NONE', #45634, 32.00000000000000000 ) ;
#18268 = CARTESIAN_POINT ( 'NONE',  ( 26.47460221209471598, -121.8961639463267090, 5.500000000000000000 ) ) ;
#18269 = PLANE ( 'NONE',  #22800 ) ;
#18270 = AXIS2_PLACEMENT_3D ( 'NONE', #36033, #31181, #2498 ) ;
#18271 = ORIENTED_EDGE ( 'NONE', *, *, #33912, .T. ) ;
#18272 = EDGE_CURVE ( 'NONE', #9873, #45638, #21052, .T. ) ;
#18273 = DIRECTION ( 'NONE',  ( 0.000000000000000000, 0.000000000000000000, 1.000000000000000000 ) ) ;
#18274 = ORIENTED_EDGE ( 'NONE', *, *, #45578, .T. ) ;
#18275 = CIRCLE ( 'NONE', #8959, 16.00000000000000000 ) ;
#18276 = AXIS2_PLACEMENT_3D ( 'NONE', #19460, #37600, #22439 ) ;
#18277 = VECTOR ( 'NONE', #10663, 1000.000000000000000 ) ;
#18278 = EDGE_CURVE ( 'NONE', #21831, #15376, #37773, .T. ) ;
#18279 = CARTESIAN_POINT ( 'NONE',  ( 11.99999999999999822, 55.19960302592066625, 51.03279382321107249 ) ) ;
#18280 = EDGE_LOOP ( 'NONE', ( #14820, #23865, #23913, #35128 ) ) ;
#18281 = CARTESIAN_POINT ( 'NONE',  ( 10.00000000000000000, 0.000000000000000000, 0.000000000000000000 ) ) ;
#18282 = DIRECTION ( 'NONE',  ( 0.000000000000000000, 0.8090169943749445647, 0.5877852522924770229 ) ) ;
#18283 = ADVANCED_FACE ( 'NONE', ( #19882 ), #799, .T. ) ;
#18284 = CARTESIAN_POINT ( 'NONE',  ( 11.99999999999999822, 0.000000000000000000, 0.000000000000000000 ) ) ;
#18285 = DIRECTION ( 'NONE',  ( -1.000000000000000000, -0.000000000000000000, -0.000000000000000000 ) ) ;
#18286 = VECTOR ( 'NONE', #35328, 1000.000000000000000 ) ;
#18287 = CARTESIAN_POINT ( 'NONE',  ( 11.99999999999999822, -69.42325613327415113, -34.44570377933671779 ) ) ;
#18288 = EDGE_CURVE ( 'NONE', #20918, #38585, #27328, .T. ) ;
#18289 = DIRECTION ( 'NONE',  ( 0.6575728627325954090, -0.7533909544171998318, 0.000000000000000000 ) ) ;
#18290 = EDGE_CURVE ( 'NONE', #47513, #46797, #6222, .T. ) ;
#18291 = CIRCLE ( 'NONE', #37054, 16.00000000000000355 ) ;
#18292 = AXIS2_PLACEMENT_3D ( 'NONE', #47273, #3178, #37207 ) ;
#18293 = AXIS2_PLACEMENT_3D ( 'NONE', #1119, #41523, #31241 ) ;
#18294 = CARTESIAN_POINT ( 'NONE',  ( 6.000000000000000000, 22.90783923731629201, 78.73519480814962890 ) ) ;
#18295 =( NAMED_UNIT ( * ) PLANE_ANGLE_UNIT ( ) SI_UNIT ( $, .RADIAN. ) );
#18296 = CARTESIAN_POINT ( 'NONE',  ( 10.00000000000000000, -20.41045688087772092, -72.35160999960838524 ) ) ;
#18297 = AXIS2_PLACEMENT_3D ( 'NONE', #23799, #13037, #31894 ) ;
#18298 = ORIENTED_EDGE ( 'NONE', *, *, #36549, .F. ) ;
#18299 = ORIENTED_EDGE ( 'NONE', *, *, #25333, .T. ) ;
#18300 = CARTESIAN_POINT ( 'NONE',  ( 10.00000000000000000, 27.05870788708231700, 26.08949754953034272 ) ) ;
#18301 = DIRECTION ( 'NONE',  ( -1.000000000000000000, 0.000000000000000000, -0.000000000000000000 ) ) ;
#18302 = ORIENTED_EDGE ( 'NONE', *, *, #47616, .T. ) ;
#18303 = EDGE_LOOP ( 'NONE', ( #38270, #5798, #15691, #36475 ) ) ;
#18304 = EDGE_CURVE ( 'NONE', #42290, #9518, #4494, .T. ) ;
#18305 = CIRCLE ( 'NONE', #24578, 31.99999999999999289 ) ;
#18306 = DIRECTION ( 'NONE',  ( -0.3853207896976547642, 0.9227826878668540234, 0.000000000000000000 ) ) ;
#18307 = VECTOR ( 'NONE', #21157, 1000.000000000000000 ) ;
#18308 = EDGE_LOOP ( 'NONE', ( #34431, #36689, #43659, #37651 ) ) ;
#18309 = EDGE_LOOP ( 'NONE', ( #10031, #21853, #37151, #5346 ) ) ;
#18310 = VECTOR ( 'NONE', #47049, 1000.000000000000000 ) ;
#18311 = PRODUCT_DEFINITION_SHAPE ( 'NONE', 'NONE',  #48464 ) ;
#18312 = EDGE_CURVE ( 'NONE', #40415, #26939, #25763, .T. ) ;
#18313 = EDGE_CURVE ( 'NONE', #17075, #35109, #46093, .T. ) ;
#18314 = DIRECTION ( 'NONE',  ( -1.000000000000000000, -0.000000000000000000, 0.000000000000000000 ) ) ;
#18315 = VECTOR ( 'NONE', #3410, 1000.000000000000000 ) ;
#18316 = ORIENTED_EDGE ( 'NONE', *, *, #1011, .T. ) ;
#18317 = DIRECTION ( 'NONE',  ( -1.000000000000000000, -0.000000000000000000, -0.000000000000000000 ) ) ;
#18318 = EDGE_LOOP ( 'NONE', ( #26221, #45793, #11025, #40642 ) ) ;
#18319 = EDGE_LOOP ( 'NONE', ( #7192, #33893, #727, #12973 ) ) ;
#18320 = AXIS2_PLACEMENT_3D ( 'NONE', #15359, #30285, #25860 ) ;
#18321 = CARTESIAN_POINT ( 'NONE',  ( 10.00000000000000000, 77.49459641780886443, -0.8261519478433788644 ) ) ;
#18322 = CIRCLE ( 'NONE', #13618, 77.49899999999998101 ) ;
#18323 = DIRECTION ( 'NONE',  ( 1.000000000000000000, 0.000000000000000000, -0.000000000000000000 ) ) ;
#18324 = CARTESIAN_POINT ( 'NONE',  ( 50.00005079999999680, 12.24744871391589207, -2.500000000000000000 ) ) ;
#18326 = VERTEX_POINT ( 'NONE', #41946 ) ;
#18325 = CIRCLE ( 'NONE', #32398, 42.00000000000000000 ) ;
#18327 = VERTEX_POINT ( 'NONE', #27251 ) ;
#18329 = EDGE_CURVE ( 'NONE', #23892, #15601, #38288, .T. ) ;
#18328 = CARTESIAN_POINT ( 'NONE',  ( 30.50000000000000000, -120.0000000000000000, 2.500000000000000000 ) ) ;
#18330 = DIRECTION ( 'NONE',  ( -0.9918136447140101231, 0.1276937514489694114, 0.000000000000000000 ) ) ;
#18331 = ORIENTED_EDGE ( 'NONE', *, *, #25661, .T. ) ;
#18332 = ORIENTED_EDGE ( 'NONE', *, *, #6940, .T. ) ;
#18333 = EDGE_CURVE ( 'NONE', #29949, #5918, #46078, .T. ) ;
#18334 = DIRECTION ( 'NONE',  ( -1.000000000000000000, -0.000000000000000000, -0.000000000000000000 ) ) ;
#18335 = DIRECTION ( 'NONE',  ( 0.000000000000000000, -0.2334453638559126909, 0.9723699203976748917 ) ) ;
#18336 = ORIENTED_EDGE ( 'NONE', *, *, #6196, .F. ) ;
#18337 = CARTESIAN_POINT ( 'NONE',  ( 11.99999999999999822, 20.41045688087824317, 72.35160999960824313 ) ) ;
#18338 = CARTESIAN_POINT ( 'NONE',  ( 0.000000000000000000, 0.000000000000000000, 0.000000000000000000 ) ) ;
#18339 = CARTESIAN_POINT ( 'NONE',  ( 11.99999999999999822, 59.03342792756328095, -46.54456581323744757 ) ) ;
#18340 = EDGE_LOOP ( 'NONE', ( #34656, #24659, #26267, #35334 ) ) ;
#18341 = ADVANCED_FACE ( 'NONE', ( #20869 ), #31419, .T. ) ;
#18342 = LINE ( 'NONE', #37920, #6450 ) ;
#18343 = FACE_OUTER_BOUND ( 'NONE', #17006, .T. ) ;
#18344 = DIRECTION ( 'NONE',  ( -1.000000000000000000, -0.000000000000000000, -0.000000000000000000 ) ) ;
#18345 = AXIS2_PLACEMENT_3D ( 'NONE', #45990, #28104, #23454 ) ;
#18346 = LINE ( 'NONE', #3162, #30207 ) ;
#18347 = FACE_OUTER_BOUND ( 'NONE', #10266, .T. ) ;
#18348 = ADVANCED_FACE ( 'NONE', ( #24781 ), #17173, .T. ) ;
#18349 = AXIS2_PLACEMENT_3D ( 'NONE', #11414, #41263, #45397 ) ;
#18350 = AXIS2_PLACEMENT_3D ( 'NONE', #15251, #26498, #27225 ) ;
#18351 = CYLINDRICAL_SURFACE ( 'NONE', #37745, 77.49899999999999523 ) ;
#18352 = LINE ( 'NONE', #29850, #4260 ) ;
#18353 = SURFACE_STYLE_USAGE ( .BOTH. , #7335 ) ;
#18354 = LINE ( 'NONE', #47713, #23274 ) ;
#18355 = ORIENTED_EDGE ( 'NONE', *, *, #36782, .T. ) ;
#18356 = VERTEX_POINT ( 'NONE', #12801 ) ;
#18357 = VERTEX_POINT ( 'NONE', #24290 ) ;
#18358 = VECTOR ( 'NONE', #15732, 1000.000000000000000 ) ;
#18359 = VECTOR ( 'NONE', #6270, 1000.000000000000000 ) ;
#18360 = CYLINDRICAL_SURFACE ( 'NONE', #16006, 12.49999999999999645 ) ;
#18361 = VECTOR ( 'NONE', #7075, 1000.000000000000114 ) ;
#18362 = CARTESIAN_POINT ( 'NONE',  ( 11.99999999999999822, -54.21277698773636899, -55.38113227695839669 ) ) ;
#18363 = CIRCLE ( 'NONE', #35570, 31.99999999999998579 ) ;
#18364 = EDGE_LOOP ( 'NONE', ( #31767, #79, #31462, #11775 ) ) ;
#18365 = VECTOR ( 'NONE', #22044, 1000.000000000000114 ) ;
#18366 = CYLINDRICAL_SURFACE ( 'NONE', #35862, 16.00000000000000000 ) ;
#18367 = ORIENTED_EDGE ( 'NONE', *, *, #2636, .T. ) ;
#18368 = CARTESIAN_POINT ( 'NONE',  ( 11.99999999999999822, -3.894527615418461153, 81.90746397400387480 ) ) ;
#18369 = ORIENTED_EDGE ( 'NONE', *, *, #10625, .F. ) ;
#18370 = ORIENTED_EDGE ( 'NONE', *, *, #13761, .T. ) ;
#18371 = VERTEX_POINT ( 'NONE', #17411 ) ;
#18372 = AXIS2_PLACEMENT_3D ( 'NONE', #6380, #21288, #35984 ) ;
#18373 = ORIENTED_EDGE ( 'NONE', *, *, #29855, .T. ) ;
#18374 = CARTESIAN_POINT ( 'NONE',  ( 10.00000000000000000, -11.30684508768395524, 76.66974797899831628 ) ) ;
#18375 = AXIS2_PLACEMENT_3D ( 'NONE', #41473, #16012, #7925 ) ;
#18376 = DIRECTION ( 'NONE',  ( 0.000000000000000000, 0.000000000000000000, -1.000000000000000000 ) ) ;
#18377 = VERTEX_POINT ( 'NONE', #47051 ) ;
#18378 = ORIENTED_EDGE ( 'NONE', *, *, #39852, .F. ) ;
#18379 = AXIS2_PLACEMENT_3D ( 'NONE', #26765, #8634, #34831 ) ;
#18380 = CARTESIAN_POINT ( 'NONE',  ( 10.00000000000000000, -68.67312586194971402, -35.91791733033549860 ) ) ;
#18381 = EDGE_CURVE ( 'NONE', #8188, #14587, #32368, .T. ) ;
#18382 = ORIENTED_EDGE ( 'NONE', *, *, #40876, .T. ) ;
#18383 = DIRECTION ( 'NONE',  ( 0.000000000000000000, 0.000000000000000000, 1.000000000000000000 ) ) ;
#18384 = DIRECTION ( 'NONE',  ( -1.000000000000000000, 0.000000000000000000, 0.000000000000000000 ) ) ;
#18385 = EDGE_LOOP ( 'NONE', ( #6824, #46185, #40472, #44104 ) ) ;
#18386 = CARTESIAN_POINT ( 'NONE',  ( 0.000000000000000000, -55.38113227695745167, -54.21277698773732823 ) ) ;
#18387 = CARTESIAN_POINT ( 'NONE',  ( 11.99999999999999822, 71.87247863392470038, -39.47590169984768949 ) ) ;
#18388 = VERTEX_POINT ( 'NONE', #25001 ) ;
#18389 = DIRECTION ( 'NONE',  ( -0.9435911131814398445, 0.3311129884571295534, 0.000000000000000000 ) ) ;
#18390 = CARTESIAN_POINT ( 'NONE',  ( 10.00000000000000000, 33.00180498840072829, -17.80606268964504935 ) ) ;
#18391 = AXIS2_PLACEMENT_3D ( 'NONE', #4248, #34089, #43133 ) ;
#18392 = AXIS2_PLACEMENT_3D ( 'NONE', #24782, #17414, #47294 ) ;
#18393 = ORIENTED_EDGE ( 'NONE', *, *, #21373, .F. ) ;
#18394 = LINE ( 'NONE', #33326, #45165 ) ;
#18395 = ORIENTED_EDGE ( 'NONE', *, *, #10515, .F. ) ;
#18396 = ORIENTED_EDGE ( 'NONE', *, *, #456, .F. ) ;
#18397 = CARTESIAN_POINT ( 'NONE',  ( 0.000000000000000000, 9.188173127307898369, -40.98264845739739570 ) ) ;
#18398 = CARTESIAN_POINT ( 'NONE',  ( 10.00000000000000000, -68.67312586195023982, 35.91791733033450384 ) ) ;
#18399 = VERTEX_POINT ( 'NONE', #13281 ) ;
#18400 = CYLINDRICAL_SURFACE ( 'NONE', #44866, 11.59999999999999787 ) ;
#18401 = AXIS2_PLACEMENT_3D ( 'NONE', #13355, #13591, #43211 ) ;
#18402 = CARTESIAN_POINT ( 'NONE',  ( -3.000000000000000000, 8.688484142253939169, 21.88630264137371029 ) ) ;
#18403 = DIRECTION ( 'NONE',  ( 0.000000000000000000, -0.9723699203976789995, 0.2334453638558957322 ) ) ;
#18404 = VERTEX_POINT ( 'NONE', #28444 ) ;
#18405 = EDGE_CURVE ( 'NONE', #9566, #17161, #9127, .T. ) ;
#18406 = AXIS2_PLACEMENT_3D ( 'NONE', #23877, #12621, #8941 ) ;
#18407 = DIRECTION ( 'NONE',  ( -1.000000000000000000, -0.000000000000000000, -0.000000000000000000 ) ) ;
#18408 = ADVANCED_FACE ( 'NONE', ( #39225 ), #9843, .F. ) ;
#18409 = ADVANCED_FACE ( 'NONE', ( #5951 ), #39478, .T. ) ;
#18410 = CARTESIAN_POINT ( 'NONE',  ( 0.000000000000000000, -71.27951684758005513, -30.41916302227188851 ) ) ;
#18411 = DIRECTION ( 'NONE',  ( -1.000000000000000000, 0.000000000000000000, 0.000000000000000000 ) ) ;
#18412 = ORIENTED_EDGE ( 'NONE', *, *, #8425, .T. ) ;
#18413 = FACE_OUTER_BOUND ( 'NONE', #42912, .T. ) ;
#18414 = PLANE ( 'NONE',  #30054 ) ;
#18415 = CARTESIAN_POINT ( 'NONE',  ( -8.826826895187510402, -94.96827758698185562, 5.500000000000000000 ) ) ;
#18416 = DIRECTION ( 'NONE',  ( 0.000000000000000000, 0.7431448254773939111, 0.6691306063588584596 ) ) ;
#18417 = EDGE_CURVE ( 'NONE', #40145, #4970, #40648, .T. ) ;
#18418 = VECTOR ( 'NONE', #5856, 1000.000000000000000 ) ;
#18419 = EDGE_CURVE ( 'NONE', #43648, #28726, #46817, .T. ) ;
#18420 = CARTESIAN_POINT ( 'NONE',  ( 5.000000000000000000, 60.67117009219216328, -55.16347631942977614 ) ) ;
#18421 = DIRECTION ( 'NONE',  ( 0.000000000000000000, -0.9969173337331287410, 0.07845909572783489605 ) ) ;
#18422 = CARTESIAN_POINT ( 'NONE',  ( 26.47460221209471598, -121.8961639463267090, 5.500000000000000000 ) ) ;
#18423 = CARTESIAN_POINT ( 'NONE',  ( 5.000000000000000000, 63.97538442413426907, 51.29473840253247374 ) ) ;
#18424 = ORIENTED_EDGE ( 'NONE', *, *, #4216, .F. ) ;
#18425 = DIRECTION ( 'NONE',  ( 0.000000000000000000, -0.7071067811865389130, -0.7071067811865563435 ) ) ;
#18426 = VERTEX_POINT ( 'NONE', #42669 ) ;
#18427 = DIRECTION ( 'NONE',  ( 0.000000000000000000, 0.000000000000000000, 1.000000000000000000 ) ) ;
#18428 =( NAMED_UNIT ( * ) PLANE_ANGLE_UNIT ( ) SI_UNIT ( $, .RADIAN. ) );
#18429 = DIRECTION ( 'NONE',  ( 0.000000000000000000, 0.8910065241883688980, -0.4539904997395447506 ) ) ;
#18430 = ORIENTED_EDGE ( 'NONE', *, *, #11888, .T. ) ;
#18431 = VECTOR ( 'NONE', #12015, 1000.000000000000000 ) ;
#18432 = LINE ( 'NONE', #6935, #4183 ) ;
#18433 = CIRCLE ( 'NONE', #31746, 31.99999999999999289 ) ;
#18434 = VERTEX_POINT ( 'NONE', #13769 ) ;
#18435 = AXIS2_PLACEMENT_3D ( 'NONE', #22608, #15748, #16474 ) ;
#18436 = EDGE_CURVE ( 'NONE', #1080, #11405, #6259, .T. ) ;
#18437 = DIRECTION ( 'NONE',  ( 0.000000000000000000, 0.000000000000000000, 1.000000000000000000 ) ) ;
#18438 = ORIENTED_EDGE ( 'NONE', *, *, #10539, .F. ) ;
#18439 = FACE_OUTER_BOUND ( 'NONE', #31399, .T. ) ;
#18440 = DIRECTION ( 'NONE',  ( -0.000000000000000000, 0.000000000000000000, -1.000000000000000000 ) ) ;
#18441 = ADVANCED_FACE ( 'NONE', ( #43619 ), #21087, .T. ) ;
#18442 = ORIENTED_EDGE ( 'NONE', *, *, #33929, .T. ) ;
#18443 = DIRECTION ( 'NONE',  ( -1.000000000000000000, 0.000000000000000000, 0.000000000000000000 ) ) ;
#18444 = VECTOR ( 'NONE', #43098, 1000.000000000000000 ) ;
#18445 = CIRCLE ( 'NONE', #15319, 16.00000000000000000 ) ;
#18446 = ADVANCED_FACE ( 'NONE', ( #16468 ), #47664, .T. ) ;
#18447 = DIRECTION ( 'NONE',  ( -0.02332147558787930897, -0.9997280174009348652, 0.000000000000000000 ) ) ;
#18448 = FACE_OUTER_BOUND ( 'NONE', #16121, .T. ) ;
#18449 = CARTESIAN_POINT ( 'NONE',  ( 0.000000000000000000, -21.60688246758530084, -79.10210256391388839 ) ) ;
#18450 = VECTOR ( 'NONE', #4154, 1000.000000000000114 ) ;
#18451 = LINE ( 'NONE', #43509, #11695 ) ;
#18452 = ORIENTED_EDGE ( 'NONE', *, *, #7662, .T. ) ;
#18453 = CARTESIAN_POINT ( 'NONE',  ( 3.250000000000000444, -13.95926121303099343, -1.199999999999999956 ) ) ;
#18454 = ORIENTED_EDGE ( 'NONE', *, *, #27883, .F. ) ;
#18455 = ORIENTED_EDGE ( 'NONE', *, *, #2174, .T. ) ;
#18456 = CARTESIAN_POINT ( 'NONE',  ( 11.99999999999999822, -14.66109333815410487, -73.73191006444587003 ) ) ;
#18457 = DIRECTION ( 'NONE',  ( -1.000000000000000000, -0.000000000000000000, 0.000000000000000000 ) ) ;
#18458 = DIRECTION ( 'NONE',  ( -1.000000000000000000, -0.000000000000000000, 0.000000000000000000 ) ) ;
#18459 = DIRECTION ( 'NONE',  ( -1.000000000000000000, -0.000000000000000000, -0.000000000000000000 ) ) ;
#18460 = VERTEX_POINT ( 'NONE', #5452 ) ;
#18461 = FACE_OUTER_BOUND ( 'NONE', #24857, .T. ) ;
#18462 = DIRECTION ( 'NONE',  ( -1.000000000000000000, -0.000000000000000000, 0.000000000000000000 ) ) ;
#18463 = EDGE_CURVE ( 'NONE', #29434, #21969, #21890, .T. ) ;
#18464 = EDGE_CURVE ( 'NONE', #11806, #28861, #30490, .T. ) ;
#18465 = CARTESIAN_POINT ( 'NONE',  ( -0.4301293587032979371, -118.5629931333561871, 2.500000000000000000 ) ) ;
#18466 = CARTESIAN_POINT ( 'NONE',  ( 4.999999999999999112, -38.55633173627022359, 16.65560815589396526 ) ) ;
#18467 = DIRECTION ( 'NONE',  ( -0.000000000000000000, -0.000000000000000000, 1.000000000000000000 ) ) ;
#18468 = CIRCLE ( 'NONE', #2838, 37.49900000000001654 ) ;
#18469 = CARTESIAN_POINT ( 'NONE',  ( 11.99999999999999822, -75.11764819372149304, 2.946379043146075905 ) ) ;
#18470 = ORIENTED_EDGE ( 'NONE', *, *, #44597, .F. ) ;
#18471 = CARTESIAN_POINT ( 'NONE',  ( 0.000000000000000000, 0.000000000000000000, 125.0000000000000000 ) ) ;
#18472 = DIRECTION ( 'NONE',  ( 0.000000000000000000, 0.4067366430758009854, 0.9135454576426004225 ) ) ;
#18473 = CIRCLE ( 'NONE', #19237, 31.99999999999998579 ) ;
#18474 = CARTESIAN_POINT ( 'NONE',  ( 15.00000000000000000, 20.85821328998756385, 10.92862929874494249 ) ) ;
#18475 = DIRECTION ( 'NONE',  ( 0.000000000000000000, 0.000000000000000000, 1.000000000000000000 ) ) ;
#18476 = DIRECTION ( 'NONE',  ( 0.02332147558787931590, 0.9997280174009348652, 0.000000000000000000 ) ) ;
#18477 = EDGE_CURVE ( 'NONE', #17581, #38891, #24992, .T. ) ;
#18478 = ORIENTED_EDGE ( 'NONE', *, *, #21819, .T. ) ;
#18479 = DIRECTION ( 'NONE',  ( 0.000000000000000000, 0.000000000000000000, -1.000000000000000000 ) ) ;
#18480 = CARTESIAN_POINT ( 'NONE',  ( 0.000000000000000000, -77.19088730480518734, -6.903761155838607166 ) ) ;
#18481 = AXIS2_PLACEMENT_3D ( 'NONE', #45022, #11498, #4147 ) ;
#18482 = CARTESIAN_POINT ( 'NONE',  ( 10.00000000000000000, 0.000000000000000000, 0.000000000000000000 ) ) ;
#18483 = CARTESIAN_POINT ( 'NONE',  ( 11.99999999999999822, 34.94270380257741238, -74.18225833017854143 ) ) ;
#18484 = CIRCLE ( 'NONE', #5992, 31.99999999999998934 ) ;
#18485 = VECTOR ( 'NONE', #26224, 999.9999999999998863 ) ;
#18486 = DIRECTION ( 'NONE',  ( -1.000000000000000000, -0.000000000000000000, 0.000000000000000000 ) ) ;
#18487 = ORIENTED_EDGE ( 'NONE', *, *, #5321, .F. ) ;
#18488 = ORIENTED_EDGE ( 'NONE', *, *, #2903, .F. ) ;
#18489 = VECTOR ( 'NONE', #3352, 1000.000000000000000 ) ;
#18490 = VERTEX_POINT ( 'NONE', #6658 ) ;
#18491 = ORIENTED_EDGE ( 'NONE', *, *, #11997, .T. ) ;
#18492 = CARTESIAN_POINT ( 'NONE',  ( 0.000000000000000000, 0.000000000000000000, -1.199999999999999956 ) ) ;
#18493 = VERTEX_POINT ( 'NONE', #25485 ) ;
#18494 = AXIS2_PLACEMENT_3D ( 'NONE', #9185, #39280, #9655 ) ;
#18495 = EDGE_CURVE ( 'NONE', #44863, #33047, #12510, .T. ) ;
#18496 = LINE ( 'NONE', #21913, #16796 ) ;
#18497 = CARTESIAN_POINT ( 'NONE',  ( -35.37301231164799731, -123.0000000000000142, -2.500000000000000000 ) ) ;
#18498 = CARTESIAN_POINT ( 'NONE',  ( -15.44521549751111422, -137.7748507232956001, 5.500000000000000000 ) ) ;
#18499 = EDGE_CURVE ( 'NONE', #40483, #6863, #19531, .T. ) ;
#18500 = EDGE_LOOP ( 'NONE', ( #13876, #24291, #41856, #20705 ) ) ;
#18501 = AXIS2_PLACEMENT_3D ( 'NONE', #20822, #31864, #46781 ) ;
#18502 = DIRECTION ( 'NONE',  ( -1.000000000000000000, -0.000000000000000000, -0.000000000000000000 ) ) ;
#18503 = VERTEX_POINT ( 'NONE', #44574 ) ;
#18504 = ORIENTED_EDGE ( 'NONE', *, *, #6010, .F. ) ;
#18505 = EDGE_CURVE ( 'NONE', #5920, #13159, #25718, .T. ) ;
#18506 = ORIENTED_EDGE ( 'NONE', *, *, #1767, .T. ) ;
#18507 = DIRECTION ( 'NONE',  ( 0.02332147558787931590, 0.9997280174009348652, 0.000000000000000000 ) ) ;
#18508 = DIRECTION ( 'NONE',  ( -1.000000000000000000, -0.000000000000000000, 0.000000000000000000 ) ) ;
#18509 = DIRECTION ( 'NONE',  ( -1.000000000000000000, 0.000000000000000000, 0.000000000000000000 ) ) ;
#18510 = VERTEX_POINT ( 'NONE', #36264 ) ;
#18511 = AXIS2_PLACEMENT_3D ( 'NONE', #46839, #27765, #16261 ) ;
#18512 = VERTEX_POINT ( 'NONE', #29886 ) ;
#18513 = DIRECTION ( 'NONE',  ( -0.000000000000000000, -0.000000000000000000, -1.000000000000000000 ) ) ;
#18514 = ORIENTED_EDGE ( 'NONE', *, *, #16102, .F. ) ;
#18515 = DIRECTION ( 'NONE',  ( -1.000000000000000000, -0.000000000000000000, -0.000000000000000000 ) ) ;
#18516 = FACE_OUTER_BOUND ( 'NONE', #21224, .T. ) ;
#18517 = CARTESIAN_POINT ( 'NONE',  ( 15.00000000000000000, 8.688484142253932063, -21.88630264137371029 ) ) ;
#18518 = CARTESIAN_POINT ( 'NONE',  ( 0.000000000000000000, 26.01480285779837232, 70.53064760720326376 ) ) ;
#18519 = CARTESIAN_POINT ( 'NONE',  ( 23.41451323550360186, -132.5004227906269989, 5.500000000000000000 ) ) ;
#18520 = AXIS2_PLACEMENT_3D ( 'NONE', #42751, #27569, #16552 ) ;
#18521 = CARTESIAN_POINT ( 'NONE',  ( 11.99999999999999822, 49.70050353004889132, 59.46389618801982380 ) ) ;
#18522 = EDGE_CURVE ( 'NONE', #44892, #3614, #8575, .T. ) ;
#18523 = EDGE_CURVE ( 'NONE', #13979, #37298, #11048, .T. ) ;
#18524 = LINE ( 'NONE', #11666, #42193 ) ;
#18525 = CARTESIAN_POINT ( 'NONE',  ( 11.99999999999999822, 70.53064760720278059, 26.01480285779964774 ) ) ;
#18526 = ORIENTED_EDGE ( 'NONE', *, *, #27905, .T. ) ;
#18527 = CARTESIAN_POINT ( 'NONE',  ( 0.000000000000000000, 0.000000000000000000, 40.80000000000001847 ) ) ;
#18528 = ORIENTED_EDGE ( 'NONE', *, *, #37134, .T. ) ;
#18529 = EDGE_CURVE ( 'NONE', #8637, #33006, #43768, .T. ) ;
#18530 = LINE ( 'NONE', #37126, #42900 ) ;
#18531 = ORIENTED_EDGE ( 'NONE', *, *, #42270, .T. ) ;
#18532 = LINE ( 'NONE', #25623, #29268 ) ;
#18533 = DIRECTION ( 'NONE',  ( 0.000000000000000000, -0.8910065241883722287, 0.4539904997395382558 ) ) ;
#18534 = DIRECTION ( 'NONE',  ( -1.000000000000000000, 0.000000000000000000, 0.000000000000000000 ) ) ;
#18535 = LINE ( 'NONE', #10716, #41181 ) ;
#18536 = CARTESIAN_POINT ( 'NONE',  ( -1.384174031800281979, -120.5779811845464735, -2.500000000000000000 ) ) ;
#18537 = EDGE_CURVE ( 'NONE', #37110, #30509, #39867, .T. ) ;
#18538 = AXIS2_PLACEMENT_3D ( 'NONE', #30937, #45862, #11836 ) ;
#18539 = DIRECTION ( 'NONE',  ( 0.000000000000000000, 0.000000000000000000, 1.000000000000000000 ) ) ;
#18540 = DIRECTION ( 'NONE',  ( 0.000000000000000000, 0.000000000000000000, 1.000000000000000000 ) ) ;
#18541 = AXIS2_PLACEMENT_3D ( 'NONE', #3902, #47704, #40620 ) ;
#18542 = CARTESIAN_POINT ( 'NONE',  ( 15.00000000000000000, 8.688484142254226938, 21.88630264137359305 ) ) ;
#18543 =( LENGTH_UNIT ( ) NAMED_UNIT ( * ) SI_UNIT ( .MILLI., .METRE. ) );
#18544 = DIRECTION ( 'NONE',  ( 0.9781476007338070211, 2.546183866652750331E-17, 0.2079116908177527367 ) ) ;
#18545 = ORIENTED_EDGE ( 'NONE', *, *, #34204, .T. ) ;
#18546 = VERTEX_POINT ( 'NONE', #7376 ) ;
#18547 = AXIS2_PLACEMENT_3D ( 'NONE', #38596, #30293, #31258 ) ;
#18548 = EDGE_LOOP ( 'NONE', ( #38194, #30790, #22791, #8917 ) ) ;
#18549 = ORIENTED_EDGE ( 'NONE', *, *, #31038, .F. ) ;
#18550 = DIRECTION ( 'NONE',  ( 0.000000000000000000, 0.000000000000000000, -1.000000000000000000 ) ) ;
#18551 = CARTESIAN_POINT ( 'NONE',  ( -9.332068499558252128, 6.890028847512362553, -44.99999999999998579 ) ) ;
#18552 = ORIENTED_EDGE ( 'NONE', *, *, #18592, .T. ) ;
#18553 = VERTEX_POINT ( 'NONE', #14485 ) ;
#18554 = DIRECTION ( 'NONE',  ( 0.9135454576426059736, -0.4067366430757887730, 0.000000000000000000 ) ) ;
#18555 = ORIENTED_EDGE ( 'NONE', *, *, #43543, .T. ) ;
#18556 = EDGE_CURVE ( 'NONE', #33236, #21422, #5483, .T. ) ;
#18557 = ORIENTED_EDGE ( 'NONE', *, *, #31488, .F. ) ;
#18558 = ORIENTED_EDGE ( 'NONE', *, *, #4344, .T. ) ;
#18559 = EDGE_CURVE ( 'NONE', #4757, #2290, #28904, .T. ) ;
#18560 = EDGE_CURVE ( 'NONE', #29434, #10009, #3203, .T. ) ;
#18561 = EDGE_CURVE ( 'NONE', #36710, #34363, #14965, .T. ) ;
#18562 = AXIS2_PLACEMENT_3D ( 'NONE', #42121, #18632, #8100 ) ;
#18563 = DIRECTION ( 'NONE',  ( 0.000000000000000000, 0.8090169943749446757, 0.5877852522924769119 ) ) ;
#18564 = ORIENTED_EDGE ( 'NONE', *, *, #7224, .F. ) ;
#18565 = FACE_OUTER_BOUND ( 'NONE', #41800, .T. ) ;
#18566 = EDGE_CURVE ( 'NONE', #13075, #32362, #29686, .T. ) ;
#18567 = ORIENTED_EDGE ( 'NONE', *, *, #19438, .T. ) ;
#18568 = DIRECTION ( 'NONE',  ( -0.000000000000000000, -0.000000000000000000, 1.000000000000000000 ) ) ;
#18569 = AXIS2_PLACEMENT_3D ( 'NONE', #5359, #29552, #14637 ) ;
#18570 = CYLINDRICAL_SURFACE ( 'NONE', #25411, 16.00000000000000000 ) ;
#18571 = DIRECTION ( 'NONE',  ( 0.000000000000000000, -0.9510565162951566398, 0.3090169943749381809 ) ) ;
#18572 = EDGE_LOOP ( 'NONE', ( #19445, #24434, #6042, #11222 ) ) ;
#18573 = ORIENTED_EDGE ( 'NONE', *, *, #20619, .T. ) ;
#18574 = EDGE_CURVE ( 'NONE', #45301, #24474, #14074, .T. ) ;
#18575 = CARTESIAN_POINT ( 'NONE',  ( -11.99999999999999645, 0.000000000000000000, 0.000000000000000000 ) ) ;
#18576 = CARTESIAN_POINT ( 'NONE',  ( 15.00000000000000000, 23.49999999999999645, 1.499999999999995337 ) ) ;
#18577 = VECTOR ( 'NONE', #1139, 1000.000000000000114 ) ;
#18578 = ORIENTED_EDGE ( 'NONE', *, *, #48184, .F. ) ;
#18579 = VERTEX_POINT ( 'NONE', #3453 ) ;
#18580 = ADVANCED_FACE ( 'NONE', ( #25232 ), #26226, .T. ) ;
#18581 = DIRECTION ( 'NONE',  ( 0.000000000000000000, 0.000000000000000000, 1.000000000000000000 ) ) ;
#18582 = CARTESIAN_POINT ( 'NONE',  ( 4.999999999999999112, 3.925862922256769583, -41.81611651403857621 ) ) ;
#18583 = ORIENTED_EDGE ( 'NONE', *, *, #4344, .F. ) ;
#18584 = CYLINDRICAL_SURFACE ( 'NONE', #45635, 16.00000000000000000 ) ;
#18585 = FACE_OUTER_BOUND ( 'NONE', #22518, .T. ) ;
#18586 = DIRECTION ( 'NONE',  ( -1.000000000000000000, -0.000000000000000000, -0.000000000000000000 ) ) ;
#18587 = FACE_OUTER_BOUND ( 'NONE', #43971, .T. ) ;
#18588 = DIRECTION ( 'NONE',  ( -1.000000000000000000, -0.000000000000000000, 0.000000000000000000 ) ) ;
#18589 = CARTESIAN_POINT ( 'NONE',  ( 10.00000000000000000, 6.555932627142418312, 37.01155633439060466 ) ) ;
#18590 = VECTOR ( 'NONE', #42007, 1000.000000000000000 ) ;
#18591 = CARTESIAN_POINT ( 'NONE',  ( 10.00000000000000000, -16.65560815589383381, -38.55633173627028754 ) ) ;
#18592 = EDGE_CURVE ( 'NONE', #34102, #36999, #48441, .T. ) ;
#18593 = DIRECTION ( 'NONE',  ( -1.000000000000000000, 0.000000000000000000, 0.000000000000000000 ) ) ;
#18594 = LINE ( 'NONE', #14924, #30129 ) ;
#18595 = EDGE_LOOP ( 'NONE', ( #42739, #47747, #29740, #27118 ) ) ;
#18596 = CARTESIAN_POINT ( 'NONE',  ( 0.000000000000000000, 29.81001611431041098, -22.74946021919100403 ) ) ;
#18597 = FACE_OUTER_BOUND ( 'NONE', #13848, .T. ) ;
#18598 = PRESENTATION_STYLE_ASSIGNMENT (( #18353 ) ) ;
#18599 = CARTESIAN_POINT ( 'NONE',  ( 10.00000000000000000, -2.946379043145784582, -75.11764819372150725 ) ) ;
#18600 = ORIENTED_EDGE ( 'NONE', *, *, #41127, .F. ) ;
#18601 = ORIENTED_EDGE ( 'NONE', *, *, #9455, .F. ) ;
#18602 = EDGE_CURVE ( 'NONE', #441, #25278, #17663, .T. ) ;
#18603 = DIRECTION ( 'NONE',  ( -1.000000000000000000, 0.000000000000000000, 0.000000000000000000 ) ) ;
#18604 = CARTESIAN_POINT ( 'NONE',  ( -3.000000000000000000, -19.89357724624987256, -12.59942793731086041 ) ) ;
#18605 = CARTESIAN_POINT ( 'NONE',  ( 0.000000000000000000, -120.0000000000000000, 102.9091629284897493 ) ) ;
#18606 = VECTOR ( 'NONE', #38623, 1000.000000000000000 ) ;
#18607 = ORIENTED_EDGE ( 'NONE', *, *, #45144, .T. ) ;
#18608 = EDGE_CURVE ( 'NONE', #43090, #47670, #32811, .T. ) ;
#18609 = CARTESIAN_POINT ( 'NONE',  ( -3.000000000000000000, 5.835314593368477354, 22.81335362449854642 ) ) ;
#18610 = VERTEX_POINT ( 'NONE', #47998 ) ;
#18611 = ORIENTED_EDGE ( 'NONE', *, *, #24756, .F. ) ;
#18612 = ORIENTED_EDGE ( 'NONE', *, *, #47959, .F. ) ;
#18613 = EDGE_LOOP ( 'NONE', ( #17611, #31725, #27578, #26499 ) ) ;
#18614 = VERTEX_POINT ( 'NONE', #7853 ) ;
#18615 = CARTESIAN_POINT ( 'NONE',  ( 0.000000000000000000, 63.18004540533027580, 44.88180994100400056 ) ) ;
#18616 = EDGE_CURVE ( 'NONE', #31274, #10549, #38320, .T. ) ;
#18617 = CARTESIAN_POINT ( 'NONE',  ( 10.00000000000000000, -75.11764819372145041, 29.05362095685286761 ) ) ;
#18618 = EDGE_LOOP ( 'NONE', ( #12911, #38621, #18252, #14035 ) ) ;
#18619 = ADVANCED_FACE ( 'NONE', ( #41887 ), #16182, .T. ) ;
#18620 = ORIENTED_EDGE ( 'NONE', *, *, #35671, .T. ) ;
#18621 = DIRECTION ( 'NONE',  ( -1.000000000000000000, -0.000000000000000000, 0.000000000000000000 ) ) ;
#18622 = ORIENTED_EDGE ( 'NONE', *, *, #19042, .F. ) ;
#18623 = CARTESIAN_POINT ( 'NONE',  ( 0.000000000000000000, 0.000000000000000000, -44.99999999999998579 ) ) ;
#18624 = DIRECTION ( 'NONE',  ( 0.000000000000000000, 0.000000000000000000, 1.000000000000000000 ) ) ;
#18625 = CARTESIAN_POINT ( 'NONE',  ( -3.000000000000000000, -14.54903810567676636, 22.19967320028755964 ) ) ;
#18626 = CYLINDRICAL_SURFACE ( 'NONE', #2076, 31.99999999999999289 ) ;
#18627 = EDGE_LOOP ( 'NONE', ( #47946, #27956, #8200, #28816 ) ) ;
#18629 = ORIENTED_EDGE ( 'NONE', *, *, #21753, .T. ) ;
#18628 = DIRECTION ( 'NONE',  ( -1.000000000000000000, -0.000000000000000000, -0.000000000000000000 ) ) ;
#18630 = CYLINDRICAL_SURFACE ( 'NONE', #37576, 31.99999999999998579 ) ;
#18631 = ORIENTED_EDGE ( 'NONE', *, *, #41507, .T. ) ;
#18632 = DIRECTION ( 'NONE',  ( -1.000000000000000000, -0.000000000000000000, -0.000000000000000000 ) ) ;
#18633 = ORIENTED_EDGE ( 'NONE', *, *, #41076, .T. ) ;
#18634 = CARTESIAN_POINT ( 'NONE',  ( -10.00000000000000000, 0.000000000000000000, 0.000000000000000000 ) ) ;
#18635 = DIRECTION ( 'NONE',  ( -1.000000000000000000, 0.000000000000000000, -0.000000000000000000 ) ) ;
#18636 = EDGE_LOOP ( 'NONE', ( #39771, #34439, #14166, #44503 ) ) ;
#18637 = AXIS2_PLACEMENT_3D ( 'NONE', #15711, #26985, #8370 ) ;
#18638 = CARTESIAN_POINT ( 'NONE',  ( -10.00000000000000000, 0.000000000000000000, 0.000000000000000000 ) ) ;
#18639 = PLANE ( 'NONE',  #21911 ) ;
#18640 = DIRECTION ( 'NONE',  ( -1.000000000000000000, -0.000000000000000000, -0.000000000000000000 ) ) ;
#18641 = AXIS2_PLACEMENT_3D ( 'NONE', #38022, #33845, #319 ) ;
#18642 = CARTESIAN_POINT ( 'NONE',  ( 10.00000000000000000, -2.663952781846440576, 41.91543099594817789 ) ) ;
#18643 = DIRECTION ( 'NONE',  ( -0.000000000000000000, -0.9510565162951506446, -0.3090169943749562220 ) ) ;
#18644 = CARTESIAN_POINT ( 'NONE',  ( 6.000000000000000000, -80.55351364060578589, -15.33399622253569383 ) ) ;
#18645 = ORIENTED_EDGE ( 'NONE', *, *, #47091, .F. ) ;
#18646 = DIRECTION ( 'NONE',  ( -1.000000000000000000, 0.000000000000000000, 0.000000000000000000 ) ) ;
#18647 = CARTESIAN_POINT ( 'NONE',  ( -3.000000000000000000, 0.000000000000000000, 0.000000000000000000 ) ) ;
#18648 = DIRECTION ( 'NONE',  ( 1.000000000000000000, 0.000000000000000000, 0.000000000000000000 ) ) ;
#18649 = FACE_OUTER_BOUND ( 'NONE', #25588, .T. ) ;
#18650 = CARTESIAN_POINT ( 'NONE',  ( -3.000000000000000000, -1.278221433540502217, 26.51162292216071847 ) ) ;
#18651 = CARTESIAN_POINT ( 'NONE',  ( 10.00000000000000000, 10.74501242461333028, -35.92658777277499382 ) ) ;
#18652 = CARTESIAN_POINT ( 'NONE',  ( 11.99999999999999822, 55.38113227695783536, 54.21277698773694453 ) ) ;
#18653 = DIRECTION ( 'NONE',  ( 0.000000000000000000, -0.8910065241883627918, -0.4539904997395567965 ) ) ;
#18654 = ORIENTED_EDGE ( 'NONE', *, *, #9077, .T. ) ;
#18655 = AXIS2_PLACEMENT_3D ( 'NONE', #33103, #10346, #25994 ) ;
#18656 = ORIENTED_EDGE ( 'NONE', *, *, #7745, .T. ) ;
#18657 = CARTESIAN_POINT ( 'NONE',  ( 0.000000000000000000, 74.65491531819118620, -8.830959090342659579 ) ) ;
#18658 = ORIENTED_EDGE ( 'NONE', *, *, #13389, .T. ) ;
#18659 = CARTESIAN_POINT ( 'NONE',  ( 5.000000000000000000, 56.15606465355042332, -59.75363087400017292 ) ) ;
#18660 = DIRECTION ( 'NONE',  ( 1.224646799147353207E-16, 1.000000000000000000, 0.000000000000000000 ) ) ;
#18661 = VERTEX_POINT ( 'NONE', #34508 ) ;
#18662 = CARTESIAN_POINT ( 'NONE',  ( 5.000000000000000000, 27.75498641678786527, -31.52238457039571173 ) ) ;
#18663 = EDGE_LOOP ( 'NONE', ( #5386, #14218, #12802, #17929 ) ) ;
#18664 = CIRCLE ( 'NONE', #32740, 82.00000000000000000 ) ;
#18665 = ADVANCED_FACE ( 'NONE', ( #743 ), #984, .T. ) ;
#18666 = DIRECTION ( 'NONE',  ( 0.000000000000000000, -0.9510565162951566398, 0.3090169943749381809 ) ) ;
#18667 = AXIS2_PLACEMENT_3D ( 'NONE', #29565, #10233, #47443 ) ;
#18668 = ORIENTED_EDGE ( 'NONE', *, *, #34145, .T. ) ;
#18669 = EDGE_CURVE ( 'NONE', #42455, #46829, #44563, .T. ) ;
#18670 = CIRCLE ( 'NONE', #42936, 82.00000000000000000 ) ;
#18671 = CARTESIAN_POINT ( 'NONE',  ( 0.000000000000000000, 37.58145647212453611, 0.6853352020791767529 ) ) ;
#18672 = ADVANCED_FACE ( 'NONE', ( #4444 ), #34038, .T. ) ;
#18673 = DIRECTION ( 'NONE',  ( -1.000000000000000000, -0.000000000000000000, -0.000000000000000000 ) ) ;
#18674 = LINE ( 'NONE', #33373, #14455 ) ;
#18675 = ORIENTED_EDGE ( 'NONE', *, *, #3360, .T. ) ;
#18676 = EDGE_CURVE ( 'NONE', #43888, #39399, #41166, .T. ) ;
#18677 = ORIENTED_EDGE ( 'NONE', *, *, #13042, .F. ) ;
#18678 = CARTESIAN_POINT ( 'NONE',  ( -11.69999999999999929, 2.571758278209441267E-15, 20.99999999999999645 ) ) ;
#18679 = DIRECTION ( 'NONE',  ( 0.000000000000000000, 0.000000000000000000, 1.000000000000000000 ) ) ;
#18680 = DIRECTION ( 'NONE',  ( 0.000000000000000000, 0.000000000000000000, 1.000000000000000000 ) ) ;
#18681 = CARTESIAN_POINT ( 'NONE',  ( 11.99999999999999822, 65.59268652807210742, 36.72794159290264560 ) ) ;
#18682 = ORIENTED_EDGE ( 'NONE', *, *, #12220, .F. ) ;
#18683 = DIRECTION ( 'NONE',  ( 0.000000000000000000, -0.3090169943749548342, 0.9510565162951510887 ) ) ;
#18684 = ORIENTED_EDGE ( 'NONE', *, *, #27877, .F. ) ;
#18685 = ORIENTED_EDGE ( 'NONE', *, *, #27575, .T. ) ;
#18686 = DIRECTION ( 'NONE',  ( -1.000000000000000000, -0.000000000000000000, 0.000000000000000000 ) ) ;
#18687 = EDGE_CURVE ( 'NONE', #293, #47513, #6285, .T. ) ;
#18688 = DIRECTION ( 'NONE',  ( 0.000000000000000000, 0.000000000000000000, 1.000000000000000000 ) ) ;
#18689 = CARTESIAN_POINT ( 'NONE',  ( -10.00000000000000000, 0.000000000000000000, 0.000000000000000000 ) ) ;
#18690 = DIRECTION ( 'NONE',  ( 1.000000000000000000, 0.000000000000000000, -0.000000000000000000 ) ) ;
#18691 = VERTEX_POINT ( 'NONE', #4196 ) ;
#18692 = DIRECTION ( 'NONE',  ( 0.000000000000000000, -6.938893903907228378E-15, 1.000000000000000000 ) ) ;
#18693 = FACE_OUTER_BOUND ( 'NONE', #13622, .T. ) ;
#18694 = PLANE ( 'NONE',  #41487 ) ;
#18695 = LINE ( 'NONE', #47825, #28314 ) ;
#18697 = VECTOR ( 'NONE', #18142, 999.9999999999998863 ) ;
#18696 = CARTESIAN_POINT ( 'NONE',  ( 0.000000000000000000, 0.000000000000000000, 0.000000000000000000 ) ) ;
#18698 = VECTOR ( 'NONE', #42771, 1000.000000000000000 ) ;
#18699 = DIRECTION ( 'NONE',  ( 1.000000000000000000, 0.000000000000000000, 0.000000000000000000 ) ) ;
#18700 = CARTESIAN_POINT ( 'NONE',  ( 0.000000000000000000, 25.88420570971438650, -27.13269053701069566 ) ) ;
#18701 = DIRECTION ( 'NONE',  ( 0.000000000000000000, 0.000000000000000000, 1.000000000000000000 ) ) ;
#18702 = DIRECTION ( 'NONE',  ( -1.000000000000000000, 0.000000000000000000, 0.000000000000000000 ) ) ;
#18703 = CARTESIAN_POINT ( 'NONE',  ( -10.00000000000000000, 0.000000000000000000, 0.000000000000000000 ) ) ;
#18704 = DIRECTION ( 'NONE',  ( -1.000000000000000000, -0.000000000000000000, 0.000000000000000000 ) ) ;
#18705 = ADVANCED_FACE ( 'NONE', ( #18857 ), #41630, .T. ) ;
#18706 = DIRECTION ( 'NONE',  ( -0.9435911131814395114, 0.3311129884571304971, 0.000000000000000000 ) ) ;
#18707 = CARTESIAN_POINT ( 'NONE',  ( 5.000000000000002665, -8.966570791700153364, -81.50828551894237251 ) ) ;
#18708 = AXIS2_PLACEMENT_3D ( 'NONE', #45593, #34564, #11595 ) ;
#18709 = DIRECTION ( 'NONE',  ( -1.000000000000000000, 0.000000000000000000, 0.000000000000000000 ) ) ;
#18710 = DIRECTION ( 'NONE',  ( 0.000000000000000000, 0.9969173337331276308, 0.07845909572784874608 ) ) ;
#18711 = EDGE_CURVE ( 'NONE', #8199, #27843, #43798, .T. ) ;
#18712 = EDGE_CURVE ( 'NONE', #35445, #32049, #8096, .T. ) ;
#18713 = DIRECTION ( 'NONE',  ( -1.000000000000000000, 0.000000000000000000, -0.000000000000000000 ) ) ;
#18714 = ORIENTED_EDGE ( 'NONE', *, *, #29918, .T. ) ;
#18715 = VERTEX_POINT ( 'NONE', #12505 ) ;
#18716 = ORIENTED_EDGE ( 'NONE', *, *, #1786, .F. ) ;
#18717 = CARTESIAN_POINT ( 'NONE',  ( 10.00000000000000000, 75.11764819372142199, 2.946379043147685728 ) ) ;
#18718 = EDGE_CURVE ( 'NONE', #32747, #14823, #14103, .T. ) ;
#18719 = ORIENTED_EDGE ( 'NONE', *, *, #25674, .F. ) ;
#18720 = EDGE_CURVE ( 'NONE', #40415, #42450, #15934, .T. ) ;
#18721 = EDGE_CURVE ( 'NONE', #47783, #27549, #19108, .T. ) ;
#18722 = DIRECTION ( 'NONE',  ( 0.000000000000000000, 0.000000000000000000, -1.000000000000000000 ) ) ;
#18723 = VECTOR ( 'NONE', #41499, 1000.000000000000000 ) ;
#18724 = DIRECTION ( 'NONE',  ( 0.000000000000000000, -0.8090169943749402348, -0.5877852522924830181 ) ) ;
#18725 = DIRECTION ( 'NONE',  ( -1.000000000000000000, -0.000000000000000000, 0.000000000000000000 ) ) ;
#18726 = AXIS2_PLACEMENT_3D ( 'NONE', #15544, #30475, #11409 ) ;
#18727 = ORIENTED_EDGE ( 'NONE', *, *, #11828, .T. ) ;
#18728 = DIRECTION ( 'NONE',  ( -0.000000000000000000, -0.000000000000000000, -1.000000000000000000 ) ) ;
#18729 = ORIENTED_EDGE ( 'NONE', *, *, #12520, .F. ) ;
#18730 = EDGE_LOOP ( 'NONE', ( #4195, #8984, #29625, #21621 ) ) ;
#18731 =( GEOMETRIC_REPRESENTATION_CONTEXT ( 3 ) GLOBAL_UNCERTAINTY_ASSIGNED_CONTEXT ( ( #34479 ) ) GLOBAL_UNIT_ASSIGNED_CONTEXT ( ( #37118, #11183, #37847 ) ) REPRESENTATION_CONTEXT ( 'NONE', 'WORKASPACE' ) );
#18732 = DIRECTION ( 'NONE',  ( -1.000000000000000000, -0.000000000000000000, 0.000000000000000000 ) ) ;
#18733 = LINE ( 'NONE', #387, #15730 ) ;
#18734 = DIRECTION ( 'NONE',  ( -0.000000000000000000, 0.000000000000000000, 1.000000000000000000 ) ) ;
#18735 = EDGE_LOOP ( 'NONE', ( #26436, #36082, #32938, #27186 ) ) ;
#18736 = VERTEX_POINT ( 'NONE', #7621 ) ;
#18737 = AXIS2_PLACEMENT_3D ( 'NONE', #23275, #4668, #30384 ) ;
#18738 = DIRECTION ( 'NONE',  ( -1.000000000000000000, 0.000000000000000000, -0.000000000000000000 ) ) ;
#18739 = EDGE_LOOP ( 'NONE', ( #31101, #16556, #38208, #17980 ) ) ;
#18740 = DIRECTION ( 'NONE',  ( 0.000000000000000000, -0.5877852522924689183, 0.8090169943749504489 ) ) ;
#18741 = LINE ( 'NONE', #6783, #19384 ) ;
#18742 = CARTESIAN_POINT ( 'NONE',  ( 0.000000000000000000, -36.72794159290288718, 65.59268652807197952 ) ) ;
#18743 = LINE ( 'NONE', #23155, #40937 ) ;
#18744 = DIRECTION ( 'NONE',  ( -1.000000000000000000, -0.000000000000000000, 0.000000000000000000 ) ) ;
#18745 = LINE ( 'NONE', #18519, #26035 ) ;
#18746 = DIRECTION ( 'NONE',  ( 1.000000000000000000, -0.000000000000000000, -0.000000000000000000 ) ) ;
#18747 = ORIENTED_EDGE ( 'NONE', *, *, #3518, .T. ) ;
#18748 = CARTESIAN_POINT ( 'NONE',  ( 5.000000000000000000, 74.74816331893430288, 33.71516098798768013 ) ) ;
#18749 = DIRECTION ( 'NONE',  ( -0.000000000000000000, -0.000000000000000000, -1.000000000000000000 ) ) ;
#18750 = ORIENTED_EDGE ( 'NONE', *, *, #9593, .F. ) ;
#18751 = CARTESIAN_POINT ( 'NONE',  ( 0.000000000000000000, -68.55367621811110723, -44.99326035066126650 ) ) ;
#18752 = ORIENTED_EDGE ( 'NONE', *, *, #8716, .T. ) ;
#18753 = DIRECTION ( 'NONE',  ( 0.000000000000000000, 0.6494480483301849905, -0.7604059656000298206 ) ) ;
#18754 = ORIENTED_EDGE ( 'NONE', *, *, #19765, .T. ) ;
#18755 = FACE_OUTER_BOUND ( 'NONE', #9469, .T. ) ;
#18756 = CARTESIAN_POINT ( 'NONE',  ( 6.000000000000000000, 16.65972982744933972, 80.28980883073764119 ) ) ;
#18757 = DIRECTION ( 'NONE',  ( 0.5687579148473765889, -0.8225049752423776450, 0.000000000000000000 ) ) ;
#18758 = DIRECTION ( 'NONE',  ( -1.000000000000000000, -0.000000000000000000, 0.000000000000000000 ) ) ;
#18759 = VECTOR ( 'NONE', #30730, 1000.000000000000000 ) ;
#18760 = EDGE_CURVE ( 'NONE', #8790, #23605, #27195, .T. ) ;
#18761 = PLANE ( 'NONE',  #9892 ) ;
#18762 = LINE ( 'NONE', #14146, #324 ) ;
#18763 = AXIS2_PLACEMENT_3D ( 'NONE', #45902, #31460, #20413 ) ;
#18765 = EDGE_CURVE ( 'NONE', #4312, #1546, #8341, .T. ) ;
#18764 = VECTOR ( 'NONE', #26445, 1000.000000000000000 ) ;
#18766 = CARTESIAN_POINT ( 'NONE',  ( -16.06301359042743115, -102.7814171781257357, 5.500000000000000000 ) ) ;
#18767 = EDGE_CURVE ( 'NONE', #13104, #41064, #15218, .T. ) ;
#18768 = DIRECTION ( 'NONE',  ( 0.000000000000000000, 0.000000000000000000, 1.000000000000000000 ) ) ;
#18769 = PRESENTATION_LAYER_ASSIGNMENT (  '', '', ( #5505 ) ) ;
#18770 = ORIENTED_EDGE ( 'NONE', *, *, #8252, .F. ) ;
#18771 = AXIS2_PLACEMENT_3D ( 'NONE', #19408, #22611, #41700 ) ;
#18772 = CIRCLE ( 'NONE', #3935, 31.99999999999999289 ) ;
#18773 = EDGE_LOOP ( 'NONE', ( #7519, #4997, #21032, #15652 ) ) ;
#18774 = ORIENTED_EDGE ( 'NONE', *, *, #25222, .T. ) ;
#18775 = PLANE ( 'NONE',  #24161 ) ;
#18776 = CYLINDRICAL_SURFACE ( 'NONE', #47228, 31.99999999999997868 ) ;
#18777 = VERTEX_POINT ( 'NONE', #11542 ) ;
#18778 = EDGE_CURVE ( 'NONE', #32168, #13208, #17998, .T. ) ;
#18779 = EDGE_CURVE ( 'NONE', #3340, #40727, #9532, .T. ) ;
#18780 = DIRECTION ( 'NONE',  ( -1.000000000000000000, 0.000000000000000000, 0.000000000000000000 ) ) ;
#18781 = VERTEX_POINT ( 'NONE', #9785 ) ;
#18782 = ORIENTED_EDGE ( 'NONE', *, *, #39121, .F. ) ;
#18783 = DIRECTION ( 'NONE',  ( -0.8541291221503266584, 0.5200609990133008287, 0.000000000000000000 ) ) ;
#18784 = ADVANCED_FACE ( 'NONE', ( #20808 ), #35245, .F. ) ;
#18786 = EDGE_LOOP ( 'NONE', ( #26157, #16457, #41155, #16054 ) ) ;
#18785 = DIRECTION ( 'NONE',  ( -0.000000000000000000, -0.000000000000000000, -1.000000000000000000 ) ) ;
#18787 = CARTESIAN_POINT ( 'NONE',  ( 0.000000000000000000, -31.46837873494930093, -68.27212725128309501 ) ) ;
#18789 = ORIENTED_EDGE ( 'NONE', *, *, #29022, .T. ) ;
#18788 = AXIS2_PLACEMENT_3D ( 'NONE', #4486, #19390, #14539 ) ;
#18790 = LINE ( 'NONE', #30074, #48126 ) ;
#18791 = VERTEX_POINT ( 'NONE', #27933 ) ;
#18792 = ORIENTED_EDGE ( 'NONE', *, *, #22325, .T. ) ;
#18793 = LINE ( 'NONE', #33973, #46292 ) ;
#18794 = VECTOR ( 'NONE', #585, 1000.000000000000000 ) ;
#18795 = AXIS2_PLACEMENT_3D ( 'NONE', #22038, #47509, #40183 ) ;
#18796 = DIRECTION ( 'NONE',  ( -1.000000000000000000, 0.000000000000000000, 0.000000000000000000 ) ) ;
#18797 = DIRECTION ( 'NONE',  ( 0.000000000000000000, 1.000000000000000000, -9.787530781167598712E-16 ) ) ;
#18798 = ORIENTED_EDGE ( 'NONE', *, *, #39486, .F. ) ;
#18799 = VECTOR ( 'NONE', #43333, 1000.000000000000000 ) ;
#18800 = ORIENTED_EDGE ( 'NONE', *, *, #30500, .F. ) ;
#18801 = AXIS2_PLACEMENT_3D ( 'NONE', #1553, #17422, #2262 ) ;
#18802 = CARTESIAN_POINT ( 'NONE',  ( 10.00000000000000000, -68.27212725128298132, 31.46837873494953541 ) ) ;
#18803 = ORIENTED_EDGE ( 'NONE', *, *, #35205, .T. ) ;
#18804 = CIRCLE ( 'NONE', #41498, 82.00000000000000000 ) ;
#18805 = EDGE_LOOP ( 'NONE', ( #37370, #12418, #46964, #44726 ) ) ;
#18806 = DIRECTION ( 'NONE',  ( -1.000000000000000000, 0.000000000000000000, 0.000000000000000000 ) ) ;
#18807 = VERTEX_POINT ( 'NONE', #39669 ) ;
#18808 = CARTESIAN_POINT ( 'NONE',  ( -11.99999999999999645, 0.000000000000000000, 0.000000000000000000 ) ) ;
#18809 = CARTESIAN_POINT ( 'NONE',  ( 11.59999999999999787, 1.420590287010929336E-15, -43.79999999999998295 ) ) ;
#18810 = DIRECTION ( 'NONE',  ( 0.000000000000000000, 0.000000000000000000, 1.000000000000000000 ) ) ;
#18811 = CARTESIAN_POINT ( 'NONE',  ( 11.59999999999999964, -0.8299999999999999600, -1.199999999999999956 ) ) ;
#18812 = FACE_OUTER_BOUND ( 'NONE', #26763, .T. ) ;
#18813 = DIRECTION ( 'NONE',  ( -1.000000000000000000, 0.000000000000000000, 0.000000000000000000 ) ) ;
#18814 = CARTESIAN_POINT ( 'NONE',  ( -10.00000000000000000, 0.000000000000000000, 0.000000000000000000 ) ) ;
#18815 = DIRECTION ( 'NONE',  ( 0.000000000000000000, 0.000000000000000000, -1.000000000000000000 ) ) ;
#18816 = DIRECTION ( 'NONE',  ( 0.000000000000000000, -0.9238795325112906243, 0.3826834323650804559 ) ) ;
#18817 = EDGE_CURVE ( 'NONE', #43544, #46765, #17234, .T. ) ;
#18818 = DIRECTION ( 'NONE',  ( -1.000000000000000000, -0.000000000000000000, -0.000000000000000000 ) ) ;
#18819 = CARTESIAN_POINT ( 'NONE',  ( 11.99999999999999822, 2.946379043146343246, 75.11764819372150725 ) ) ;
#18820 = SURFACE_STYLE_USAGE ( .BOTH. , #3909 ) ;
#18821 = FACE_OUTER_BOUND ( 'NONE', #31449, .T. ) ;
#18822 = EDGE_CURVE ( 'NONE', #188, #46211, #25038, .T. ) ;
#18823 = ORIENTED_EDGE ( 'NONE', *, *, #35475, .F. ) ;
#18824 = CIRCLE ( 'NONE', #12593, 1.000000000000000000 ) ;
#18825 = AXIS2_PLACEMENT_3D ( 'NONE', #34207, #30538, #45466 ) ;
#18827 = EDGE_CURVE ( 'NONE', #28062, #30774, #20080, .T. ) ;
#18826 = PRODUCT_DEFINITION_CONTEXT ( 'detailed design', #30723, 'design' ) ;
#18828 = CARTESIAN_POINT ( 'NONE',  ( 0.000000000000000000, -46.21855187248673502, 62.20884554314003623 ) ) ;
#18829 = AXIS2_PLACEMENT_3D ( 'NONE', #46269, #38202, #46519 ) ;
#18830 = DIRECTION ( 'NONE',  ( -0.5000000000000039968, 0.8660254037844363761, 0.000000000000000000 ) ) ;
#18831 = CARTESIAN_POINT ( 'NONE',  ( -3.000000000000000000, -22.32062822937489344, 14.36278369418800160 ) ) ;
#18832 = ORIENTED_EDGE ( 'NONE', *, *, #29666, .T. ) ;
#18833 = VECTOR ( 'NONE', #38392, 1000.000000000000000 ) ;
#18834 = EDGE_CURVE ( 'NONE', #38214, #22715, #819, .T. ) ;
#18835 = CIRCLE ( 'NONE', #4774, 77.49899999999999523 ) ;
#18836 = ADVANCED_FACE ( 'NONE', ( #46994 ), #8810, .T. ) ;
#18837 = DIRECTION ( 'NONE',  ( 0.000000000000000000, 0.6494480483301849905, -0.7604059656000298206 ) ) ;
#18838 = VERTEX_POINT ( 'NONE', #5891 ) ;
#18839 = VERTEX_POINT ( 'NONE', #23748 ) ;
#18840 = ORIENTED_EDGE ( 'NONE', *, *, #44791, .F. ) ;
#18841 = ORIENTED_EDGE ( 'NONE', *, *, #453, .F. ) ;
#18842 = ORIENTED_EDGE ( 'NONE', *, *, #11556, .F. ) ;
#18843 = DIRECTION ( 'NONE',  ( 0.000000000000000000, 0.1564344650402243742, 0.9876883405951387696 ) ) ;
#18844 = ADVANCED_FACE ( 'NONE', ( #35734 ), #16651, .F. ) ;
#18845 = CARTESIAN_POINT ( 'NONE',  ( 0.000000000000000000, 0.000000000000000000, 0.000000000000000000 ) ) ;
#18846 = ORIENTED_EDGE ( 'NONE', *, *, #36061, .F. ) ;
#18847 = ORIENTED_EDGE ( 'NONE', *, *, #11715, .F. ) ;
#18848 = DIRECTION ( 'NONE',  ( -1.000000000000000000, -0.000000000000000000, -0.000000000000000000 ) ) ;
#18849 = ORIENTED_EDGE ( 'NONE', *, *, #41198, .T. ) ;
#18850 = CARTESIAN_POINT ( 'NONE',  ( 0.000000000000000000, 31.46837873494978055, 68.27212725128286763 ) ) ;
#18851 = DIRECTION ( 'NONE',  ( 0.000000000000000000, 0.4539904997395414754, 0.8910065241883706744 ) ) ;
#18852 = VERTEX_POINT ( 'NONE', #32076 ) ;
#18853 = DIRECTION ( 'NONE',  ( 0.000000000000000000, -0.9510565162951565288, 0.3090169943749382364 ) ) ;
#18854 = CARTESIAN_POINT ( 'NONE',  ( 0.000000000000000000, -33.71516098798793593, 74.74816331893418919 ) ) ;
#18855 = ORIENTED_EDGE ( 'NONE', *, *, #17939, .F. ) ;
#18856 = EDGE_CURVE ( 'NONE', #5626, #5369, #24272, .T. ) ;
#18858 = VERTEX_POINT ( 'NONE', #35495 ) ;
#18857 = FACE_OUTER_BOUND ( 'NONE', #27662, .T. ) ;
#18859 = DIRECTION ( 'NONE',  ( -1.000000000000000000, 0.000000000000000000, -0.000000000000000000 ) ) ;
#18860 = ORIENTED_EDGE ( 'NONE', *, *, #18217, .F. ) ;
#18861 = CARTESIAN_POINT ( 'NONE',  ( -3.000000000000000000, -23.29833615347109443, 3.418703333116492438 ) ) ;
#18862 = ORIENTED_EDGE ( 'NONE', *, *, #4499, .F. ) ;
#18863 = CARTESIAN_POINT ( 'NONE',  ( -22.53294031248082163, -134.0273518838794757, 5.500000000000000000 ) ) ;
#18864 = FACE_OUTER_BOUND ( 'NONE', #5283, .T. ) ;
#18865 = VECTOR ( 'NONE', #5768, 1000.000000000000000 ) ;
#18866 = AXIS2_PLACEMENT_3D ( 'NONE', #45723, #30799, #6532 ) ;
#18867 = CARTESIAN_POINT ( 'NONE',  ( 50.00005079999999680, 2.571758278209441661E-15, -21.00000000000000000 ) ) ;
#18868 = DIRECTION ( 'NONE',  ( 0.000000000000000000, 0.000000000000000000, -1.000000000000000000 ) ) ;
#18869 = CYLINDRICAL_SURFACE ( 'NONE', #25269, 77.49899999999999523 ) ;
#18870 = LINE ( 'NONE', #15232, #27308 ) ;
#18871 = DIRECTION ( 'NONE',  ( -1.000000000000000000, 0.000000000000000000, 0.000000000000000000 ) ) ;
#18872 = DIRECTION ( 'NONE',  ( 0.000000000000000000, 1.000000000000000000, 0.000000000000000000 ) ) ;
#18873 = VERTEX_POINT ( 'NONE', #43332 ) ;
#18874 = LINE ( 'NONE', #19365, #19988 ) ;
#18875 = DIRECTION ( 'NONE',  ( -1.000000000000000000, -0.000000000000000000, 0.000000000000000000 ) ) ;
#18876 = LINE ( 'NONE', #22570, #15442 ) ;
#18877 = CARTESIAN_POINT ( 'NONE',  ( -3.000000000000000000, -4.261787119644969479, -26.19803753235780519 ) ) ;
#18878 = EDGE_CURVE ( 'NONE', #11835, #27388, #46958, .T. ) ;
#18879 = AXIS2_PLACEMENT_3D ( 'NONE', #10567, #32585, #21801 ) ;
#18880 = EDGE_CURVE ( 'NONE', #47714, #46188, #25825, .T. ) ;
#18881 = CARTESIAN_POINT ( 'NONE',  ( 0.000000000000000000, -26.02418014898260878, -70.52718814184285634 ) ) ;
#18882 = CARTESIAN_POINT ( 'NONE',  ( 10.00000000000000000, 0.000000000000000000, 0.000000000000000000 ) ) ;
#18883 = CARTESIAN_POINT ( 'NONE',  ( 10.00000000000000000, 71.27951684758069462, -30.41916302227035729 ) ) ;
#18884 = LINE ( 'NONE', #32851, #42104 ) ;
#18885 = EDGE_CURVE ( 'NONE', #37023, #35068, #19560, .T. ) ;
#18886 = ORIENTED_EDGE ( 'NONE', *, *, #21130, .T. ) ;
#18887 = EDGE_CURVE ( 'NONE', #16528, #24990, #35210, .T. ) ;
#18888 = LINE ( 'NONE', #26735, #48046 ) ;
#18889 = ORIENTED_EDGE ( 'NONE', *, *, #30908, .F. ) ;
#18890 = EDGE_CURVE ( 'NONE', #17899, #46621, #33629, .T. ) ;
#18891 = DIRECTION ( 'NONE',  ( -0.6575728627325957421, 0.7533909544171993877, 1.230411769795008318E-16 ) ) ;
#18892 = DIRECTION ( 'NONE',  ( -0.9675294772147033928, 0.2527582060401658559, 0.000000000000000000 ) ) ;
#18893 = DIRECTION ( 'NONE',  ( 1.000000000000000000, -0.000000000000000000, -0.000000000000000000 ) ) ;
#18894 = ORIENTED_EDGE ( 'NONE', *, *, #26746, .T. ) ;
#18895 = CIRCLE ( 'NONE', #38481, 31.99999999999999645 ) ;
#18896 = VECTOR ( 'NONE', #38759, 1000.000000000000227 ) ;
#18897 = VECTOR ( 'NONE', #19567, 1000.000000000000114 ) ;
#18898 = CARTESIAN_POINT ( 'NONE',  ( 0.000000000000000000, -31.46837873494930093, -68.27212725128309501 ) ) ;
#18899 = ORIENTED_EDGE ( 'NONE', *, *, #32863, .F. ) ;
#18900 = AXIS2_PLACEMENT_3D ( 'NONE', #27087, #30281, #1379 ) ;
#18901 = EDGE_CURVE ( 'NONE', #30560, #10624, #12993, .T. ) ;
#18902 = FACE_OUTER_BOUND ( 'NONE', #27058, .T. ) ;
#18903 = CARTESIAN_POINT ( 'NONE',  ( 11.99999999999999822, 0.000000000000000000, 0.000000000000000000 ) ) ;
#18905 = VERTEX_POINT ( 'NONE', #39166 ) ;
#18904 = DIRECTION ( 'NONE',  ( -1.000000000000000000, -0.000000000000000000, -0.000000000000000000 ) ) ;
#18906 = AXIS2_PLACEMENT_3D ( 'NONE', #39662, #13699, #19289 ) ;
#18907 = ORIENTED_EDGE ( 'NONE', *, *, #44755, .F. ) ;
#18908 = EDGE_CURVE ( 'NONE', #34659, #37280, #9414, .T. ) ;
#18909 = ORIENTED_EDGE ( 'NONE', *, *, #19388, .T. ) ;
#18910 = CARTESIAN_POINT ( 'NONE',  ( 0.000000000000000000, 0.000000000000000000, 0.000000000000000000 ) ) ;
#18911 = LINE ( 'NONE', #571, #39799 ) ;
#18912 = CARTESIAN_POINT ( 'NONE',  ( 10.00000000000000000, -12.93880638057369659, 76.41127070299266677 ) ) ;
#18913 = EDGE_CURVE ( 'NONE', #47361, #39725, #47691, .T. ) ;
#18914 = CARTESIAN_POINT ( 'NONE',  ( 10.00000000000000000, 0.000000000000000000, 0.000000000000000000 ) ) ;
#18915 = VERTEX_POINT ( 'NONE', #7069 ) ;
#18916 = DIRECTION ( 'NONE',  ( -1.000000000000000000, -0.000000000000000000, 0.000000000000000000 ) ) ;
#18917 = ORIENTED_EDGE ( 'NONE', *, *, #4868, .F. ) ;
#18918 = ORIENTED_EDGE ( 'NONE', *, *, #38332, .F. ) ;
#18919 = CARTESIAN_POINT ( 'NONE',  ( 0.000000000000000000, 59.75363087400153006, -56.15606465354897381 ) ) ;
#18920 = LINE ( 'NONE', #27023, #13680 ) ;
#18921 = CARTESIAN_POINT ( 'NONE',  ( 10.00000000000000000, -5.256550761632340141, -77.32052557432847095 ) ) ;
#18922 = DIRECTION ( 'NONE',  ( -1.000000000000000000, 0.000000000000000000, -0.000000000000000000 ) ) ;
#18923 = EDGE_LOOP ( 'NONE', ( #34825, #29503, #28277, #34018 ) ) ;
#18924 = FACE_OUTER_BOUND ( 'NONE', #37865, .T. ) ;
#18925 = DIRECTION ( 'NONE',  ( 0.000000000000000000, 0.000000000000000000, 1.000000000000000000 ) ) ;
#18926 = LINE ( 'NONE', #37789, #33645 ) ;
#18927 = CIRCLE ( 'NONE', #4871, 42.00000000000000000 ) ;
#18928 = DIRECTION ( 'NONE',  ( -1.000000000000000000, -0.000000000000000000, -0.000000000000000000 ) ) ;
#18929 = FACE_OUTER_BOUND ( 'NONE', #40494, .T. ) ;
#18930 = CARTESIAN_POINT ( 'NONE',  ( 22.94323693612312454, -114.6983135802921083, -2.500000000000000000 ) ) ;
#18931 = FACE_OUTER_BOUND ( 'NONE', #29916, .T. ) ;
#18932 = DIRECTION ( 'NONE',  ( -1.000000000000000000, -0.000000000000000000, -0.000000000000000000 ) ) ;
#18933 = EDGE_CURVE ( 'NONE', #40387, #2188, #10187, .T. ) ;
#18934 = VECTOR ( 'NONE', #47463, 1000.000000000000000 ) ;
#18935 = PLANE ( 'NONE',  #36888 ) ;
#18936 = DIRECTION ( 'NONE',  ( -1.000000000000000000, 0.000000000000000000, 0.000000000000000000 ) ) ;
#18937 = EDGE_CURVE ( 'NONE', #7367, #6719, #32858, .T. ) ;
#18938 = AXIS2_PLACEMENT_3D ( 'NONE', #40616, #19063, #45024 ) ;
#18939 = CARTESIAN_POINT ( 'NONE',  ( 0.000000000000000000, -0.8299999999999999600, 0.000000000000000000 ) ) ;
#18940 = EDGE_LOOP ( 'NONE', ( #20777, #30988, #14794, #26135 ) ) ;
#18941 = DIRECTION ( 'NONE',  ( 0.000000000000000000, 0.000000000000000000, -1.000000000000000000 ) ) ;
#18942 = CARTESIAN_POINT ( 'NONE',  ( 0.000000000000000000, 0.000000000000000000, 125.0000000000000000 ) ) ;
#18943 = FACE_OUTER_BOUND ( 'NONE', #8867, .T. ) ;
#18944 = EDGE_CURVE ( 'NONE', #6258, #15099, #18772, .T. ) ;
#18945 = CARTESIAN_POINT ( 'NONE',  ( 10.00000000000000000, -55.16347631942997509, -60.67117009219195722 ) ) ;
#18946 = VECTOR ( 'NONE', #41252, 1000.000000000000000 ) ;
#18947 = EDGE_CURVE ( 'NONE', #8139, #26232, #6598, .T. ) ;
#18948 = CARTESIAN_POINT ( 'NONE',  ( 11.99999999999999822, 63.18004540533092239, -44.88180994100307686 ) ) ;
#18949 = ORIENTED_EDGE ( 'NONE', *, *, #21316, .T. ) ;
#18950 = ORIENTED_EDGE ( 'NONE', *, *, #27463, .T. ) ;
#18951 = ORIENTED_EDGE ( 'NONE', *, *, #5043, .F. ) ;
#18952 = AXIS2_PLACEMENT_3D ( 'NONE', #25184, #7317, #21533 ) ;
#18953 = CYLINDRICAL_SURFACE ( 'NONE', #13265, 32.00000000000000000 ) ;
#18954 = AXIS2_PLACEMENT_3D ( 'NONE', #3497, #34072, #41428 ) ;
#18955 = ORIENTED_EDGE ( 'NONE', *, *, #28133, .T. ) ;
#18956 = ORIENTED_EDGE ( 'NONE', *, *, #46822, .T. ) ;
#18957 = VECTOR ( 'NONE', #12113, 1000.000000000000000 ) ;
#18958 = DIRECTION ( 'NONE',  ( 0.000000000000000000, 0.000000000000000000, 1.000000000000000000 ) ) ;
#18959 = DIRECTION ( 'NONE',  ( 0.000000000000000000, 0.000000000000000000, 1.000000000000000000 ) ) ;
#18960 = AXIS2_PLACEMENT_3D ( 'NONE', #37172, #3641, #48419 ) ;
#18961 = DIRECTION ( 'NONE',  ( 0.000000000000000000, -0.9723699203976740035, -0.2334453638559160216 ) ) ;
#18962 = ORIENTED_EDGE ( 'NONE', *, *, #44754, .T. ) ;
#18963 = DIRECTION ( 'NONE',  ( 0.000000000000000000, 0.000000000000000000, 1.000000000000000000 ) ) ;
#18964 = AXIS2_PLACEMENT_3D ( 'NONE', #16127, #17065, #16841 ) ;
#18965 = VERTEX_POINT ( 'NONE', #29098 ) ;
#18966 = ORIENTED_EDGE ( 'NONE', *, *, #38974, .F. ) ;
#18967 = CIRCLE ( 'NONE', #46351, 77.49899999999999523 ) ;
#18968 = EDGE_LOOP ( 'NONE', ( #30125, #43011, #21645, #42179 ) ) ;
#18969 = CARTESIAN_POINT ( 'NONE',  ( 0.000000000000000000, 75.11764819372142199, 2.946379043147685728 ) ) ;
#18970 = CARTESIAN_POINT ( 'NONE',  ( 10.00000000000000000, 12.26510123303259725, 35.53030884539089840 ) ) ;
#18971 = LINE ( 'NONE', #33907, #15779 ) ;
#18972 = ORIENTED_EDGE ( 'NONE', *, *, #3756, .T. ) ;
#18973 = CIRCLE ( 'NONE', #28386, 31.99999999999998934 ) ;
#18974 = ORIENTED_EDGE ( 'NONE', *, *, #46054, .T. ) ;
#18975 = VERTEX_POINT ( 'NONE', #18328 ) ;
#18976 = DIRECTION ( 'NONE',  ( 0.000000000000000000, 0.000000000000000000, 1.000000000000000000 ) ) ;
#18977 = VERTEX_POINT ( 'NONE', #43795 ) ;
#18978 = CARTESIAN_POINT ( 'NONE',  ( 11.99999999999999822, 0.000000000000000000, 0.000000000000000000 ) ) ;
#18979 = VECTOR ( 'NONE', #32406, 1000.000000000000000 ) ;
#18980 = EDGE_CURVE ( 'NONE', #17592, #11314, #5512, .T. ) ;
#18981 = LINE ( 'NONE', #38572, #9993 ) ;
#18982 = LINE ( 'NONE', #29767, #15119 ) ;
#18983 = CARTESIAN_POINT ( 'NONE',  ( 0.000000000000000000, 73.72996012237460661, -14.67089635893632504 ) ) ;
#18984 = DIRECTION ( 'NONE',  ( 0.000000000000000000, 0.9969173337331281859, -0.07845909572784182107 ) ) ;
#18985 = DIRECTION ( 'NONE',  ( -1.000000000000000000, -0.000000000000000000, -0.000000000000000000 ) ) ;
#18986 = EDGE_CURVE ( 'NONE', #17380, #17289, #11763, .T. ) ;
#18987 = DIRECTION ( 'NONE',  ( -0.9918136447140100120, 0.1276937514489704939, 0.000000000000000000 ) ) ;
#18988 = SURFACE_STYLE_USAGE ( .BOTH. , #41055 ) ;
#18989 = FACE_OUTER_BOUND ( 'NONE', #7604, .T. ) ;
#18990 = ORIENTED_EDGE ( 'NONE', *, *, #45367, .F. ) ;
#18991 = PLANE ( 'NONE',  #18102 ) ;
#18992 = VERTEX_POINT ( 'NONE', #2668 ) ;
#18993 = EDGE_LOOP ( 'NONE', ( #6025, #36568, #6103, #13637 ) ) ;
#18994 = CARTESIAN_POINT ( 'NONE',  ( 15.00000000000000000, 0.000000000000000000, 0.000000000000000000 ) ) ;
#18995 = ORIENTED_EDGE ( 'NONE', *, *, #39174, .T. ) ;
#18996 = DIRECTION ( 'NONE',  ( -1.000000000000000000, -0.000000000000000000, -0.000000000000000000 ) ) ;
#18997 = DIRECTION ( 'NONE',  ( -1.000000000000000000, 0.000000000000000000, 0.000000000000000000 ) ) ;
#18998 = AXIS2_PLACEMENT_3D ( 'NONE', #20841, #21299, #2703 ) ;
#18999 = CARTESIAN_POINT ( 'NONE',  ( 0.000000000000000000, 36.88895765772633695, 6.736453364083687667 ) ) ;
#19000 = EDGE_CURVE ( 'NONE', #29208, #28374, #38359, .T. ) ;
#19001 = EDGE_CURVE ( 'NONE', #19294, #38298, #17843, .T. ) ;
#19002 = EDGE_CURVE ( 'NONE', #37684, #2082, #39132, .T. ) ;
#19003 = CIRCLE ( 'NONE', #47144, 77.49899999999999523 ) ;
#19004 = CARTESIAN_POINT ( 'NONE',  ( 0.000000000000000000, -0.8828120875903202602, 37.48860685352291000 ) ) ;
#19005 = FACE_OUTER_BOUND ( 'NONE', #40182, .T. ) ;
#19006 = CARTESIAN_POINT ( 'NONE',  ( 12.00000000000000000, 8.688484142253932063, -21.88630264137371029 ) ) ;
#19007 = EDGE_CURVE ( 'NONE', #39954, #11520, #47936, .T. ) ;
#19008 = VECTOR ( 'NONE', #25612, 1000.000000000000000 ) ;
#19009 = CIRCLE ( 'NONE', #25257, 37.49900000000000233 ) ;
#19010 = AXIS2_PLACEMENT_3D ( 'NONE', #41284, #7739, #26587 ) ;
#19011 = DIRECTION ( 'NONE',  ( -1.000000000000000000, -0.000000000000000000, -0.000000000000000000 ) ) ;
#19012 = EDGE_CURVE ( 'NONE', #1618, #38183, #10992, .T. ) ;
#19013 = FILL_AREA_STYLE_COLOUR ( '', #28005 ) ;
#19014 = AXIS2_PLACEMENT_3D ( 'NONE', #47598, #40033, #20451 ) ;
#19015 = CYLINDRICAL_SURFACE ( 'NONE', #16722, 82.00000000000000000 ) ;
#19016 = ORIENTED_EDGE ( 'NONE', *, *, #32285, .T. ) ;
#19017 = CIRCLE ( 'NONE', #26160, 31.99999999999998934 ) ;
#19018 = AXIS2_PLACEMENT_3D ( 'NONE', #41002, #25320, #48328 ) ;
#19019 = VECTOR ( 'NONE', #17366, 1000.000000000000000 ) ;
#19020 = VERTEX_POINT ( 'NONE', #6363 ) ;
#19021 = CIRCLE ( 'NONE', #17451, 82.00000000000000000 ) ;
#19022 = CARTESIAN_POINT ( 'NONE',  ( -3.702536634196095910, 8.043911037661889196, 52.00000000000002132 ) ) ;
#19023 = DIRECTION ( 'NONE',  ( -1.000000000000000000, 0.000000000000000000, -0.000000000000000000 ) ) ;
#19024 = ORIENTED_EDGE ( 'NONE', *, *, #26845, .F. ) ;
#19025 = VECTOR ( 'NONE', #9634, 1000.000000000000000 ) ;
#19026 = PLANE ( 'NONE',  #11651 ) ;
#19027 = ORIENTED_EDGE ( 'NONE', *, *, #7837, .T. ) ;
#19028 = VERTEX_POINT ( 'NONE', #21270 ) ;
#19029 = EDGE_CURVE ( 'NONE', #31653, #13885, #37551, .T. ) ;
#19030 = AXIS2_PLACEMENT_3D ( 'NONE', #945, #41849, #8308 ) ;
#19031 = DIRECTION ( 'NONE',  ( -1.000000000000000000, 0.000000000000000000, -0.000000000000000000 ) ) ;
#19032 = CARTESIAN_POINT ( 'NONE',  ( 11.99999999999999822, 46.11716303203186840, 67.80270845531904911 ) ) ;
#19033 = LINE ( 'NONE', #22711, #13401 ) ;
#19034 = EDGE_CURVE ( 'NONE', #6091, #15795, #848, .T. ) ;
#19035 = ORIENTED_EDGE ( 'NONE', *, *, #44312, .F. ) ;
#19036 = CYLINDRICAL_SURFACE ( 'NONE', #14529, 37.49900000000000233 ) ;
#19037 = VERTEX_POINT ( 'NONE', #33264 ) ;
#19038 = CYLINDRICAL_SURFACE ( 'NONE', #43943, 77.49899999999999523 ) ;
#19039 = AXIS2_PLACEMENT_3D ( 'NONE', #20688, #35854, #35624 ) ;
#19040 = CIRCLE ( 'NONE', #26070, 15.99999999999999645 ) ;
#19041 = AXIS2_PLACEMENT_3D ( 'NONE', #3613, #14876, #7537 ) ;
#19042 = EDGE_CURVE ( 'NONE', #23167, #23653, #1637, .T. ) ;
#19043 = DIRECTION ( 'NONE',  ( -1.000000000000000000, -0.000000000000000000, 0.000000000000000000 ) ) ;
#19044 = FACE_OUTER_BOUND ( 'NONE', #13916, .T. ) ;
#19045 = EDGE_CURVE ( 'NONE', #24460, #1914, #18804, .T. ) ;
#19046 = ORIENTED_EDGE ( 'NONE', *, *, #562, .T. ) ;
#19047 = ORIENTED_EDGE ( 'NONE', *, *, #39259, .F. ) ;
#19048 = DIRECTION ( 'NONE',  ( 1.000000000000000000, -0.000000000000000000, 0.000000000000000000 ) ) ;
#19049 = DIRECTION ( 'NONE',  ( 1.000000000000000000, -0.000000000000000000, -0.000000000000000000 ) ) ;
#19050 = AXIS2_PLACEMENT_3D ( 'NONE', #12312, #23792, #38245 ) ;
#19051 = AXIS2_PLACEMENT_3D ( 'NONE', #23056, #41655, #15245 ) ;
#19052 = ORIENTED_EDGE ( 'NONE', *, *, #44340, .F. ) ;
#19053 = VERTEX_POINT ( 'NONE', #13709 ) ;
#19054 = AXIS2_PLACEMENT_3D ( 'NONE', #24015, #34521, #20318 ) ;
#19055 = CARTESIAN_POINT ( 'NONE',  ( 11.99999999999999822, 2.956366410621684260, -75.11725578898465017 ) ) ;
#19056 = ORIENTED_EDGE ( 'NONE', *, *, #7535, .T. ) ;
#19057 = VECTOR ( 'NONE', #28889, 1000.000000000000000 ) ;
#19058 = CARTESIAN_POINT ( 'NONE',  ( 10.00000000000000000, -65.64334221924939072, 41.19522573413710376 ) ) ;
#19059 = DIRECTION ( 'NONE',  ( 0.000000000000000000, 0.000000000000000000, -1.000000000000000000 ) ) ;
#19060 = LINE ( 'NONE', #29365, #32924 ) ;
#19061 = LINE ( 'NONE', #37430, #37821 ) ;
#19062 = ORIENTED_EDGE ( 'NONE', *, *, #13995, .T. ) ;
#19063 = DIRECTION ( 'NONE',  ( 1.000000000000000000, 0.000000000000000000, 0.000000000000000000 ) ) ;
#19064 = CARTESIAN_POINT ( 'NONE',  ( 10.00000000000000000, 29.81001611431041098, -22.74946021919100403 ) ) ;
#19065 = AXIS2_PLACEMENT_3D ( 'NONE', #41937, #37762, #4245 ) ;
#19066 = ADVANCED_FACE ( 'NONE', ( #43566 ), #10025, .F. ) ;
#19067 = EDGE_CURVE ( 'NONE', #38490, #16837, #28978, .T. ) ;
#19068 = DIRECTION ( 'NONE',  ( 0.000000000000000000, 0.000000000000000000, -1.000000000000000000 ) ) ;
#19069 = FACE_OUTER_BOUND ( 'NONE', #40660, .T. ) ;
#19070 = DIRECTION ( 'NONE',  ( -0.02332147558787823344, -0.9997280174009349762, 0.000000000000000000 ) ) ;
#19071 = DIRECTION ( 'NONE',  ( 0.9038112904824853189, -0.4279312458752977388, 0.000000000000000000 ) ) ;
#19072 = CARTESIAN_POINT ( 'NONE',  ( 0.000000000000000000, -35.95386929396264009, 10.96151621346475658 ) ) ;
#19073 = LINE ( 'NONE', #41367, #11580 ) ;
#19074 = AXIS2_PLACEMENT_3D ( 'NONE', #1815, #46846, #27774 ) ;
#19075 = ADVANCED_FACE ( 'NONE', ( #462 ), #4614, .T. ) ;
#19076 = ORIENTED_EDGE ( 'NONE', *, *, #48196, .F. ) ;
#19077 = CIRCLE ( 'NONE', #33925, 31.99999999999998579 ) ;
#19078 = CARTESIAN_POINT ( 'NONE',  ( 0.000000000000000000, 0.000000000000000000, 0.000000000000000000 ) ) ;
#19079 = CIRCLE ( 'NONE', #17508, 16.00000000000000000 ) ;
#19080 = AXIS2_PLACEMENT_3D ( 'NONE', #18910, #34321, #26283 ) ;
#19081 = DIRECTION ( 'NONE',  ( 0.000000000000000000, 0.000000000000000000, 1.000000000000000000 ) ) ;
#19082 = DIRECTION ( 'NONE',  ( 0.000000000000000000, 0.000000000000000000, 1.000000000000000000 ) ) ;
#19083 = ORIENTED_EDGE ( 'NONE', *, *, #20661, .F. ) ;
#19084 = ORIENTED_EDGE ( 'NONE', *, *, #2220, .T. ) ;
#19085 = AXIS2_PLACEMENT_3D ( 'NONE', #22215, #3608, #18540 ) ;
#19086 = AXIS2_PLACEMENT_3D ( 'NONE', #10270, #17853, #24736 ) ;
#19087 = DIRECTION ( 'NONE',  ( -1.000000000000000000, 0.000000000000000000, 0.000000000000000000 ) ) ;
#19088 = EDGE_LOOP ( 'NONE', ( #42889, #26892, #42727, #27302 ) ) ;
#19089 = ORIENTED_EDGE ( 'NONE', *, *, #11887, .F. ) ;
#19090 = ORIENTED_EDGE ( 'NONE', *, *, #32325, .F. ) ;
#19091 = VERTEX_POINT ( 'NONE', #45480 ) ;
#19092 = EDGE_LOOP ( 'NONE', ( #30154, #28831, #510, #3627 ) ) ;
#19093 = CIRCLE ( 'NONE', #30856, 11.59999999999999787 ) ;
#19094 = CARTESIAN_POINT ( 'NONE',  ( -11.99999999999999645, 0.000000000000000000, 0.000000000000000000 ) ) ;
#19095 = EDGE_CURVE ( 'NONE', #27309, #17444, #37659, .T. ) ;
#19096 = ORIENTED_EDGE ( 'NONE', *, *, #22637, .T. ) ;
#19097 = ORIENTED_EDGE ( 'NONE', *, *, #10857, .T. ) ;
#19098 = CARTESIAN_POINT ( 'NONE',  ( 6.000000000000000000, 78.73519480814955784, 22.90783923731656557 ) ) ;
#19099 = ORIENTED_EDGE ( 'NONE', *, *, #10394, .T. ) ;
#19100 = EDGE_CURVE ( 'NONE', #35670, #8149, #692, .T. ) ;
#19101 = DIRECTION ( 'NONE',  ( -1.000000000000000000, 0.000000000000000000, 0.000000000000000000 ) ) ;
#19102 = CARTESIAN_POINT ( 'NONE',  ( 10.00000000000000000, -30.00120703465222149, 22.64427369931158296 ) ) ;
#19103 = ADVANCED_FACE ( 'NONE', ( #7566 ), #4393, .F. ) ;
#19104 = EDGE_LOOP ( 'NONE', ( #14058, #25948, #24150, #41979 ) ) ;
#19105 = MANIFOLD_SOLID_BREP ( 'CirPattern1', #10664 ) ;
#19106 = DIRECTION ( 'NONE',  ( -1.000000000000000000, 0.000000000000000000, 0.000000000000000000 ) ) ;
#19107 = ORIENTED_EDGE ( 'NONE', *, *, #9603, .F. ) ;
#19108 = LINE ( 'NONE', #521, #1601 ) ;
#19109 = AXIS2_PLACEMENT_3D ( 'NONE', #8821, #5900, #5405 ) ;
#19110 = CARTESIAN_POINT ( 'NONE',  ( -3.000000000000000000, -23.29833615347104825, -3.418703333116803744 ) ) ;
#19111 = ORIENTED_EDGE ( 'NONE', *, *, #41387, .F. ) ;
#19112 = LINE ( 'NONE', #748, #37332 ) ;
#19113 = VERTEX_POINT ( 'NONE', #15157 ) ;
#19114 = ORIENTED_EDGE ( 'NONE', *, *, #28071, .F. ) ;
#19115 = CARTESIAN_POINT ( 'NONE',  ( 12.00000000000000000, -14.54903810567644484, 22.19967320028775504 ) ) ;
#19116 = CIRCLE ( 'NONE', #26146, 16.00000000000000355 ) ;
#19117 = DIRECTION ( 'NONE',  ( 0.000000000000000000, 0.3090169943749482839, -0.9510565162951533091 ) ) ;
#19118 = ORIENTED_EDGE ( 'NONE', *, *, #34856, .F. ) ;
#19119 = CIRCLE ( 'NONE', #37887, 12.49999999999999645 ) ;
#19120 = CARTESIAN_POINT ( 'NONE',  ( 11.99999999999999822, 11.30684508768339569, 76.66974797899841576 ) ) ;
#19121 = CARTESIAN_POINT ( 'NONE',  ( 10.00000000000000000, 0.000000000000000000, 0.000000000000000000 ) ) ;
#19122 = CARTESIAN_POINT ( 'NONE',  ( -4.653126046682595884, -146.1313684676804314, 5.500000000000000000 ) ) ;
#19123 = CARTESIAN_POINT ( 'NONE',  ( 10.00000000000000000, -62.50884508063453637, 41.76106447765467777 ) ) ;
#19124 = ADVANCED_FACE ( 'NONE', ( #26894 ), #7794, .T. ) ;
#19125 = DIRECTION ( 'NONE',  ( -1.000000000000000000, 0.000000000000000000, -0.000000000000000000 ) ) ;
#19126 = EDGE_CURVE ( 'NONE', #22374, #28331, #35233, .T. ) ;
#19127 = FACE_OUTER_BOUND ( 'NONE', #44221, .T. ) ;
#19128 = ORIENTED_EDGE ( 'NONE', *, *, #46717, .T. ) ;
#19129 = VECTOR ( 'NONE', #13133, 1000.000000000000000 ) ;
#19130 = CARTESIAN_POINT ( 'NONE',  ( 10.00000000000000000, 5.202137450156907761, -37.22597642581151689 ) ) ;
#19131 = ADVANCED_FACE ( 'NONE', ( #26168 ), #8288, .T. ) ;
#19132 = DIRECTION ( 'NONE',  ( 0.000000000000000000, -0.4539904997395541875, 0.8910065241883641241 ) ) ;
#19134 = VECTOR ( 'NONE', #24563, 1000.000000000000000 ) ;
#19133 = DIRECTION ( 'NONE',  ( -0.000000000000000000, -1.000000000000000000, -0.000000000000000000 ) ) ;
#19135 = VECTOR ( 'NONE', #37723, 999.9999999999998863 ) ;
#19136 = DIRECTION ( 'NONE',  ( -1.000000000000000000, 0.000000000000000000, 0.000000000000000000 ) ) ;
#19137 = DIRECTION ( 'NONE',  ( 0.000000000000000000, 0.000000000000000000, 1.000000000000000000 ) ) ;
#19138 = DIRECTION ( 'NONE',  ( 0.000000000000000000, 0.3090169943749450088, 0.9510565162951544194 ) ) ;
#19139 = DIRECTION ( 'NONE',  ( 0.000000000000000000, -0.3090169943749573878, 0.9510565162951503115 ) ) ;
#19140 = AXIS2_PLACEMENT_3D ( 'NONE', #7736, #18515, #4071 ) ;
#19141 = ORIENTED_EDGE ( 'NONE', *, *, #23990, .F. ) ;
#19142 = EDGE_CURVE ( 'NONE', #22787, #4650, #24311, .T. ) ;
#19143 = ORIENTED_EDGE ( 'NONE', *, *, #8142, .T. ) ;
#19144 = FACE_BOUND ( 'NONE', #8507, .T. ) ;
#19145 = ORIENTED_EDGE ( 'NONE', *, *, #2127, .T. ) ;
#19146 = DIRECTION ( 'NONE',  ( -1.000000000000000000, 0.000000000000000000, 0.000000000000000000 ) ) ;
#19147 = ITEM_DEFINED_TRANSFORMATION ( 'NONE', 'NONE', #40528,  #11636 ) ;
#19148 = DIRECTION ( 'NONE',  ( 0.000000000000000000, 0.000000000000000000, 1.000000000000000000 ) ) ;
#19149 = EDGE_LOOP ( 'NONE', ( #9704, #10013, #25581, #18995 ) ) ;
#19150 = VECTOR ( 'NONE', #44654, 1000.000000000000000 ) ;
#19151 = VECTOR ( 'NONE', #10875, 1000.000000000000000 ) ;
#19152 = CARTESIAN_POINT ( 'NONE',  ( -10.00000000000000000, 0.000000000000000000, 0.000000000000000000 ) ) ;
#19153 = VERTEX_POINT ( 'NONE', #30328 ) ;
#19154 = ORIENTED_EDGE ( 'NONE', *, *, #6211, .F. ) ;
#19155 = CIRCLE ( 'NONE', #16831, 32.00000000000000000 ) ;
#19156 = CARTESIAN_POINT ( 'NONE',  ( 0.000000000000000000, -65.59268652807183742, -36.72794159290312166 ) ) ;
#19157 = CARTESIAN_POINT ( 'NONE',  ( 10.00000000000000000, -35.38097989696503021, -12.42422080174676147 ) ) ;
#19159 = EDGE_LOOP ( 'NONE', ( #3061, #43318, #28494, #29398 ) ) ;
#19158 = DIRECTION ( 'NONE',  ( -0.000000000000000000, -0.000000000000000000, -1.000000000000000000 ) ) ;
#19160 = ORIENTED_EDGE ( 'NONE', *, *, #45366, .T. ) ;
#19161 = EDGE_CURVE ( 'NONE', #44883, #29381, #26412, .T. ) ;
#19162 = CIRCLE ( 'NONE', #28545, 32.00000000000000711 ) ;
#19163 = EDGE_CURVE ( 'NONE', #3559, #10015, #45247, .T. ) ;
#19164 = CIRCLE ( 'NONE', #46548, 32.00000000000000000 ) ;
#19165 = EDGE_CURVE ( 'NONE', #21692, #35831, #32151, .T. ) ;
#19166 = CARTESIAN_POINT ( 'NONE',  ( -7.543218489614351263, -11.91259227951415056, 0.000000000000000000 ) ) ;
#19167 = CARTESIAN_POINT ( 'NONE',  ( 10.00000000000000000, 0.000000000000000000, 0.000000000000000000 ) ) ;
#19168 = DIRECTION ( 'NONE',  ( -1.000000000000000000, 0.000000000000000000, 0.000000000000000000 ) ) ;
#19169 = ADVANCED_FACE ( 'NONE', ( #26650 ), #32025, .T. ) ;
#19170 = DIRECTION ( 'NONE',  ( 1.000000000000000000, 0.000000000000000000, 0.000000000000000000 ) ) ;
#19171 = AXIS2_PLACEMENT_3D ( 'NONE', #36759, #14017, #28934 ) ;
#19172 = ORIENTED_EDGE ( 'NONE', *, *, #17712, .T. ) ;
#19173 = ADVANCED_FACE ( 'NONE', ( #34952 ), #24416, .T. ) ;
#19174 = CARTESIAN_POINT ( 'NONE',  ( 15.00000000000000000, 16.61724383029390140, 20.69703378468902955 ) ) ;
#19175 = ORIENTED_EDGE ( 'NONE', *, *, #35931, .F. ) ;
#19176 = ORIENTED_EDGE ( 'NONE', *, *, #3861, .T. ) ;
#19177 = EDGE_CURVE ( 'NONE', #3188, #12549, #13170, .T. ) ;
#19178 = DIRECTION ( 'NONE',  ( 1.000000000000000000, -0.000000000000000000, 0.000000000000000000 ) ) ;
#19179 = DIRECTION ( 'NONE',  ( -1.000000000000000000, -0.000000000000000000, -0.000000000000000000 ) ) ;
#19180 = AXIS2_PLACEMENT_3D ( 'NONE', #41125, #29604, #37927 ) ;
#19181 = CARTESIAN_POINT ( 'NONE',  ( 0.000000000000000000, 0.000000000000000000, 0.000000000000000000 ) ) ;
#19182 = CARTESIAN_POINT ( 'NONE',  ( 0.000000000000000000, -28.89263327155693517, -71.91182617369219088 ) ) ;
#19183 = VERTEX_POINT ( 'NONE', #20757 ) ;
#19184 = FACE_OUTER_BOUND ( 'NONE', #29761, .T. ) ;
#19185 = DIRECTION ( 'NONE',  ( -1.000000000000000000, -0.000000000000000000, -0.000000000000000000 ) ) ;
#19186 = CARTESIAN_POINT ( 'NONE',  ( 10.00000000000000000, -37.16516213103273714, -4.992566952385376844 ) ) ;
#19187 = LINE ( 'NONE', #342, #46314 ) ;
#19188 = AXIS2_PLACEMENT_3D ( 'NONE', #6203, #39008, #5470 ) ;
#19189 = CARTESIAN_POINT ( 'NONE',  ( 11.99999999999999822, -46.54456581323762521, -59.03342792756313884 ) ) ;
#19190 = DIRECTION ( 'NONE',  ( -0.9038112904824853189, 0.4279312458752976833, 0.000000000000000000 ) ) ;
#19191 = EDGE_CURVE ( 'NONE', #13632, #4753, #28098, .T. ) ;
#19192 = DIRECTION ( 'NONE',  ( 0.000000000000000000, -0.8090169943749433434, 0.5877852522924787992 ) ) ;
#19193 = DIRECTION ( 'NONE',  ( -1.000000000000000000, 0.000000000000000000, 0.000000000000000000 ) ) ;
#19194 = CARTESIAN_POINT ( 'NONE',  ( 0.000000000000000000, -81.50828551894234408, 8.966570791700407383 ) ) ;
#19195 = LINE ( 'NONE', #30460, #42473 ) ;
#19196 = CARTESIAN_POINT ( 'NONE',  ( 11.99999999999999822, -36.73666225445940370, 65.58780272294062286 ) ) ;
#19197 = EDGE_CURVE ( 'NONE', #9076, #42556, #35433, .T. ) ;
#19198 = ORIENTED_EDGE ( 'NONE', *, *, #25526, .T. ) ;
#19199 = AXIS2_PLACEMENT_3D ( 'NONE', #24773, #20357, #24525 ) ;
#19200 = AXIS2_PLACEMENT_3D ( 'NONE', #3752, #19562, #15672 ) ;
#19201 = CARTESIAN_POINT ( 'NONE',  ( 0.000000000000000000, -33.80338159004296017, 16.23288003029484727 ) ) ;
#19202 = DIRECTION ( 'NONE',  ( -1.000000000000000000, 0.000000000000000000, 0.000000000000000000 ) ) ;
#19203 = CARTESIAN_POINT ( 'NONE',  ( 10.00000000000000000, 75.11764819372149304, -2.946379043146603482 ) ) ;
#19204 = ORIENTED_EDGE ( 'NONE', *, *, #23210, .F. ) ;
#19205 = AXIS2_PLACEMENT_3D ( 'NONE', #28275, #20942, #9671 ) ;
#19206 = DIRECTION ( 'NONE',  ( 0.000000000000000000, 0.000000000000000000, -1.000000000000000000 ) ) ;
#19207 = EDGE_LOOP ( 'NONE', ( #21794, #42265, #3209, #33487 ) ) ;
#19208 = EDGE_CURVE ( 'NONE', #15657, #31823, #35687, .T. ) ;
#19209 = VERTEX_POINT ( 'NONE', #43029 ) ;
#19210 = AXIS2_PLACEMENT_3D ( 'NONE', #20420, #12861, #46382 ) ;
#19211 = DIRECTION ( 'NONE',  ( -1.000000000000000000, 0.000000000000000000, 0.000000000000000000 ) ) ;
#19212 = VECTOR ( 'NONE', #18704, 1000.000000000000000 ) ;
#19213 = ORIENTED_EDGE ( 'NONE', *, *, #3408, .F. ) ;
#19214 = ADVANCED_FACE ( 'NONE', ( #5838 ), #9251, .T. ) ;
#19215 = CIRCLE ( 'NONE', #5153, 31.99999999999999289 ) ;
#19216 = DIRECTION ( 'NONE',  ( 0.000000000000000000, 0.000000000000000000, 1.000000000000000000 ) ) ;
#19217 = EDGE_CURVE ( 'NONE', #25968, #46297, #12689, .T. ) ;
#19218 = CARTESIAN_POINT ( 'NONE',  ( 10.00000000000000000, -64.81221759200380461, 50.23322058963325532 ) ) ;
#19219 = CARTESIAN_POINT ( 'NONE',  ( 11.99999999999999822, -71.27951684758045303, 30.41916302227090085 ) ) ;
#19220 = ORIENTED_EDGE ( 'NONE', *, *, #35819, .T. ) ;
#19221 = LINE ( 'NONE', #26809, #35189 ) ;
#19222 = ADVANCED_FACE ( 'NONE', ( #13407 ), #28328, .T. ) ;
#19223 = EDGE_LOOP ( 'NONE', ( #23189, #13207, #14330, #12191 ) ) ;
#19224 = VERTEX_POINT ( 'NONE', #39355 ) ;
#19225 = EDGE_CURVE ( 'NONE', #4472, #20356, #36001, .T. ) ;
#19226 = CARTESIAN_POINT ( 'NONE',  ( 10.00000000000000000, 4.992566952385523393, -37.16516213103272293 ) ) ;
#19227 = CARTESIAN_POINT ( 'NONE',  ( 11.99999999999999822, 72.35432306680455383, 20.40083707023012494 ) ) ;
#19229 = EDGE_LOOP ( 'NONE', ( #20557, #28818, #25432, #19744 ) ) ;
#19228 = AXIS2_PLACEMENT_3D ( 'NONE', #44744, #7558, #37650 ) ;
#19230 = ORIENTED_EDGE ( 'NONE', *, *, #24921, .F. ) ;
#19231 = VERTEX_POINT ( 'NONE', #20500 ) ;
#19232 = ORIENTED_EDGE ( 'NONE', *, *, #46248, .F. ) ;
#19233 = DIRECTION ( 'NONE',  ( 0.000000000000000000, -0.8526401643540861830, -0.5224985647159590130 ) ) ;
#19234 = ORIENTED_EDGE ( 'NONE', *, *, #12546, .T. ) ;
#19235 = EDGE_CURVE ( 'NONE', #46809, #37478, #29793, .T. ) ;
#19236 = DIRECTION ( 'NONE',  ( 0.000000000000000000, 0.000000000000000000, 1.000000000000000000 ) ) ;
#19237 = AXIS2_PLACEMENT_3D ( 'NONE', #11851, #26775, #41707 ) ;
#19238 = CARTESIAN_POINT ( 'NONE',  ( 10.00000000000000000, 0.000000000000000000, 0.000000000000000000 ) ) ;
#19239 = FACE_OUTER_BOUND ( 'NONE', #15784, .T. ) ;
#19240 = CARTESIAN_POINT ( 'NONE',  ( 0.4966694826857007139, -118.5846133302278247, -2.500000000000000000 ) ) ;
#19241 = DIRECTION ( 'NONE',  ( 0.000000000000000000, -0.8526401643540860720, -0.5224985647159589019 ) ) ;
#19242 = CYLINDRICAL_SURFACE ( 'NONE', #42461, 16.00000000000000000 ) ;
#19243 = CARTESIAN_POINT ( 'NONE',  ( -3.000000000000000000, -10.45096189432314837, -21.10159698893440350 ) ) ;
#19244 = CARTESIAN_POINT ( 'NONE',  ( 0.000000000000000000, 37.22597642581150268, 5.202137450157037435 ) ) ;
#19245 = DIRECTION ( 'NONE',  ( 0.000000000000000000, 0.000000000000000000, 1.000000000000000000 ) ) ;
#19246 = ORIENTED_EDGE ( 'NONE', *, *, #12362, .F. ) ;
#19247 = FACE_OUTER_BOUND ( 'NONE', #34946, .T. ) ;
#19248 = EDGE_LOOP ( 'NONE', ( #22757, #4288, #12896, #20874 ) ) ;
#19249 = ORIENTED_EDGE ( 'NONE', *, *, #43215, .F. ) ;
#19250 = DIRECTION ( 'NONE',  ( -1.000000000000000000, 0.000000000000000000, -0.000000000000000000 ) ) ;
#19251 = CARTESIAN_POINT ( 'NONE',  ( 10.00000000000000000, 6.736453364084091788, -36.88895765772625879 ) ) ;
#19252 = FACE_OUTER_BOUND ( 'NONE', #42060, .T. ) ;
#19253 = CARTESIAN_POINT ( 'NONE',  ( 0.000000000000000000, 15.48615015657637883, -39.04073710021327770 ) ) ;
#19254 = VECTOR ( 'NONE', #44092, 1000.000000000000000 ) ;
#19255 = DIRECTION ( 'NONE',  ( 0.000000000000000000, -0.07845909572783056618, -0.9969173337331290741 ) ) ;
#19256 = DIRECTION ( 'NONE',  ( 0.000000000000000000, 0.000000000000000000, 1.000000000000000000 ) ) ;
#19257 = CIRCLE ( 'NONE', #10673, 16.00000000000000000 ) ;
#19258 = CARTESIAN_POINT ( 'NONE',  ( 10.00000000000000000, -55.19960302592104284, 51.03279382321070301 ) ) ;
#19259 = CARTESIAN_POINT ( 'NONE',  ( -7.468086116107294004, -12.33868914344945189, -1.199999999999999956 ) ) ;
#19260 = CARTESIAN_POINT ( 'NONE',  ( 10.00000000000000000, -77.32052557432837148, -5.256550761633697277 ) ) ;
#19261 = ORIENTED_EDGE ( 'NONE', *, *, #25279, .F. ) ;
#19262 = AXIS2_PLACEMENT_3D ( 'NONE', #4380, #41817, #19285 ) ;
#19263 = ORIENTED_EDGE ( 'NONE', *, *, #12488, .F. ) ;
#19264 = ORIENTED_EDGE ( 'NONE', *, *, #39972, .T. ) ;
#19265 = AXIS2_PLACEMENT_3D ( 'NONE', #46288, #8360, #4460 ) ;
#19266 = DIRECTION ( 'NONE',  ( 0.000000000000000000, 0.000000000000000000, -1.000000000000000000 ) ) ;
#19267 = CARTESIAN_POINT ( 'NONE',  ( 4.250000000000000000, -13.95926121303099343, -1.199999999999999956 ) ) ;
#19268 = ORIENTED_EDGE ( 'NONE', *, *, #11154, .F. ) ;
#19269 = EDGE_CURVE ( 'NONE', #36021, #43246, #14910, .T. ) ;
#19270 = VECTOR ( 'NONE', #24423, 1000.000000000000000 ) ;
#19271 = ADVANCED_FACE ( 'NONE', ( #1186 ), #9726, .T. ) ;
#19272 = DIRECTION ( 'NONE',  ( -1.000000000000000000, -0.000000000000000000, 0.000000000000000000 ) ) ;
#19273 = ORIENTED_EDGE ( 'NONE', *, *, #800, .F. ) ;
#19274 = ORIENTED_EDGE ( 'NONE', *, *, #25529, .T. ) ;
#19275 = ORIENTED_EDGE ( 'NONE', *, *, #25170, .F. ) ;
#19276 = ADVANCED_FACE ( 'NONE', ( #5348 ), #31797, .T. ) ;
#19277 =( GEOMETRIC_REPRESENTATION_CONTEXT ( 3 ) GLOBAL_UNCERTAINTY_ASSIGNED_CONTEXT ( ( #41370 ) ) GLOBAL_UNIT_ASSIGNED_CONTEXT ( ( #26605, #38593, #15110 ) ) REPRESENTATION_CONTEXT ( 'NONE', 'WORKASPACE' ) );
#19278 = CARTESIAN_POINT ( 'NONE',  ( 10.00000000000000000, 0.000000000000000000, 0.000000000000000000 ) ) ;
#19279 = ADVANCED_FACE ( 'NONE', ( #45985 ), #20262, .T. ) ;
#19281 = ORIENTED_EDGE ( 'NONE', *, *, #21673, .T. ) ;
#19280 = DIRECTION ( 'NONE',  ( 0.000000000000000000, 0.000000000000000000, 1.000000000000000000 ) ) ;
#19282 = VECTOR ( 'NONE', #10720, 1000.000000000000000 ) ;
#19283 = DIRECTION ( 'NONE',  ( 0.000000000000000000, 0.4539904997395478037, -0.8910065241883673437 ) ) ;
#19284 = ORIENTED_EDGE ( 'NONE', *, *, #20660, .T. ) ;
#19285 = DIRECTION ( 'NONE',  ( 0.000000000000000000, 0.000000000000000000, 1.000000000000000000 ) ) ;
#19286 = EDGE_LOOP ( 'NONE', ( #36252, #5324, #9898, #28303 ) ) ;
#19287 = EDGE_LOOP ( 'NONE', ( #26818, #11372, #17984, #18832 ) ) ;
#19288 = EDGE_CURVE ( 'NONE', #38732, #14493, #38647, .T. ) ;
#19289 = DIRECTION ( 'NONE',  ( 0.000000000000000000, 0.000000000000000000, 1.000000000000000000 ) ) ;
#19290 = EDGE_CURVE ( 'NONE', #38922, #21614, #33656, .T. ) ;
#19291 = DIRECTION ( 'NONE',  ( -1.000000000000000000, -0.000000000000000000, 0.000000000000000000 ) ) ;
#19292 = DIRECTION ( 'NONE',  ( 0.000000000000000000, 0.000000000000000000, 1.000000000000000000 ) ) ;
#19293 = ORIENTED_EDGE ( 'NONE', *, *, #26197, .T. ) ;
#19294 = VERTEX_POINT ( 'NONE', #48140 ) ;
#19295 = DIRECTION ( 'NONE',  ( 1.000000000000000000, -0.000000000000000000, -0.000000000000000000 ) ) ;
#19296 = CIRCLE ( 'NONE', #34143, 42.00000000000000000 ) ;
#19297 = ORIENTED_EDGE ( 'NONE', *, *, #6303, .F. ) ;
#19298 = FACE_OUTER_BOUND ( 'NONE', #19788, .T. ) ;
#19299 = ORIENTED_EDGE ( 'NONE', *, *, #46664, .F. ) ;
#19300 = CARTESIAN_POINT ( 'NONE',  ( 0.000000000000000000, 20.40083707022987625, -72.35432306680462489 ) ) ;
#19301 = DIRECTION ( 'NONE',  ( -1.000000000000000000, -0.000000000000000000, 0.000000000000000000 ) ) ;
#19302 = CIRCLE ( 'NONE', #24803, 82.00000000000000000 ) ;
#19303 = CARTESIAN_POINT ( 'NONE',  ( 0.000000000000000000, 0.000000000000000000, 0.000000000000000000 ) ) ;
#19304 = DIRECTION ( 'NONE',  ( 0.000000000000000000, 0.000000000000000000, 1.000000000000000000 ) ) ;
#19305 = DIRECTION ( 'NONE',  ( 1.000000000000000000, 0.000000000000000000, -0.000000000000000000 ) ) ;
#19306 = CARTESIAN_POINT ( 'NONE',  ( 1.459549131277868561, -120.3460004817713411, 2.500000000000000000 ) ) ;
#19307 = CARTESIAN_POINT ( 'NONE',  ( 4.999999999999999112, 40.68715046381943523, -10.41901085202036370 ) ) ;
#19308 = VECTOR ( 'NONE', #36294, 1000.000000000000114 ) ;
#19309 = DIRECTION ( 'NONE',  ( -1.000000000000000000, 0.000000000000000000, -0.000000000000000000 ) ) ;
#19310 = CYLINDRICAL_SURFACE ( 'NONE', #32467, 42.00000000000000000 ) ;
#19311 = DIRECTION ( 'NONE',  ( 0.000000000000000000, 0.000000000000000000, 1.000000000000000000 ) ) ;
#19312 = LINE ( 'NONE', #39074, #24625 ) ;
#19313 = SHAPE_REPRESENTATION_RELATIONSHIP ( 'NONE' , 'NONE' ,  #37520, #20448 ) ;
#19314 = CARTESIAN_POINT ( 'NONE',  ( 11.99999999999999822, 73.73191006444572793, -14.66109333815486515 ) ) ;
#19315 = ORIENTED_EDGE ( 'NONE', *, *, #14156, .T. ) ;
#19316 = VECTOR ( 'NONE', #38344, 1000.000000000000000 ) ;
#19317 = EDGE_CURVE ( 'NONE', #44556, #39373, #9971, .T. ) ;
#19318 = UNCERTAINTY_MEASURE_WITH_UNIT (LENGTH_MEASURE( 1.000000000000000082E-05 ), #29558, 'distance_accuracy_value', 'NONE');
#19319 = FACE_OUTER_BOUND ( 'NONE', #3799, .T. ) ;
#19320 = EDGE_CURVE ( 'NONE', #41947, #28440, #40336, .T. ) ;
#19321 = PLANE ( 'NONE',  #6527 ) ;
#19322 = DIRECTION ( 'NONE',  ( -1.000000000000000000, 0.000000000000000000, 0.000000000000000000 ) ) ;
#19323 = EDGE_CURVE ( 'NONE', #42306, #24639, #11735, .T. ) ;
#19324 = ORIENTED_EDGE ( 'NONE', *, *, #33982, .F. ) ;
#19325 = AXIS2_PLACEMENT_3D ( 'NONE', #44178, #24850, #40741 ) ;
#19326 = ORIENTED_EDGE ( 'NONE', *, *, #15467, .T. ) ;
#19327 = VECTOR ( 'NONE', #23328, 1000.000000000000114 ) ;
#19328 = CARTESIAN_POINT ( 'NONE',  ( 15.00000000000000000, 0.000000000000000000, 0.000000000000000000 ) ) ;
#19329 = VERTEX_POINT ( 'NONE', #24899 ) ;
#19330 = ORIENTED_EDGE ( 'NONE', *, *, #62, .F. ) ;
#19331 = ORIENTED_EDGE ( 'NONE', *, *, #24364, .F. ) ;
#19332 = EDGE_CURVE ( 'NONE', #38183, #32221, #3337, .T. ) ;
#19333 = ADVANCED_FACE ( 'NONE', ( #25374 ), #32723, .F. ) ;
#19334 = EDGE_CURVE ( 'NONE', #43536, #48063, #10708, .T. ) ;
#19335 = CARTESIAN_POINT ( 'NONE',  ( 0.000000000000000000, -81.90746397400386059, -3.894527615418766242 ) ) ;
#19336 = CIRCLE ( 'NONE', #29515, 82.00000000000000000 ) ;
#19337 = ORIENTED_EDGE ( 'NONE', *, *, #35614, .F. ) ;
#19338 = CARTESIAN_POINT ( 'NONE',  ( 0.000000000000000000, 44.88180994100376608, 63.18004540533043922 ) ) ;
#19339 = ORIENTED_EDGE ( 'NONE', *, *, #35044, .T. ) ;
#19340 = CARTESIAN_POINT ( 'NONE',  ( 15.00000000000000000, 5.835314593368777558, 22.81335362449846471 ) ) ;
#19341 = VERTEX_POINT ( 'NONE', #29305 ) ;
#19342 = FACE_OUTER_BOUND ( 'NONE', #12716, .T. ) ;
#19343 = CARTESIAN_POINT ( 'NONE',  ( 10.00000000000000000, -22.74946021919153694, 29.81001611431000597 ) ) ;
#19344 = ORIENTED_EDGE ( 'NONE', *, *, #22828, .T. ) ;
#19345 = DIRECTION ( 'NONE',  ( -1.000000000000000000, -0.000000000000000000, -0.000000000000000000 ) ) ;
#19346 = VERTEX_POINT ( 'NONE', #14128 ) ;
#19347 = EDGE_CURVE ( 'NONE', #8722, #15986, #28901, .T. ) ;
#19348 = AXIS2_PLACEMENT_3D ( 'NONE', #27280, #6146, #38286 ) ;
#19350 = ORIENTED_EDGE ( 'NONE', *, *, #26845, .T. ) ;
#19349 = DIRECTION ( 'NONE',  ( 0.000000000000000000, 0.000000000000000000, 1.000000000000000000 ) ) ;
#19351 = FACE_OUTER_BOUND ( 'NONE', #5455, .T. ) ;
#19352 = EDGE_LOOP ( 'NONE', ( #20579, #28157, #39360, #32998 ) ) ;
#19353 = CARTESIAN_POINT ( 'NONE',  ( -21.33958957442910886, -129.9559990355020034, 5.500000000000000000 ) ) ;
#19354 = ORIENTED_EDGE ( 'NONE', *, *, #45479, .F. ) ;
#19355 = CARTESIAN_POINT ( 'NONE',  ( -11.59999999999999787, 0.000000000000000000, -56.19999999999998863 ) ) ;
#19356 = DIRECTION ( 'NONE',  ( 0.000000000000000000, 0.000000000000000000, 1.000000000000000000 ) ) ;
#19357 = VERTEX_POINT ( 'NONE', #25615 ) ;
#19358 = DIRECTION ( 'NONE',  ( 0.000000000000000000, 0.000000000000000000, -1.000000000000000000 ) ) ;
#19359 = CARTESIAN_POINT ( 'NONE',  ( 5.000000000000000000, 41.91543099594818500, 2.663952781846291362 ) ) ;
#19360 = DIRECTION ( 'NONE',  ( -0.000000000000000000, -0.000000000000000000, -1.000000000000000000 ) ) ;
#19361 = LINE ( 'NONE', #19585, #3858 ) ;
#19362 = CARTESIAN_POINT ( 'NONE',  ( 0.000000000000000000, 33.00180498840046539, 17.80606268964551120 ) ) ;
#19363 = FACE_OUTER_BOUND ( 'NONE', #4923, .T. ) ;
#19364 = VERTEX_POINT ( 'NONE', #10206 ) ;
#19365 = CARTESIAN_POINT ( 'NONE',  ( 12.50000000000000000, -107.5000000000000000, 2.500000000000000000 ) ) ;
#19366 = DIRECTION ( 'NONE',  ( 0.000000000000000000, 0.8910065241883655673, 0.4539904997395510233 ) ) ;
#19367 = LINE ( 'NONE', #29909, #24705 ) ;
#19368 = ORIENTED_EDGE ( 'NONE', *, *, #30974, .T. ) ;
#19369 = CIRCLE ( 'NONE', #44391, 10.00000000000000178 ) ;
#19370 = DIRECTION ( 'NONE',  ( -1.000000000000000000, 0.000000000000000000, 0.000000000000000000 ) ) ;
#19371 = CARTESIAN_POINT ( 'NONE',  ( 5.999999999999999112, -55.16347631942998930, -60.67117009219195722 ) ) ;
#19373 = AXIS2_PLACEMENT_3D ( 'NONE', #45408, #26814, #18507 ) ;
#19372 = CARTESIAN_POINT ( 'NONE',  ( 10.00000000000000000, 0.000000000000000000, 0.000000000000000000 ) ) ;
#19374 = ORIENTED_EDGE ( 'NONE', *, *, #11932, .F. ) ;
#19375 = EDGE_CURVE ( 'NONE', #27608, #27838, #36150, .T. ) ;
#19376 = FACE_BOUND ( 'NONE', #37507, .T. ) ;
#19377 = ORIENTED_EDGE ( 'NONE', *, *, #22969, .T. ) ;
#19378 = LINE ( 'NONE', #778, #1009 ) ;
#19379 = EDGE_CURVE ( 'NONE', #25227, #36913, #12605, .T. ) ;
#19380 = CONTEXT_DEPENDENT_SHAPE_REPRESENTATION ( #15719, #33961 ) ;
#19381 = CYLINDRICAL_SURFACE ( 'NONE', #45575, 31.99999999999998579 ) ;
#19382 = ADVANCED_FACE ( 'NONE', ( #10456 ), #10938, .F. ) ;
#19383 = ORIENTED_EDGE ( 'NONE', *, *, #27883, .T. ) ;
#19384 = VECTOR ( 'NONE', #48132, 1000.000000000000000 ) ;
#19385 = CARTESIAN_POINT ( 'NONE',  ( -24.50849501662245800, -109.8101191361138831, 5.500000000000000000 ) ) ;
#19386 = VERTEX_POINT ( 'NONE', #40797 ) ;
#19387 = EDGE_CURVE ( 'NONE', #23803, #23034, #6253, .T. ) ;
#19388 = EDGE_CURVE ( 'NONE', #32236, #28820, #39863, .T. ) ;
#19389 = DIRECTION ( 'NONE',  ( 0.000000000000000000, 0.000000000000000000, -1.000000000000000000 ) ) ;
#19390 = DIRECTION ( 'NONE',  ( -1.000000000000000000, -0.000000000000000000, -0.000000000000000000 ) ) ;
#19392 = ORIENTED_EDGE ( 'NONE', *, *, #20722, .F. ) ;
#19391 = DIRECTION ( 'NONE',  ( -0.8225049752423776450, -0.5687579148473765889, 0.000000000000000000 ) ) ;
#19393 = VERTEX_POINT ( 'NONE', #39841 ) ;
#19394 = CIRCLE ( 'NONE', #46784, 42.00000000000000000 ) ;
#19395 = CIRCLE ( 'NONE', #9277, 77.49899999999999523 ) ;
#19396 = FACE_OUTER_BOUND ( 'NONE', #28012, .T. ) ;
#19397 = DIRECTION ( 'NONE',  ( 0.000000000000000000, 0.7071067811865487940, -0.7071067811865462405 ) ) ;
#19398 = DIRECTION ( 'NONE',  ( 0.000000000000000000, 0.000000000000000000, 1.000000000000000000 ) ) ;
#19399 = EDGE_CURVE ( 'NONE', #40287, #17719, #81, .T. ) ;
#19400 = LINE ( 'NONE', #45860, #7773 ) ;
#19401 = ORIENTED_EDGE ( 'NONE', *, *, #29513, .F. ) ;
#19402 = DIRECTION ( 'NONE',  ( -1.000000000000000000, 0.000000000000000000, -0.000000000000000000 ) ) ;
#19403 = EDGE_LOOP ( 'NONE', ( #19691, #16656, #45886, #316, #16836, #41464 ) ) ;
#19404 = ORIENTED_EDGE ( 'NONE', *, *, #330, .T. ) ;
#19405 = CARTESIAN_POINT ( 'NONE',  ( 10.00000000000000000, 0.000000000000000000, 0.000000000000000000 ) ) ;
#19406 = ORIENTED_EDGE ( 'NONE', *, *, #26188, .T. ) ;
#19407 = CARTESIAN_POINT ( 'NONE',  ( -10.00000000000000000, 0.000000000000000000, 0.000000000000000000 ) ) ;
#19408 = CARTESIAN_POINT ( 'NONE',  ( -16.06301359042743115, -102.7814171781257357, 5.500000000000000000 ) ) ;
#19409 = DIRECTION ( 'NONE',  ( -1.000000000000000000, 0.000000000000000000, 0.000000000000000000 ) ) ;
#19410 = EDGE_LOOP ( 'NONE', ( #26089, #2579, #9104, #46023, #31500, #22211 ) ) ;
#19411 = DIRECTION ( 'NONE',  ( 0.000000000000000000, -0.000000000000000000, 1.000000000000000000 ) ) ;
#19412 = CARTESIAN_POINT ( 'NONE',  ( 10.00000000000000000, 32.34446384430010113, -26.79245525562679831 ) ) ;
#19413 = CARTESIAN_POINT ( 'NONE',  ( -11.59517495878806947, -96.12423995607481686, 2.500000000000000000 ) ) ;
#19414 = FACE_OUTER_BOUND ( 'NONE', #41865, .T. ) ;
#19415 = CARTESIAN_POINT ( 'NONE',  ( 0.000000000000000000, -27.05870788708213226, -26.08949754953053102 ) ) ;
#19416 = CARTESIAN_POINT ( 'NONE',  ( 15.00000000000000000, -0.9646360437375368635, -23.52805723605589705 ) ) ;
#19417 = DIRECTION ( 'NONE',  ( 0.000000000000000000, 0.000000000000000000, 1.000000000000000000 ) ) ;
#19418 = DIRECTION ( 'NONE',  ( 0.000000000000000000, 0.000000000000000000, -1.000000000000000000 ) ) ;
#19419 = FACE_OUTER_BOUND ( 'NONE', #30729, .T. ) ;
#19420 = DIRECTION ( 'NONE',  ( 0.000000000000000000, 0.000000000000000000, 1.000000000000000000 ) ) ;
#19421 = MANIFOLD_SOLID_BREP ( 'Revolve1', #30197 ) ;
#19422 = FACE_BOUND ( 'NONE', #25719, .T. ) ;
#19423 = FACE_OUTER_BOUND ( 'NONE', #8684, .T. ) ;
#19424 = DIRECTION ( 'NONE',  ( 0.000000000000000000, 0.000000000000000000, -1.000000000000000000 ) ) ;
#19425 = CARTESIAN_POINT ( 'NONE',  ( 0.000000000000000000, 49.70050353004889132, 59.46389618801982380 ) ) ;
#19426 = VERTEX_POINT ( 'NONE', #41524 ) ;
#19428 = EDGE_CURVE ( 'NONE', #6106, #31086, #46118, .T. ) ;
#19427 = CIRCLE ( 'NONE', #2247, 16.00000000000000000 ) ;
#19429 = AXIS2_PLACEMENT_3D ( 'NONE', #30537, #7553, #23431 ) ;
#19430 = LINE ( 'NONE', #38293, #45542 ) ;
#19431 = ADVANCED_FACE ( 'NONE', ( #11906 ), #15572, .T. ) ;
#19432 = EDGE_LOOP ( 'NONE', ( #39026, #9522, #10746, #7222 ) ) ;
#19433 = ADVANCED_FACE ( 'NONE', ( #869 ), #7258, .T. ) ;
#19434 = ORIENTED_EDGE ( 'NONE', *, *, #21143, .F. ) ;
#19435 = ORIENTED_EDGE ( 'NONE', *, *, #40821, .T. ) ;
#19436 = FACE_OUTER_BOUND ( 'NONE', #43052, .T. ) ;
#19437 = ORIENTED_EDGE ( 'NONE', *, *, #33298, .T. ) ;
#19438 = EDGE_CURVE ( 'NONE', #37652, #45656, #44956, .T. ) ;
#19439 = AXIS2_PLACEMENT_3D ( 'NONE', #43354, #38964, #6144 ) ;
#19440 = CARTESIAN_POINT ( 'NONE',  ( -12.50000000000000000, -132.5000000000000000, 2.500000000000000000 ) ) ;
#19441 = VERTEX_POINT ( 'NONE', #15818 ) ;
#19442 = ADVANCED_FACE ( 'NONE', ( #44706 ), #7747, .T. ) ;
#19443 = DIRECTION ( 'NONE',  ( 1.000000000000000000, 0.000000000000000000, -0.000000000000000000 ) ) ;
#19444 = CARTESIAN_POINT ( 'NONE',  ( 6.782329983125267248, 10.49999999999999645, -125.0000000000000000 ) ) ;
#19445 = ORIENTED_EDGE ( 'NONE', *, *, #37094, .F. ) ;
#19446 = CARTESIAN_POINT ( 'NONE',  ( 11.99999999999999822, 18.89407956138257205, 75.16055320797038064 ) ) ;
#19447 = ORIENTED_EDGE ( 'NONE', *, *, #9998, .F. ) ;
#19448 = DIRECTION ( 'NONE',  ( 0.000000000000000000, -0.5224985647159560154, 0.8526401643540879594 ) ) ;
#19449 = CARTESIAN_POINT ( 'NONE',  ( 11.99999999999999822, -71.21200624218766961, -40.65526001592688488 ) ) ;
#19450 = EDGE_CURVE ( 'NONE', #4251, #2189, #18524, .T. ) ;
#19451 = VERTEX_POINT ( 'NONE', #26830 ) ;
#19452 = EDGE_LOOP ( 'NONE', ( #2732, #36308, #2464, #40139 ) ) ;
#19453 = AXIS2_PLACEMENT_3D ( 'NONE', #44016, #10238, #25887 ) ;
#19454 = CARTESIAN_POINT ( 'NONE',  ( 10.00000000000000000, -3.894527615417343824, -81.90746397400393164 ) ) ;
#19455 = ORIENTED_EDGE ( 'NONE', *, *, #33801, .T. ) ;
#19456 = CARTESIAN_POINT ( 'NONE',  ( 11.99999999999999822, 68.26794271651262136, 31.47745569255165066 ) ) ;
#19457 = AXIS2_PLACEMENT_3D ( 'NONE', #176, #11936, #44731 ) ;
#19458 = DIRECTION ( 'NONE',  ( -0.9227826878668545785, -0.3853207896976533209, 0.000000000000000000 ) ) ;
#19459 = DIRECTION ( 'NONE',  ( 0.000000000000000000, -1.000000000000000000, -1.040834085586084730E-14 ) ) ;
#19460 = CARTESIAN_POINT ( 'NONE',  ( 11.99999999999999822, -55.20638768913797634, 51.02545421589302777 ) ) ;
#19461 = CARTESIAN_POINT ( 'NONE',  ( 0.000000000000000000, 0.000000000000000000, 0.000000000000000000 ) ) ;
#19462 = DIRECTION ( 'NONE',  ( -1.000000000000000000, -0.000000000000000000, 0.000000000000000000 ) ) ;
#19463 = VECTOR ( 'NONE', #37294, 1000.000000000000000 ) ;
#19464 = FACE_OUTER_BOUND ( 'NONE', #224, .T. ) ;
#19465 = DIRECTION ( 'NONE',  ( 0.000000000000000000, 0.000000000000000000, 1.000000000000000000 ) ) ;
#19466 = VERTEX_POINT ( 'NONE', #26595 ) ;
#19467 = EDGE_CURVE ( 'NONE', #270, #41584, #26106, .T. ) ;
#19468 = LINE ( 'NONE', #4801, #4043 ) ;
#19469 = DIRECTION ( 'NONE',  ( -0.8090169943749426773, -0.5877852522924797984, 0.000000000000000000 ) ) ;
#19470 = VERTEX_POINT ( 'NONE', #3590 ) ;
#19471 = VERTEX_POINT ( 'NONE', #30503 ) ;
#19472 = DIRECTION ( 'NONE',  ( -1.000000000000000000, 0.000000000000000000, 0.000000000000000000 ) ) ;
#19473 = FACE_OUTER_BOUND ( 'NONE', #3731, .T. ) ;
#19474 = DIRECTION ( 'NONE',  ( -0.000000000000000000, -0.000000000000000000, -1.000000000000000000 ) ) ;
#19475 = FACE_OUTER_BOUND ( 'NONE', #45796, .T. ) ;
#19476 = FACE_OUTER_BOUND ( 'NONE', #15578, .T. ) ;
#19477 = DIRECTION ( 'NONE',  ( 0.000000000000000000, 0.000000000000000000, -1.000000000000000000 ) ) ;
#19478 = ORIENTED_EDGE ( 'NONE', *, *, #30462, .T. ) ;
#19479 = CARTESIAN_POINT ( 'NONE',  ( 10.00000000000000000, -9.188173127307003085, -40.98264845739760176 ) ) ;
#19480 = CARTESIAN_POINT ( 'NONE',  ( -10.00000000000000000, 0.000000000000000000, 0.000000000000000000 ) ) ;
#19481 = ADVANCED_FACE ( 'NONE', ( #41766 ), #8229, .F. ) ;
#19482 = EDGE_CURVE ( 'NONE', #40068, #47873, #4333, .T. ) ;
#19483 = DIRECTION ( 'NONE',  ( -1.000000000000000000, 0.000000000000000000, 0.000000000000000000 ) ) ;
#19484 = ORIENTED_EDGE ( 'NONE', *, *, #13965, .F. ) ;
#19485 = EDGE_CURVE ( 'NONE', #43495, #41616, #150, .T. ) ;
#19486 = ORIENTED_EDGE ( 'NONE', *, *, #43709, .F. ) ;
#19487 = AXIS2_PLACEMENT_3D ( 'NONE', #11557, #46051, #30162 ) ;
#19488 = EDGE_CURVE ( 'NONE', #39693, #22548, #33597, .T. ) ;
#19489 = ORIENTED_EDGE ( 'NONE', *, *, #44041, .F. ) ;
#19490 = AXIS2_PLACEMENT_3D ( 'NONE', #41987, #2020, #43599 ) ;
#19491 = LINE ( 'NONE', #15602, #16378 ) ;
#19492 = DIRECTION ( 'NONE',  ( 0.000000000000000000, 0.000000000000000000, 1.000000000000000000 ) ) ;
#19493 = EDGE_LOOP ( 'NONE', ( #13799, #38708, #35174, #1098 ) ) ;
#19494 = MANIFOLD_SOLID_BREP ( 'Fillet2', #41908 ) ;
#19495 = AXIS2_PLACEMENT_3D ( 'NONE', #30935, #38027, #8157 ) ;
#19496 = DIRECTION ( 'NONE',  ( -1.000000000000000000, -0.000000000000000000, -0.000000000000000000 ) ) ;
#19497 = EDGE_LOOP ( 'NONE', ( #43426, #1354, #32217, #43666 ) ) ;
#19498 = ORIENTED_EDGE ( 'NONE', *, *, #11274, .T. ) ;
#19499 = LINE ( 'NONE', #34433, #27287 ) ;
#19500 = CARTESIAN_POINT ( 'NONE',  ( 11.99999999999999822, 0.000000000000000000, 0.000000000000000000 ) ) ;
#19501 = ADVANCED_FACE ( 'NONE', ( #16788 ), #22192, .T. ) ;
#19502 = DIRECTION ( 'NONE',  ( -1.000000000000000000, 0.000000000000000000, -0.000000000000000000 ) ) ;
#19503 = VERTEX_POINT ( 'NONE', #8694 ) ;
#19504 = CARTESIAN_POINT ( 'NONE',  ( 11.99999999999999822, 10.30890764327382136, 81.34940948281339956 ) ) ;
#19505 = VERTEX_POINT ( 'NONE', #31485 ) ;
#19506 = ORIENTED_EDGE ( 'NONE', *, *, #10038, .T. ) ;
#19507 = DIRECTION ( 'NONE',  ( 1.000000000000000000, -0.000000000000000000, -0.000000000000000000 ) ) ;
#19508 = DIRECTION ( 'NONE',  ( -1.000000000000000000, -0.000000000000000000, -0.000000000000000000 ) ) ;
#19509 = VERTEX_POINT ( 'NONE', #24129 ) ;
#19510 = DIRECTION ( 'NONE',  ( 0.000000000000000000, 0.8910065241883657894, 0.4539904997395509678 ) ) ;
#19511 = CARTESIAN_POINT ( 'NONE',  ( 0.000000000000000000, -23.16143007188480496, 73.95703589263965227 ) ) ;
#19512 = ORIENTED_EDGE ( 'NONE', *, *, #41658, .T. ) ;
#19513 = ORIENTED_EDGE ( 'NONE', *, *, #25412, .T. ) ;
#19514 = CARTESIAN_POINT ( 'NONE',  ( 10.00000000000000000, 20.41045688087930898, -72.35160999960793049 ) ) ;
#19515 = CIRCLE ( 'NONE', #35952, 31.99999999999999645 ) ;
#19516 = DIRECTION ( 'NONE',  ( -0.9918136447140101231, 0.1276937514489694114, 0.000000000000000000 ) ) ;
#19517 = ORIENTED_EDGE ( 'NONE', *, *, #40656, .T. ) ;
#19518 = VECTOR ( 'NONE', #31216, 1000.000000000000000 ) ;
#19519 = DIRECTION ( 'NONE',  ( -1.000000000000000000, 0.000000000000000000, 0.000000000000000000 ) ) ;
#19520 = VERTEX_POINT ( 'NONE', #23632 ) ;
#19521 = AXIS2_PLACEMENT_3D ( 'NONE', #1467, #35946, #31831 ) ;
#19522 = DIRECTION ( 'NONE',  ( -1.000000000000000000, 0.000000000000000000, 0.000000000000000000 ) ) ;
#19523 = CARTESIAN_POINT ( 'NONE',  ( 10.00000000000000000, -55.38113227695743745, -54.21277698773734244 ) ) ;
#19524 = FACE_OUTER_BOUND ( 'NONE', #38001, .T. ) ;
#19525 = CARTESIAN_POINT ( 'NONE',  ( 10.00000000000000000, 0.000000000000000000, 0.000000000000000000 ) ) ;
#19526 = CYLINDRICAL_SURFACE ( 'NONE', #17191, 31.99999999999998579 ) ;
#19527 = CIRCLE ( 'NONE', #7838, 77.49899999999999523 ) ;
#19528 = VECTOR ( 'NONE', #27261, 1000.000000000000000 ) ;
#19529 = CARTESIAN_POINT ( 'NONE',  ( 10.00000000000000000, 72.35160999960817207, 20.41045688087850607 ) ) ;
#19530 = CARTESIAN_POINT ( 'NONE',  ( 0.000000000000000000, 0.000000000000000000, 0.000000000000000000 ) ) ;
#19531 = CIRCLE ( 'NONE', #34383, 77.49900000000000944 ) ;
#19532 = LINE ( 'NONE', #31817, #20724 ) ;
#19533 = EDGE_CURVE ( 'NONE', #18873, #22722, #4798, .T. ) ;
#19534 = DIRECTION ( 'NONE',  ( 0.000000000000000000, 0.000000000000000000, 1.000000000000000000 ) ) ;
#19535 = DIRECTION ( 'NONE',  ( 0.000000000000000000, 0.8910065241883688980, -0.4539904997395447506 ) ) ;
#19536 = EDGE_CURVE ( 'NONE', #47237, #7713, #8467, .T. ) ;
#19537 = APPLICATION_PROTOCOL_DEFINITION ( 'draft international standard', 'automotive_design', 1998, #17570 ) ;
#19538 = DIRECTION ( 'NONE',  ( 0.000000000000000000, 0.2334453638559060851, -0.9723699203976764460 ) ) ;
#19539 = VERTEX_POINT ( 'NONE', #13117 ) ;
#19540 = ORIENTED_EDGE ( 'NONE', *, *, #19572, .T. ) ;
#19541 = DIRECTION ( 'NONE',  ( -1.000000000000000000, 0.000000000000000000, -0.000000000000000000 ) ) ;
#19542 = EDGE_CURVE ( 'NONE', #3270, #21795, #7810, .T. ) ;
#19543 = ORIENTED_EDGE ( 'NONE', *, *, #19751, .T. ) ;
#19544 = EDGE_CURVE ( 'NONE', #42999, #39357, #29016, .T. ) ;
#19545 = DIRECTION ( 'NONE',  ( 1.000000000000000000, 0.000000000000000000, 0.000000000000000000 ) ) ;
#19546 = DIRECTION ( 'NONE',  ( 1.000000000000000000, -0.000000000000000000, -0.000000000000000000 ) ) ;
#19547 = VERTEX_POINT ( 'NONE', #27559 ) ;
#19548 = AXIS2_PLACEMENT_3D ( 'NONE', #1099, #41502, #27301 ) ;
#19549 = CIRCLE ( 'NONE', #43033, 77.49900000000000944 ) ;
#19550 = PLANE ( 'NONE',  #32804 ) ;
#19551 = CIRCLE ( 'NONE', #17989, 42.00000000000000000 ) ;
#19552 = CIRCLE ( 'NONE', #25817, 42.00000000000000000 ) ;
#19553 = EDGE_LOOP ( 'NONE', ( #6006, #7413, #28435, #9948 ) ) ;
#19554 = EDGE_CURVE ( 'NONE', #25578, #5318, #34895, .T. ) ;
#19555 = ORIENTED_EDGE ( 'NONE', *, *, #12780, .F. ) ;
#19556 = ORIENTED_EDGE ( 'NONE', *, *, #33368, .T. ) ;
#19557 = EDGE_LOOP ( 'NONE', ( #26560, #32815, #38203, #19097 ) ) ;
#19558 = AXIS2_PLACEMENT_3D ( 'NONE', #5396, #20307, #35246 ) ;
#19559 = DIRECTION ( 'NONE',  ( 0.7533909544171996098, 0.6575728627325955200, -7.625282249115660656E-32 ) ) ;
#19560 = CIRCLE ( 'NONE', #13343, 82.00000000000000000 ) ;
#19561 = VERTEX_POINT ( 'NONE', #38832 ) ;
#19562 = DIRECTION ( 'NONE',  ( -1.000000000000000000, 0.000000000000000000, 0.000000000000000000 ) ) ;
#19563 = VERTEX_POINT ( 'NONE', #5772 ) ;
#19564 = CARTESIAN_POINT ( 'NONE',  ( 10.00000000000000000, 0.000000000000000000, 0.000000000000000000 ) ) ;
#19565 = VERTEX_POINT ( 'NONE', #24355 ) ;
#19566 = DIRECTION ( 'NONE',  ( -1.000000000000000000, -0.000000000000000000, -0.000000000000000000 ) ) ;
#19567 = DIRECTION ( 'NONE',  ( -0.6862798483830534479, -0.7273375899149810975, 0.000000000000000000 ) ) ;
#19568 = ORIENTED_EDGE ( 'NONE', *, *, #17582, .F. ) ;
#19569 = DIRECTION ( 'NONE',  ( -1.000000000000000000, 0.000000000000000000, 0.000000000000000000 ) ) ;
#19570 = VERTEX_POINT ( 'NONE', #20690 ) ;
#19571 = CARTESIAN_POINT ( 'NONE',  ( 10.00000000000000000, -36.88895765772637247, 6.736453364083436313 ) ) ;
#19572 = EDGE_CURVE ( 'NONE', #39870, #12844, #9380, .T. ) ;
#19573 = DIRECTION ( 'NONE',  ( 0.000000000000000000, 0.000000000000000000, 1.000000000000000000 ) ) ;
#19574 = ORIENTED_EDGE ( 'NONE', *, *, #7017, .F. ) ;
#19575 = DIRECTION ( 'NONE',  ( -1.000000000000000000, 0.000000000000000000, -0.000000000000000000 ) ) ;
#19576 = VERTEX_POINT ( 'NONE', #35374 ) ;
#19577 = DIRECTION ( 'NONE',  ( -1.000000000000000000, 0.000000000000000000, 0.000000000000000000 ) ) ;
#19578 = CARTESIAN_POINT ( 'NONE',  ( -2.981742216678212820, 1.885622467846870828E-15, -15.39727592608509177 ) ) ;
#19579 = ORIENTED_EDGE ( 'NONE', *, *, #12557, .F. ) ;
#19580 = EDGE_CURVE ( 'NONE', #18007, #28886, #15642, .T. ) ;
#19581 = DIRECTION ( 'NONE',  ( 0.000000000000000000, 0.000000000000000000, 1.000000000000000000 ) ) ;
#19582 = CARTESIAN_POINT ( 'NONE',  ( 11.99999999999999822, 0.000000000000000000, 0.000000000000000000 ) ) ;
#19583 = CARTESIAN_POINT ( 'NONE',  ( -10.00000000000000000, 0.000000000000000000, 0.000000000000000000 ) ) ;
#19584 = EDGE_CURVE ( 'NONE', #23235, #6704, #42307, .T. ) ;
#19585 = CARTESIAN_POINT ( 'NONE',  ( 50.00005079999999680, 0.000000000000000000, 12.50000000000000000 ) ) ;
#19586 = DIRECTION ( 'NONE',  ( 0.000000000000000000, 0.000000000000000000, 1.000000000000000000 ) ) ;
#19588 = AXIS2_PLACEMENT_3D ( 'NONE', #30450, #22855, #3278 ) ;
#19587 = DIRECTION ( 'NONE',  ( 0.000000000000000000, 0.000000000000000000, 1.000000000000000000 ) ) ;
#19589 = AXIS2_PLACEMENT_3D ( 'NONE', #47406, #13880, #10440 ) ;
#19590 = LINE ( 'NONE', #15951, #23133 ) ;
#19591 = DIRECTION ( 'NONE',  ( 0.000000000000000000, 0.7071067811865439090, 0.7071067811865512365 ) ) ;
#19592 = CYLINDRICAL_SURFACE ( 'NONE', #45854, 31.99999999999999289 ) ;
#19593 = VERTEX_POINT ( 'NONE', #46887 ) ;
#19594 = CIRCLE ( 'NONE', #40710, 37.49900000000000944 ) ;
#19595 = AXIS2_PLACEMENT_3D ( 'NONE', #6113, #39878, #46983 ) ;
#19596 = ORIENTED_EDGE ( 'NONE', *, *, #26584, .F. ) ;
#19597 = CARTESIAN_POINT ( 'NONE',  ( 0.000000000000000000, 41.19522573413731692, 65.64334221924924861 ) ) ;
#19598 = CARTESIAN_POINT ( 'NONE',  ( 0.000000000000000000, -73.72996012237449293, 14.67089635893687571 ) ) ;
#19599 = LINE ( 'NONE', #1008, #47531 ) ;
#19600 = ADVANCED_FACE ( 'NONE', ( #13352 ), #20438, .T. ) ;
#19601 = DIRECTION ( 'NONE',  ( -1.000000000000000000, -0.000000000000000000, -0.000000000000000000 ) ) ;
#19602 = AXIS2_PLACEMENT_3D ( 'NONE', #10026, #35970, #13462 ) ;
#19603 = EDGE_CURVE ( 'NONE', #24691, #20853, #38330, .T. ) ;
#19604 = ORIENTED_EDGE ( 'NONE', *, *, #18329, .T. ) ;
#19605 = ADVANCED_FACE ( 'NONE', ( #42741 ), #34641, .T. ) ;
#19606 = AXIS2_PLACEMENT_3D ( 'NONE', #25731, #40672, #7631 ) ;
#19607 = EDGE_LOOP ( 'NONE', ( #10919, #46698, #11420, #16987 ) ) ;
#19608 = FACE_BOUND ( 'NONE', #14029, .T. ) ;
#19609 = AXIS2_PLACEMENT_3D ( 'NONE', #22496, #37420, #11717 ) ;
#19610 = VERTEX_POINT ( 'NONE', #25077 ) ;
#19611 = DIRECTION ( 'NONE',  ( 0.000000000000000000, 0.000000000000000000, 1.000000000000000000 ) ) ;
#19612 = SHAPE_DEFINITION_REPRESENTATION ( #12414, #29385 ) ;
#19613 = EDGE_CURVE ( 'NONE', #33332, #8066, #21117, .T. ) ;
#19614 = DIRECTION ( 'NONE',  ( -1.000000000000000000, -0.000000000000000000, -0.000000000000000000 ) ) ;
#19615 = ORIENTED_EDGE ( 'NONE', *, *, #5690, .F. ) ;
#19616 = PRODUCT_RELATED_PRODUCT_CATEGORY ( 'part', '', ( #40211 ) ) ;
#19617 = DIRECTION ( 'NONE',  ( 0.000000000000000000, 0.000000000000000000, 1.000000000000000000 ) ) ;
#19618 = EDGE_CURVE ( 'NONE', #39890, #12529, #48452, .T. ) ;
#19619 = ORIENTED_EDGE ( 'NONE', *, *, #42046, .T. ) ;
#19620 = AXIS2_PLACEMENT_3D ( 'NONE', #6910, #7865, #48018 ) ;
#19621 = CARTESIAN_POINT ( 'NONE',  ( 0.000000000000000000, -2.956366410620109519, -75.11725578898472122 ) ) ;
#19622 = CIRCLE ( 'NONE', #39992, 15.99999999999999822 ) ;
#19623 = CARTESIAN_POINT ( 'NONE',  ( -19.90058851926621131, -132.5883508287165853, 5.500000000000000000 ) ) ;
#19625 = EDGE_LOOP ( 'NONE', ( #43119, #40839, #35332, #10371 ) ) ;
#19624 = LINE ( 'NONE', #16231, #18358 ) ;
#19626 = AXIS2_PLACEMENT_3D ( 'NONE', #46034, #42352, #31356 ) ;
#19627 = AXIS2_PLACEMENT_3D ( 'NONE', #4377, #31531, #9236 ) ;
#19628 = ORIENTED_EDGE ( 'NONE', *, *, #146, .F. ) ;
#19629 = AXIS2_PLACEMENT_3D ( 'NONE', #23448, #8290, #15875 ) ;
#19630 = DIRECTION ( 'NONE',  ( 0.000000000000000000, 0.000000000000000000, 1.000000000000000000 ) ) ;
#19631 = DIRECTION ( 'NONE',  ( -1.000000000000000000, -0.000000000000000000, -0.000000000000000000 ) ) ;
#19632 = CARTESIAN_POINT ( 'NONE',  ( 10.00000000000000000, -62.20884554313985149, -46.21855187248698371 ) ) ;
#19634 = ORIENTED_EDGE ( 'NONE', *, *, #34742, .T. ) ;
#19633 = DIRECTION ( 'NONE',  ( -1.000000000000000000, 0.000000000000000000, 0.000000000000000000 ) ) ;
#19635 = EDGE_CURVE ( 'NONE', #25752, #18006, #35965, .T. ) ;
#19636 = VERTEX_POINT ( 'NONE', #10153 ) ;
#19637 = CARTESIAN_POINT ( 'NONE',  ( 11.99999999999999822, 68.67312586194995561, 35.91791733033500122 ) ) ;
#19638 = ORIENTED_EDGE ( 'NONE', *, *, #11724, .F. ) ;
#19639 = EDGE_LOOP ( 'NONE', ( #16166, #39261, #27858, #10319 ) ) ;
#19640 = CIRCLE ( 'NONE', #38314, 37.49900000000000233 ) ;
#19641 = DIRECTION ( 'NONE',  ( 0.000000000000000000, -0.9723699203976741146, -0.2334453638559159938 ) ) ;
#19642 = AXIS2_PLACEMENT_3D ( 'NONE', #31841, #16642, #34755 ) ;
#19643 = ADVANCED_FACE ( 'NONE', ( #47588 ), #2325, .T. ) ;
#19644 = DIRECTION ( 'NONE',  ( 1.000000000000000000, -0.000000000000000000, -0.000000000000000000 ) ) ;
#19645 = DIRECTION ( 'NONE',  ( -1.000000000000000000, -0.000000000000000000, -0.000000000000000000 ) ) ;
#19646 = CARTESIAN_POINT ( 'NONE',  ( 0.000000000000000000, 0.000000000000000000, -2.500000000000000000 ) ) ;
#19647 = ORIENTED_EDGE ( 'NONE', *, *, #26251, .T. ) ;
#19648 = DIRECTION ( 'NONE',  ( -1.000000000000000000, 0.000000000000000000, 0.000000000000000000 ) ) ;
#19649 = ADVANCED_FACE ( 'NONE', ( #28762 ), #6487, .T. ) ;
#19650 = CARTESIAN_POINT ( 'NONE',  ( -3.000000000000000000, 14.60985201121704513, 18.46759930825707841 ) ) ;
#19651 = CARTESIAN_POINT ( 'NONE',  ( 0.000000000000000000, -46.53671651293991118, 59.03961581697383565 ) ) ;
#19652 = DIRECTION ( 'NONE',  ( -1.000000000000000000, -0.000000000000000000, -0.000000000000000000 ) ) ;
#19653 = DIRECTION ( 'NONE',  ( -1.000000000000000000, 0.000000000000000000, 0.000000000000000000 ) ) ;
#19654 = CARTESIAN_POINT ( 'NONE',  ( 12.00000000000000000, -19.89357724624986545, 12.59942793731086219 ) ) ;
#19655 = CYLINDRICAL_SURFACE ( 'NONE', #12670, 31.99999999999999289 ) ;
#19656 = DIRECTION ( 'NONE',  ( 0.000000000000000000, 0.000000000000000000, 1.000000000000000000 ) ) ;
#19657 = CARTESIAN_POINT ( 'NONE',  ( 0.000000000000000000, 36.73666225445894185, 65.58780272294090707 ) ) ;
#19658 = CARTESIAN_POINT ( 'NONE',  ( 10.00000000000000000, 0.000000000000000000, 0.000000000000000000 ) ) ;
#19659 = EDGE_CURVE ( 'NONE', #14587, #37445, #36768, .T. ) ;
#19660 = VERTEX_POINT ( 'NONE', #17740 ) ;
#19661 = EDGE_CURVE ( 'NONE', #14617, #35941, #28989, .T. ) ;
#19662 = VERTEX_POINT ( 'NONE', #39555 ) ;
#19663 = FACE_OUTER_BOUND ( 'NONE', #30505, .T. ) ;
#19664 = DIRECTION ( 'NONE',  ( 1.000000000000000000, 0.000000000000000000, -0.000000000000000000 ) ) ;
#19665 = AXIS2_PLACEMENT_3D ( 'NONE', #42905, #31418, #4721 ) ;
#19666 = ORIENTED_EDGE ( 'NONE', *, *, #4100, .T. ) ;
#19667 = ORIENTED_EDGE ( 'NONE', *, *, #12819, .T. ) ;
#19668 = AXIS2_PLACEMENT_3D ( 'NONE', #25229, #6411, #40191 ) ;
#19669 = AXIS2_PLACEMENT_3D ( 'NONE', #45374, #8178, #38047 ) ;
#19670 = DIRECTION ( 'NONE',  ( -1.000000000000000000, -0.000000000000000000, 0.000000000000000000 ) ) ;
#19671 = AXIS2_PLACEMENT_3D ( 'NONE', #25796, #17968, #29246 ) ;
#19672 = ORIENTED_EDGE ( 'NONE', *, *, #26993, .F. ) ;
#19673 = EDGE_CURVE ( 'NONE', #41636, #199, #27390, .T. ) ;
#19674 = ORIENTED_EDGE ( 'NONE', *, *, #16256, .F. ) ;
#19675 = AXIS2_PLACEMENT_3D ( 'NONE', #37902, #15148, #41337 ) ;
#19676 = ORIENTED_EDGE ( 'NONE', *, *, #16514, .F. ) ;
#19677 = ORIENTED_EDGE ( 'NONE', *, *, #41564, .F. ) ;
#19678 = FACE_OUTER_BOUND ( 'NONE', #7381, .T. ) ;
#19679 = DIRECTION ( 'NONE',  ( 1.000000000000000000, 0.000000000000000000, 0.000000000000000000 ) ) ;
#19680 = DIRECTION ( 'NONE',  ( 0.000000000000000000, 0.000000000000000000, 1.000000000000000000 ) ) ;
#19681 = VERTEX_POINT ( 'NONE', #20938 ) ;
#19682 = CARTESIAN_POINT ( 'NONE',  ( -11.59999999999999787, 0.000000000000000000, 53.20000000000001705 ) ) ;
#19683 = ORIENTED_EDGE ( 'NONE', *, *, #44385, .F. ) ;
#19684 = ORIENTED_EDGE ( 'NONE', *, *, #17855, .F. ) ;
#19685 = ORIENTED_EDGE ( 'NONE', *, *, #26329, .F. ) ;
#19686 = DIRECTION ( 'NONE',  ( 0.000000000000000000, -0.8090169943749426773, 0.5877852522924796874 ) ) ;
#19687 = CARTESIAN_POINT ( 'NONE',  ( -10.00000000000000000, 0.000000000000000000, 0.000000000000000000 ) ) ;
#19688 = CARTESIAN_POINT ( 'NONE',  ( 9.984461079971730157, -95.40710393340120277, -5.500000000000000000 ) ) ;
#19689 = CIRCLE ( 'NONE', #5638, 32.00000000000000000 ) ;
#19690 = EDGE_LOOP ( 'NONE', ( #39116, #1367, #12718, #33132 ) ) ;
#19691 = ORIENTED_EDGE ( 'NONE', *, *, #7995, .T. ) ;
#19692 = CARTESIAN_POINT ( 'NONE',  ( 0.000000000000000000, -66.50666863321973210, -39.78640506895674633 ) ) ;
#19693 = ORIENTED_EDGE ( 'NONE', *, *, #13450, .F. ) ;
#19694 = AXIS2_PLACEMENT_3D ( 'NONE', #31354, #27432, #46267 ) ;
#19695 = CARTESIAN_POINT ( 'NONE',  ( 11.99999999999999822, 0.000000000000000000, 0.000000000000000000 ) ) ;
#19696 = EDGE_CURVE ( 'NONE', #2616, #14712, #24844, .T. ) ;
#19697 = DIRECTION ( 'NONE',  ( 0.000000000000000000, 0.000000000000000000, -1.000000000000000000 ) ) ;
#19698 = CARTESIAN_POINT ( 'NONE',  ( 10.00000000000000000, -73.72996012237449293, 14.67089635893687571 ) ) ;
#19699 = DIRECTION ( 'NONE',  ( -1.000000000000000000, -0.000000000000000000, -0.000000000000000000 ) ) ;
#19700 = DIRECTION ( 'NONE',  ( -1.000000000000000000, -0.000000000000000000, 0.000000000000000000 ) ) ;
#19701 = CARTESIAN_POINT ( 'NONE',  ( 0.000000000000000000, 0.000000000000000000, 0.000000000000000000 ) ) ;
#19702 = EDGE_CURVE ( 'NONE', #25280, #39350, #36098, .T. ) ;
#19703 = AXIS2_PLACEMENT_3D ( 'NONE', #406, #1123, #45675 ) ;
#19704 = CARTESIAN_POINT ( 'NONE',  ( 0.000000000000000000, 29.01471420065674423, -76.69515212745984911 ) ) ;
#19705 = DIRECTION ( 'NONE',  ( -0.000000000000000000, 0.4067366430758000417, -0.9135454576426009776 ) ) ;
#19706 = CARTESIAN_POINT ( 'NONE',  ( 5.000000000000000000, 46.11716303203284184, -67.80270845531839541 ) ) ;
#19707 = CARTESIAN_POINT ( 'NONE',  ( -3.000000000000000000, 16.83928648764923253, 16.46020748918050458 ) ) ;
#19708 = DIRECTION ( 'NONE',  ( 1.000000000000000000, 0.000000000000000000, -0.000000000000000000 ) ) ;
#19709 = VERTEX_POINT ( 'NONE', #28527 ) ;
#19710 = CARTESIAN_POINT ( 'NONE',  ( 10.00000000000000000, -51.02545421589363883, 55.20638768913742922 ) ) ;
#19711 = VECTOR ( 'NONE', #17037, 1000.000000000000114 ) ;
#19712 = DIRECTION ( 'NONE',  ( 1.000000000000000000, -0.000000000000000000, -0.000000000000000000 ) ) ;
#19713 = DIRECTION ( 'NONE',  ( 0.000000000000000000, -0.9945218953682730678, -0.1045284632676570791 ) ) ;
#19714 = DIRECTION ( 'NONE',  ( -0.9730327541852497042, 0.2306669878475623159, 0.000000000000000000 ) ) ;
#19715 = EDGE_CURVE ( 'NONE', #26495, #15657, #785, .T. ) ;
#19716 = ADVANCED_FACE ( 'NONE', ( #34804 ), #42400, .T. ) ;
#19717 = CARTESIAN_POINT ( 'NONE',  ( 0.000000000000000000, 0.000000000000000000, 0.000000000000000000 ) ) ;
#19718 = CARTESIAN_POINT ( 'NONE',  ( 0.000000000000000000, 0.000000000000000000, 0.000000000000000000 ) ) ;
#19719 = DIRECTION ( 'NONE',  ( 0.000000000000000000, -0.2334453638558922628, -0.9723699203976798877 ) ) ;
#19720 = CARTESIAN_POINT ( 'NONE',  ( 11.99999999999999822, -68.27212725128254078, -31.46837873495049465 ) ) ;
#19721 = EDGE_CURVE ( 'NONE', #16137, #37878, #16451, .T. ) ;
#19722 = ORIENTED_EDGE ( 'NONE', *, *, #45098, .T. ) ;
#19723 = ORIENTED_EDGE ( 'NONE', *, *, #16317, .F. ) ;
#19724 = CARTESIAN_POINT ( 'NONE',  ( -3.360000000000002096, 0.000000000000000000, -21.00000000000000000 ) ) ;
#19725 = VERTEX_POINT ( 'NONE', #35539 ) ;
#19726 = AXIS2_PLACEMENT_3D ( 'NONE', #2060, #39983, #6441 ) ;
#19727 = EDGE_CURVE ( 'NONE', #17845, #9989, #43791, .T. ) ;
#19728 = CIRCLE ( 'NONE', #2543, 77.49900000000000944 ) ;
#19729 = CIRCLE ( 'NONE', #26001, 37.49900000000001654 ) ;
#19730 = CIRCLE ( 'NONE', #6481, 31.99999999999999289 ) ;
#19731 = CARTESIAN_POINT ( 'NONE',  ( -14.87942725330654348, -141.9795960975983178, 5.500000000000000000 ) ) ;
#19732 = ORIENTED_EDGE ( 'NONE', *, *, #38834, .T. ) ;
#19733 = AXIS2_PLACEMENT_3D ( 'NONE', #38042, #7690, #22617 ) ;
#19734 = MANIFOLD_SOLID_BREP ( 'Cut-Extrude-Thin1', #25490 ) ;
#19735 = ORIENTED_EDGE ( 'NONE', *, *, #39417, .T. ) ;
#19736 = AXIS2_PLACEMENT_3D ( 'NONE', #37545, #10650, #11380 ) ;
#19737 = DIRECTION ( 'NONE',  ( -1.000000000000000000, 0.000000000000000000, 0.000000000000000000 ) ) ;
#19738 = AXIS2_PLACEMENT_3D ( 'NONE', #33115, #48284, #7166 ) ;
#19739 = DIRECTION ( 'NONE',  ( 0.000000000000000000, 0.000000000000000000, 1.000000000000000000 ) ) ;
#19740 = ORIENTED_EDGE ( 'NONE', *, *, #41984, .T. ) ;
#19741 = ORIENTED_EDGE ( 'NONE', *, *, #10966, .T. ) ;
#19742 = CARTESIAN_POINT ( 'NONE',  ( -12.49999999999999645, 0.000000000000000000, 52.00000000000002132 ) ) ;
#19744 = ORIENTED_EDGE ( 'NONE', *, *, #38689, .T. ) ;
#19743 = CARTESIAN_POINT ( 'NONE',  ( 0.000000000000000000, 32.34446384430010113, -26.79245525562679831 ) ) ;
#19745 = CARTESIAN_POINT ( 'NONE',  ( 10.00000000000000000, 17.67226234102874116, -33.17418723428288274 ) ) ;
#19746 = ORIENTED_EDGE ( 'NONE', *, *, #19288, .T. ) ;
#19747 = VERTEX_POINT ( 'NONE', #16698 ) ;
#19748 = CARTESIAN_POINT ( 'NONE',  ( -7.543218489614351263, -11.91259227951415056, -1.199999999999999956 ) ) ;
#19749 = ORIENTED_EDGE ( 'NONE', *, *, #45586, .T. ) ;
#19750 = ORIENTED_EDGE ( 'NONE', *, *, #15015, .T. ) ;
#19751 = EDGE_CURVE ( 'NONE', #7167, #44170, #28947, .T. ) ;
#19752 = DIRECTION ( 'NONE',  ( -1.000000000000000000, -0.000000000000000000, 0.000000000000000000 ) ) ;
#19753 = CARTESIAN_POINT ( 'NONE',  ( 10.00000000000000000, -31.52238457039580055, -27.75498641678775869 ) ) ;
#19754 = ORIENTED_EDGE ( 'NONE', *, *, #43384, .F. ) ;
#19755 = EDGE_CURVE ( 'NONE', #23468, #11531, #40645, .T. ) ;
#19756 = CARTESIAN_POINT ( 'NONE',  ( 10.00000000000000000, 0.000000000000000000, 0.000000000000000000 ) ) ;
#19757 = DIRECTION ( 'NONE',  ( -1.000000000000000000, 0.000000000000000000, 0.000000000000000000 ) ) ;
#19758 = AXIS2_PLACEMENT_3D ( 'NONE', #4701, #45565, #19611 ) ;
#19759 = DIRECTION ( 'NONE',  ( 0.000000000000000000, 0.2079116908177664758, 0.9781476007338042455 ) ) ;
#19760 = EDGE_LOOP ( 'NONE', ( #10481, #9754, #4648, #17983 ) ) ;
#19761 = EDGE_CURVE ( 'NONE', #42120, #43790, #29715, .T. ) ;
#19762 = ORIENTED_EDGE ( 'NONE', *, *, #18556, .F. ) ;
#19763 = CIRCLE ( 'NONE', #6506, 31.99999999999998224 ) ;
#19764 = DIRECTION ( 'NONE',  ( 0.000000000000000000, 0.000000000000000000, 1.000000000000000000 ) ) ;
#19765 = EDGE_CURVE ( 'NONE', #26327, #17279, #9574, .T. ) ;
#19766 = CARTESIAN_POINT ( 'NONE',  ( 5.999999999999999112, 74.74816331893477184, -33.71516098798660011 ) ) ;
#19768 = EDGE_CURVE ( 'NONE', #43334, #41271, #19527, .T. ) ;
#19767 = EDGE_LOOP ( 'NONE', ( #36780, #47666, #8487, #7308 ) ) ;
#19769 = EDGE_CURVE ( 'NONE', #3739, #17824, #12540, .T. ) ;
#19770 = DIRECTION ( 'NONE',  ( -1.000000000000000000, 0.000000000000000000, 0.000000000000000000 ) ) ;
#19771 = ORIENTED_EDGE ( 'NONE', *, *, #31691, .T. ) ;
#19772 = VECTOR ( 'NONE', #31735, 1000.000000000000000 ) ;
#19773 = CIRCLE ( 'NONE', #12774, 12.50000000000000000 ) ;
#19774 = CARTESIAN_POINT ( 'NONE',  ( 0.000000000000000000, 46.21855187248628738, 62.20884554314034887 ) ) ;
#19775 = DIRECTION ( 'NONE',  ( -1.000000000000000000, -0.000000000000000000, -0.000000000000000000 ) ) ;
#19776 = DIRECTION ( 'NONE',  ( -1.000000000000000000, -0.000000000000000000, -0.000000000000000000 ) ) ;
#19777 = ORIENTED_EDGE ( 'NONE', *, *, #35148, .F. ) ;
#19778 = DIRECTION ( 'NONE',  ( -1.000000000000000000, -0.000000000000000000, 0.000000000000000000 ) ) ;
#19779 = AXIS2_PLACEMENT_3D ( 'NONE', #45750, #12229, #27154 ) ;
#19780 = LINE ( 'NONE', #48270, #2679 ) ;
#19781 = CARTESIAN_POINT ( 'NONE',  ( 0.000000000000000000, 0.000000000000000000, 0.000000000000000000 ) ) ;
#19782 = AXIS2_PLACEMENT_3D ( 'NONE', #29242, #48318, #44172 ) ;
#19783 = CARTESIAN_POINT ( 'NONE',  ( 0.000000000000000000, 46.11716303203284184, -67.80270845531839541 ) ) ;
#19784 = CARTESIAN_POINT ( 'NONE',  ( 11.99999999999999822, -70.53064760720336324, 26.01480285779810231 ) ) ;
#19785 = CIRCLE ( 'NONE', #249, 16.00000000000000000 ) ;
#19786 = DIRECTION ( 'NONE',  ( -1.000000000000000000, 0.000000000000000000, 0.000000000000000000 ) ) ;
#19787 = AXIS2_PLACEMENT_3D ( 'NONE', #11094, #17713, #39767 ) ;
#19788 = EDGE_LOOP ( 'NONE', ( #23533, #19615, #20899, #13447 ) ) ;
#19789 = EDGE_LOOP ( 'NONE', ( #37543, #32625, #3926, #3519 ) ) ;
#19790 = EDGE_CURVE ( 'NONE', #828, #24345, #47035, .T. ) ;
#19791 = DIRECTION ( 'NONE',  ( 0.000000000000000000, 0.000000000000000000, -1.000000000000000000 ) ) ;
#19792 = ORIENTED_EDGE ( 'NONE', *, *, #25945, .T. ) ;
#19793 = CARTESIAN_POINT ( 'NONE',  ( -0.9515373497862389396, -96.47140937769621871, 5.500000000000000000 ) ) ;
#19794 = EDGE_CURVE ( 'NONE', #7344, #39808, #27723, .T. ) ;
#19795 = LINE ( 'NONE', #28124, #47198 ) ;
#19796 = ORIENTED_EDGE ( 'NONE', *, *, #45881, .F. ) ;
#19797 = ADVANCED_FACE ( 'NONE', ( #24047 ), #1293, .T. ) ;
#19798 = DIRECTION ( 'NONE',  ( 0.000000000000000000, 0.4067366430758010409, 0.9135454576426005335 ) ) ;
#19799 = AXIS2_PLACEMENT_3D ( 'NONE', #26296, #3276, #11122 ) ;
#19800 = CIRCLE ( 'NONE', #33890, 82.00000000000000000 ) ;
#19801 = ORIENTED_EDGE ( 'NONE', *, *, #1164, .F. ) ;
#19802 = ORIENTED_EDGE ( 'NONE', *, *, #27039, .F. ) ;
#19803 = ORIENTED_EDGE ( 'NONE', *, *, #32807, .T. ) ;
#19804 = PRODUCT_DEFINITION_SHAPE ( 'NONE', 'NONE',  #22354 ) ;
#19805 = EDGE_CURVE ( 'NONE', #44934, #34735, #38980, .T. ) ;
#19806 = DIRECTION ( 'NONE',  ( 0.000000000000000000, 0.000000000000000000, -1.000000000000000000 ) ) ;
#19807 = AXIS2_PLACEMENT_3D ( 'NONE', #1941, #17568, #20518 ) ;
#19808 = AXIS2_PLACEMENT_3D ( 'NONE', #12351, #45884, #34122 ) ;
#19809 = EDGE_LOOP ( 'NONE', ( #18424, #30258, #8791, #30415 ) ) ;
#19810 = DIRECTION ( 'NONE',  ( -1.000000000000000000, -0.000000000000000000, 0.000000000000000000 ) ) ;
#19811 = ORIENTED_EDGE ( 'NONE', *, *, #3643, .F. ) ;
#19812 = VECTOR ( 'NONE', #23759, 1000.000000000000000 ) ;
#19813 = EDGE_CURVE ( 'NONE', #45628, #45301, #10960, .T. ) ;
#19814 = DIRECTION ( 'NONE',  ( -1.000000000000000000, -0.000000000000000000, 0.000000000000000000 ) ) ;
#19815 = CIRCLE ( 'NONE', #42520, 37.49900000000000233 ) ;
#19816 = CARTESIAN_POINT ( 'NONE',  ( 12.00000000000000000, -26.23277895567245466, 4.042438405570107030 ) ) ;
#19817 = ADVANCED_FACE ( 'NONE', ( #25703 ), #28900, .T. ) ;
#19818 = FACE_OUTER_BOUND ( 'NONE', #156, .T. ) ;
#19820 = VERTEX_POINT ( 'NONE', #3439 ) ;
#19819 = CIRCLE ( 'NONE', #13586, 77.49899999999999523 ) ;
#19821 = CARTESIAN_POINT ( 'NONE',  ( 0.000000000000000000, -75.54627589209931671, -17.28742895386162814 ) ) ;
#19822 = VERTEX_POINT ( 'NONE', #10297 ) ;
#19823 = DIRECTION ( 'NONE',  ( 0.000000000000000000, -0.9876883405951393247, 0.1564344650402204329 ) ) ;
#19824 = CARTESIAN_POINT ( 'NONE',  ( 0.000000000000000000, 0.000000000000000000, 0.000000000000000000 ) ) ;
#19825 = ORIENTED_EDGE ( 'NONE', *, *, #44312, .T. ) ;
#19826 = DIRECTION ( 'NONE',  ( 1.000000000000000000, 0.000000000000000000, 0.000000000000000000 ) ) ;
#19827 = ORIENTED_EDGE ( 'NONE', *, *, #48180, .F. ) ;
#19828 = EDGE_LOOP ( 'NONE', ( #46435, #41758, #32289, #547, #13712, #3825, #30058, #36887, #6536, #30876, #35606, #19925, #2131, #37107, #30804, #43247, #3301, #42757, #20305, #45295, #43701, #12301, #6770, #15387, #4945, #7596, #4910, #7213, #40161, #44306, #20467, #40913, #18369, #31784, #42661, #4655, #26405, #44683, #45768, #3195, #42932, #8035, #31955, #45401, #1481, #29084, #27664, #45119, #5493, #2665, #20618, #13438, #47989, #34248, #34004, #25203, #2483, #17352, #9890, #21219, #15282, #34883, #21932, #29706, #19762, #45899, #16053, #47364, #30929, #24788, #45244, #12453, #2147, #33949, #38409, #24181, #33589, #18677, #13371, #22967, #5872, #23013, #15101, #11171, #27344, #23783, #43922, #40670, #43053, #9392, #32160, #39661, #17281, #25394, #13406, #5480, #29956, #24240, #14206, #31888, #32117, #21626, #41570, #25913, #18716, #42343, #12917, #34325, #16726, #38502, #20510, #6240, #83, #3955, #31530, #22012, #10157, #31907, #14350, #33015, #8978, #44147, #18065, #3705, #305, #3649, #15822, #17125, #28086, #9773, #24904, #35275, #29107, #15921, #379, #37082, #35811, #30544, #43432, #24340, #36672, #26695, #39967, #27149, #20598, #22299, #42790, #42513, #11014, #26446, #32055, #5400, #21716, #38336, #22532, #32059, #28532, #4297, #30732, #7538, #6443, #4594, #27605, #30234, #39422 ) ) ;
#19829 = EDGE_CURVE ( 'NONE', #35109, #22493, #43003, .T. ) ;
#19830 = DIRECTION ( 'NONE',  ( -1.000000000000000000, -0.000000000000000000, -0.000000000000000000 ) ) ;
#19831 = DIRECTION ( 'NONE',  ( -1.000000000000000000, 0.000000000000000000, -0.000000000000000000 ) ) ;
#19832 = ORIENTED_EDGE ( 'NONE', *, *, #20947, .F. ) ;
#19833 = CYLINDRICAL_SURFACE ( 'NONE', #11305, 21.00000000000000000 ) ;
#19834 = DIRECTION ( 'NONE',  ( -1.000000000000000000, 0.000000000000000000, -0.000000000000000000 ) ) ;
#19835 = DIRECTION ( 'NONE',  ( 0.000000000000000000, 0.000000000000000000, 1.000000000000000000 ) ) ;
#19836 = DIRECTION ( 'NONE',  ( 0.000000000000000000, 0.000000000000000000, -1.000000000000000000 ) ) ;
#19837 = CARTESIAN_POINT ( 'NONE',  ( -18.12185313557660038, -104.9634299478706794, 5.500000000000000000 ) ) ;
#19838 = CIRCLE ( 'NONE', #5783, 16.00000000000000000 ) ;
#19839 = LINE ( 'NONE', #45548, #39633 ) ;
#19840 = CIRCLE ( 'NONE', #36267, 77.49899999999999523 ) ;
#19841 = CARTESIAN_POINT ( 'NONE',  ( 10.00000000000000000, 81.90746397400388901, 3.894527615418187150 ) ) ;
#19842 = CARTESIAN_POINT ( 'NONE',  ( 11.99999999999999822, -55.16347631943085617, 60.67117009219116852 ) ) ;
#19843 = CARTESIAN_POINT ( 'NONE',  ( 0.000000000000000000, 32.34446384430010113, -26.79245525562679831 ) ) ;
#19844 = CIRCLE ( 'NONE', #25327, 31.99999999999998579 ) ;
#19845 = AXIS2_PLACEMENT_3D ( 'NONE', #20432, #20934, #35852 ) ;
#19846 = AXIS2_PLACEMENT_3D ( 'NONE', #11624, #11395, #1076 ) ;
#19847 = CARTESIAN_POINT ( 'NONE',  ( 10.00000000000000000, 9.188173127307898369, -40.98264845739739570 ) ) ;
#19848 = DIRECTION ( 'NONE',  ( -0.2079116908177587875, 0.000000000000000000, 0.9781476007338056888 ) ) ;
#19849 = SURFACE_SIDE_STYLE ('',( #12764 ) ) ;
#19850 = CARTESIAN_POINT ( 'NONE',  ( -3.000000000000000000, 9.615535125379096826, -24.73947219025905042 ) ) ;
#19851 = VERTEX_POINT ( 'NONE', #18374 ) ;
#19852 = ORIENTED_EDGE ( 'NONE', *, *, #35136, .T. ) ;
#19854 = CARTESIAN_POINT ( 'NONE',  ( -12.00000000000000000, 0.000000000000000000, 0.000000000000000000 ) ) ;
#19853 = CIRCLE ( 'NONE', #46469, 82.00000000000000000 ) ;
#19855 = CIRCLE ( 'NONE', #11277, 31.99999999999999645 ) ;
#19856 = ORIENTED_EDGE ( 'NONE', *, *, #18712, .T. ) ;
#19857 = CIRCLE ( 'NONE', #47226, 82.00000000000000000 ) ;
#19858 = CARTESIAN_POINT ( 'NONE',  ( 5.000000000000000000, 56.15606465354959198, 59.75363087400094741 ) ) ;
#19859 = CONTEXT_DEPENDENT_SHAPE_REPRESENTATION ( #31686, #11699 ) ;
#19860 = CARTESIAN_POINT ( 'NONE',  ( 12.49999999999999645, 1.530808498934191127E-15, 125.0000000000000000 ) ) ;
#19861 = ORIENTED_EDGE ( 'NONE', *, *, #25526, .F. ) ;
#19862 = ADVANCED_FACE ( 'NONE', ( #14714 ), #33306, .T. ) ;
#19863 = DIRECTION ( 'NONE',  ( 0.9435911131814402886, -0.3311129884571281101, 0.000000000000000000 ) ) ;
#19864 = ORIENTED_EDGE ( 'NONE', *, *, #26075, .T. ) ;
#19865 = CARTESIAN_POINT ( 'NONE',  ( 11.99999999999999822, 0.000000000000000000, 0.000000000000000000 ) ) ;
#19866 = AXIS2_PLACEMENT_3D ( 'NONE', #4400, #19301, #26904 ) ;
#19867 = DIRECTION ( 'NONE',  ( -1.000000000000000000, 0.000000000000000000, 0.000000000000000000 ) ) ;
#19868 = CARTESIAN_POINT ( 'NONE',  ( 0.000000000000000000, 59.46389618801963195, 49.70050353004911159 ) ) ;
#19869 = ORIENTED_EDGE ( 'NONE', *, *, #5429, .F. ) ;
#19870 = VECTOR ( 'NONE', #4052, 1000.000000000000000 ) ;
#19871 = FACE_OUTER_BOUND ( 'NONE', #34899, .T. ) ;
#19872 = CIRCLE ( 'NONE', #40239, 42.00000000000000000 ) ;
#19873 = ORIENTED_EDGE ( 'NONE', *, *, #45946, .T. ) ;
#19874 = AXIS2_PLACEMENT_3D ( 'NONE', #44633, #11105, #40974 ) ;
#19875 = ADVANCED_FACE ( 'NONE', ( #14471 ), #18118, .T. ) ;
#19876 = DIRECTION ( 'NONE',  ( -1.000000000000000000, -0.000000000000000000, -0.000000000000000000 ) ) ;
#19877 = ADVANCED_FACE ( 'NONE', ( #43603 ), #36723, .F. ) ;
#19878 = CARTESIAN_POINT ( 'NONE',  ( 0.000000000000000000, -5.256550761633411284, 77.32052557432838569 ) ) ;
#19879 = CARTESIAN_POINT ( 'NONE',  ( 15.00000000000000000, 23.49999999999999645, 1.499999999999995337 ) ) ;
#19880 = CARTESIAN_POINT ( 'NONE',  ( 0.000000000000000000, -2.543863470248944214, 81.96053171279901051 ) ) ;
#19881 = ADVANCED_FACE ( 'NONE', ( #21074 ), #10068, .T. ) ;
#19883 = ORIENTED_EDGE ( 'NONE', *, *, #20226, .T. ) ;
#19882 = FACE_OUTER_BOUND ( 'NONE', #11928, .T. ) ;
#19884 = AXIS2_PLACEMENT_3D ( 'NONE', #47401, #1902, #43245 ) ;
#19885 = CIRCLE ( 'NONE', #2700, 37.49900000000000944 ) ;
#19886 = VERTEX_POINT ( 'NONE', #9827 ) ;
#19887 = CYLINDRICAL_SURFACE ( 'NONE', #32616, 16.00000000000000000 ) ;
#19888 = ORIENTED_EDGE ( 'NONE', *, *, #45625, .T. ) ;
#19889 = ORIENTED_EDGE ( 'NONE', *, *, #41491, .T. ) ;
#19890 = CIRCLE ( 'NONE', #47269, 16.00000000000000000 ) ;
#19891 = EDGE_CURVE ( 'NONE', #44730, #3690, #43069, .T. ) ;
#19892 = CARTESIAN_POINT ( 'NONE',  ( 11.99999999999999822, 0.000000000000000000, 0.000000000000000000 ) ) ;
#19893 = CIRCLE ( 'NONE', #8854, 82.00000000000000000 ) ;
#19894 = ORIENTED_EDGE ( 'NONE', *, *, #20381, .F. ) ;
#19895 = LINE ( 'NONE', #41698, #24643 ) ;
#19896 = VECTOR ( 'NONE', #9792, 1000.000000000000000 ) ;
#19897 = EDGE_CURVE ( 'NONE', #18083, #10970, #24766, .T. ) ;
#19898 = LINE ( 'NONE', #31674, #19528 ) ;
#19899 = CARTESIAN_POINT ( 'NONE',  ( 10.00000000000000000, 35.47612816024523141, 22.48208911017513145 ) ) ;
#19900 = ORIENTED_EDGE ( 'NONE', *, *, #42827, .F. ) ;
#19901 = DIRECTION ( 'NONE',  ( 1.000000000000000000, -0.000000000000000000, 0.000000000000000000 ) ) ;
#19902 = AXIS2_PLACEMENT_3D ( 'NONE', #18978, #48367, #22664 ) ;
#19903 = DIRECTION ( 'NONE',  ( -1.000000000000000000, 0.000000000000000000, 0.000000000000000000 ) ) ;
#19904 = DIRECTION ( 'NONE',  ( -1.000000000000000000, -0.000000000000000000, -0.000000000000000000 ) ) ;
#19905 = DIRECTION ( 'NONE',  ( -0.000000000000000000, -0.000000000000000000, 1.000000000000000000 ) ) ;
#19906 = DIRECTION ( 'NONE',  ( -1.000000000000000000, 0.000000000000000000, -0.000000000000000000 ) ) ;
#19907 = CARTESIAN_POINT ( 'NONE',  ( 10.00000000000000000, -59.46389618801928378, -49.70050353004953791 ) ) ;
#19908 = CARTESIAN_POINT ( 'NONE',  ( 12.00000000000000000, 24.81905959214260804, -9.408202855044827118 ) ) ;
#19909 = EDGE_CURVE ( 'NONE', #13681, #16544, #25471, .T. ) ;
#19910 = CARTESIAN_POINT ( 'NONE',  ( 0.000000000000000000, -27.75498641678764855, 31.52238457039590358 ) ) ;
#19911 = PLANE ( 'NONE',  #36245 ) ;
#19912 = MANIFOLD_SOLID_BREP ( 'Boss-Extrude2', #40364 ) ;
#19913 = EDGE_LOOP ( 'NONE', ( #20482, #18134, #38819, #45739 ) ) ;
#19914 = ORIENTED_EDGE ( 'NONE', *, *, #30609, .T. ) ;
#19915 = AXIS2_PLACEMENT_3D ( 'NONE', #35693, #20269, #46226 ) ;
#19916 = DIRECTION ( 'NONE',  ( 0.000000000000000000, 0.000000000000000000, 1.000000000000000000 ) ) ;
#19917 = ORIENTED_EDGE ( 'NONE', *, *, #35324, .F. ) ;
#19918 = ORIENTED_EDGE ( 'NONE', *, *, #11780, .F. ) ;
#19919 = CARTESIAN_POINT ( 'NONE',  ( 0.000000000000000000, -44.88180994100329713, -63.18004540533077318 ) ) ;
#19920 = VECTOR ( 'NONE', #17960, 1000.000000000000000 ) ;
#19921 = CARTESIAN_POINT ( 'NONE',  ( 0.000000000000000000, 0.000000000000000000, 0.000000000000000000 ) ) ;
#19922 = ORIENTED_EDGE ( 'NONE', *, *, #23832, .F. ) ;
#19923 = EDGE_CURVE ( 'NONE', #44741, #9216, #26707, .T. ) ;
#19924 = CIRCLE ( 'NONE', #45726, 77.49899999999999523 ) ;
#19925 = ORIENTED_EDGE ( 'NONE', *, *, #31945, .F. ) ;
#19926 = EDGE_CURVE ( 'NONE', #30912, #9644, #35228, .T. ) ;
#19927 = ORIENTED_EDGE ( 'NONE', *, *, #4707, .T. ) ;
#19928 = VECTOR ( 'NONE', #13945, 1000.000000000000000 ) ;
#19929 = EDGE_LOOP ( 'NONE', ( #25882, #21207, #10299, #47041 ) ) ;
#19930 = ORIENTED_EDGE ( 'NONE', *, *, #24818, .T. ) ;
#19931 = EDGE_CURVE ( 'NONE', #29124, #16097, #10220, .T. ) ;
#19932 = AXIS2_PLACEMENT_3D ( 'NONE', #33203, #10930, #25842 ) ;
#19933 = AXIS2_PLACEMENT_3D ( 'NONE', #11040, #10569, #33316 ) ;
#19934 = DIRECTION ( 'NONE',  ( -1.000000000000000000, 0.000000000000000000, -0.000000000000000000 ) ) ;
#19935 = DIRECTION ( 'NONE',  ( -1.000000000000000000, -0.000000000000000000, -0.000000000000000000 ) ) ;
#19936 = DIRECTION ( 'NONE',  ( 0.9435911131814398445, -0.3311129884571295534, 0.000000000000000000 ) ) ;
#19937 = VERTEX_POINT ( 'NONE', #3951 ) ;
#19938 = DIRECTION ( 'NONE',  ( -1.000000000000000000, -0.000000000000000000, -0.000000000000000000 ) ) ;
#19939 = CIRCLE ( 'NONE', #11375, 11.59999999999999787 ) ;
#19940 = EDGE_LOOP ( 'NONE', ( #26208, #4242, #3116, #6947 ) ) ;
#19941 = ORIENTED_EDGE ( 'NONE', *, *, #42154, .T. ) ;
#19942 = EDGE_CURVE ( 'NONE', #4524, #21044, #41399, .T. ) ;
#19943 = EDGE_CURVE ( 'NONE', #28297, #8075, #7622, .T. ) ;
#19944 = PLANE ( 'NONE',  #13960 ) ;
#19945 = FACE_OUTER_BOUND ( 'NONE', #4321, .T. ) ;
#19946 = CARTESIAN_POINT ( 'NONE',  ( 0.000000000000000000, 35.95386929396241271, 10.96151621346552751 ) ) ;
#19947 = VECTOR ( 'NONE', #36528, 1000.000000000000000 ) ;
#19948 = EDGE_LOOP ( 'NONE', ( #10261, #41037, #1414, #28073 ) ) ;
#19949 = ORIENTED_EDGE ( 'NONE', *, *, #7837, .F. ) ;
#19950 = ORIENTED_EDGE ( 'NONE', *, *, #30781, .T. ) ;
#19951 = CARTESIAN_POINT ( 'NONE',  ( -3.000000000000000000, 23.59884966291538078, -12.14883922797231541 ) ) ;
#19952 = ORIENTED_EDGE ( 'NONE', *, *, #7290, .F. ) ;
#19953 = DIRECTION ( 'NONE',  ( 0.000000000000000000, 0.000000000000000000, 1.000000000000000000 ) ) ;
#19954 = DIRECTION ( 'NONE',  ( 0.000000000000000000, 0.000000000000000000, 1.000000000000000000 ) ) ;
#19955 = DIRECTION ( 'NONE',  ( -1.000000000000000000, 0.000000000000000000, 0.000000000000000000 ) ) ;
#19956 = PLANE ( 'NONE',  #12807 ) ;
#19957 = LINE ( 'NONE', #8691, #46947 ) ;
#19958 = DIRECTION ( 'NONE',  ( -1.000000000000000000, -0.000000000000000000, -0.000000000000000000 ) ) ;
#19959 = CARTESIAN_POINT ( 'NONE',  ( 11.99999999999999822, -22.90783923731685334, 78.73519480814947258 ) ) ;
#19960 = ORIENTED_EDGE ( 'NONE', *, *, #25661, .F. ) ;
#19961 = CARTESIAN_POINT ( 'NONE',  ( 0.000000000000000000, 0.000000000000000000, -43.79999999999998295 ) ) ;
#19963 = CYLINDRICAL_SURFACE ( 'NONE', #48064, 16.00000000000000000 ) ;
#19962 = PRODUCT_RELATED_PRODUCT_CATEGORY ( 'part', '', ( #1883 ) ) ;
#19964 = CARTESIAN_POINT ( 'NONE',  ( 0.000000000000000000, 36.73666225445988687, -65.58780272294035285 ) ) ;
#19965 = CARTESIAN_POINT ( 'NONE',  ( 0.000000000000000000, -8.830959090342926032, 74.65491531819115778 ) ) ;
#19966 = VECTOR ( 'NONE', #42407, 1000.000000000000000 ) ;
#19967 = CIRCLE ( 'NONE', #18392, 13.71399988598171049 ) ;
#19968 = ORIENTED_EDGE ( 'NONE', *, *, #34104, .F. ) ;
#19969 = EDGE_LOOP ( 'NONE', ( #1422, #8990, #34213, #24866 ) ) ;
#19970 =( LENGTH_UNIT ( ) NAMED_UNIT ( * ) SI_UNIT ( .MILLI., .METRE. ) );
#19971 = AXIS2_PLACEMENT_3D ( 'NONE', #10883, #37550, #25797 ) ;
#19972 = CYLINDRICAL_SURFACE ( 'NONE', #40248, 31.99999999999999289 ) ;
#19973 = CYLINDRICAL_SURFACE ( 'NONE', #40051, 42.00000000000000000 ) ;
#19974 = CARTESIAN_POINT ( 'NONE',  ( 0.000000000000000000, -2.663952781846440576, 41.91543099594817789 ) ) ;
#19975 = AXIS2_PLACEMENT_3D ( 'NONE', #33390, #3765, #26291 ) ;
#19976 = VECTOR ( 'NONE', #31843, 999.9999999999998863 ) ;
#19977 = DIRECTION ( 'NONE',  ( -1.000000000000000000, 0.000000000000000000, 0.000000000000000000 ) ) ;
#19978 = DIRECTION ( 'NONE',  ( -1.000000000000000000, -0.000000000000000000, 0.000000000000000000 ) ) ;
#19979 = CIRCLE ( 'NONE', #23090, 77.49899999999998101 ) ;
#19980 = DIRECTION ( 'NONE',  ( -1.000000000000000000, 0.000000000000000000, 0.000000000000000000 ) ) ;
#19981 = DIRECTION ( 'NONE',  ( -1.000000000000000000, -0.000000000000000000, -0.000000000000000000 ) ) ;
#19982 = ORIENTED_EDGE ( 'NONE', *, *, #30978, .F. ) ;
#19983 = VERTEX_POINT ( 'NONE', #7854 ) ;
#19984 = CIRCLE ( 'NONE', #24708, 37.49900000000000233 ) ;
#19985 = LINE ( 'NONE', #15594, #3379 ) ;
#19986 = ORIENTED_EDGE ( 'NONE', *, *, #13792, .F. ) ;
#19987 = VERTEX_POINT ( 'NONE', #37481 ) ;
#19988 = VECTOR ( 'NONE', #38224, 1000.000000000000000 ) ;
#19989 = EDGE_CURVE ( 'NONE', #13555, #6779, #47725, .T. ) ;
#19990 = ADVANCED_FACE ( 'NONE', ( #15454 ), #18630, .T. ) ;
#19991 = FACE_OUTER_BOUND ( 'NONE', #11909, .T. ) ;
#19992 = ORIENTED_EDGE ( 'NONE', *, *, #8115, .F. ) ;
#19993 = EDGE_CURVE ( 'NONE', #31364, #26622, #38355, .T. ) ;
#19994 = ORIENTED_EDGE ( 'NONE', *, *, #17030, .T. ) ;
#19995 = CIRCLE ( 'NONE', #1249, 11.59999999999999787 ) ;
#19996 = CARTESIAN_POINT ( 'NONE',  ( 11.99999999999999822, -39.78640506895559525, -66.50666863322042843 ) ) ;
#19997 = LINE ( 'NONE', #42527, #12848 ) ;
#19998 = ORIENTED_EDGE ( 'NONE', *, *, #17382, .T. ) ;
#19999 = AXIS2_PLACEMENT_3D ( 'NONE', #45086, #14987, #40453 ) ;
#20000 = AXIS2_PLACEMENT_3D ( 'NONE', #12565, #27502, #36029 ) ;
#20001 = ADVANCED_FACE ( 'NONE', ( #262 ), #15221, .F. ) ;
#20002 = ADVANCED_FACE ( 'NONE', ( #37234 ), #33560, .F. ) ;
#20003 = FACE_OUTER_BOUND ( 'NONE', #3298, .T. ) ;
#20005 = ORIENTED_EDGE ( 'NONE', *, *, #38017, .T. ) ;
#20004 = DIRECTION ( 'NONE',  ( 0.000000000000000000, 0.000000000000000000, 1.000000000000000000 ) ) ;
#20006 = CARTESIAN_POINT ( 'NONE',  ( -15.44521549751111955, -137.7748507232956001, -2.500000000000000000 ) ) ;
#20007 = EDGE_LOOP ( 'NONE', ( #27679, #672, #38243, #13758 ) ) ;
#20008 = VERTEX_POINT ( 'NONE', #26466 ) ;
#20009 = AXIS2_PLACEMENT_3D ( 'NONE', #38057, #29978, #15533 ) ;
#20010 = LINE ( 'NONE', #16120, #45058 ) ;
#20011 = ADVANCED_FACE ( 'NONE', ( #34039 ), #522, .T. ) ;
#20012 = ORIENTED_EDGE ( 'NONE', *, *, #21197, .F. ) ;
#20013 = VERTEX_POINT ( 'NONE', #40663 ) ;
#20014 = CARTESIAN_POINT ( 'NONE',  ( 10.00000000000000000, 0.000000000000000000, 0.000000000000000000 ) ) ;
#20015 = DIRECTION ( 'NONE',  ( -1.000000000000000000, -0.000000000000000000, -0.000000000000000000 ) ) ;
#20016 = VERTEX_POINT ( 'NONE', #4446 ) ;
#20017 = LINE ( 'NONE', #46459, #1806 ) ;
#20018 = CARTESIAN_POINT ( 'NONE',  ( 12.49999999999999645, 1.530808498934191127E-15, -54.99999999999998579 ) ) ;
#20019 = DIRECTION ( 'NONE',  ( -0.000000000000000000, -0.000000000000000000, -1.000000000000000000 ) ) ;
#20020 = AXIS2_PLACEMENT_3D ( 'NONE', #17410, #35788, #47744 ) ;
#20021 = ORIENTED_EDGE ( 'NONE', *, *, #29941, .T. ) ;
#20022 = ORIENTED_EDGE ( 'NONE', *, *, #4210, .F. ) ;
#20023 = DIRECTION ( 'NONE',  ( -1.000000000000000000, -0.000000000000000000, -0.000000000000000000 ) ) ;
#20024 = ADVANCED_FACE ( 'NONE', ( #19351 ), #47999, .T. ) ;
#20025 = CIRCLE ( 'NONE', #47394, 77.49899999999999523 ) ;
#20026 = DIRECTION ( 'NONE',  ( -1.000000000000000000, 0.000000000000000000, -0.000000000000000000 ) ) ;
#20027 = VERTEX_POINT ( 'NONE', #19 ) ;
#20028 = CARTESIAN_POINT ( 'NONE',  ( 10.00000000000000000, 37.58145647212453611, 0.6853352020791767529 ) ) ;
#20029 = ORIENTED_EDGE ( 'NONE', *, *, #45164, .T. ) ;
#20030 = CARTESIAN_POINT ( 'NONE',  ( -3.000000000000000000, -23.29833615347109443, 3.418703333116492438 ) ) ;
#20031 = DIRECTION ( 'NONE',  ( -1.000000000000000000, -0.000000000000000000, 0.000000000000000000 ) ) ;
#20032 = DIRECTION ( 'NONE',  ( -1.000000000000000000, 0.000000000000000000, 0.000000000000000000 ) ) ;
#20033 = VERTEX_POINT ( 'NONE', #44575 ) ;
#20034 = DIRECTION ( 'NONE',  ( 0.000000000000000000, 0.000000000000000000, 1.000000000000000000 ) ) ;
#20035 = DIRECTION ( 'NONE',  ( -1.000000000000000000, -0.000000000000000000, 0.000000000000000000 ) ) ;
#20036 = LINE ( 'NONE', #34965, #41994 ) ;
#20037 = AXIS2_PLACEMENT_3D ( 'NONE', #11706, #34687, #4845 ) ;
#20038 = DIRECTION ( 'NONE',  ( -1.000000000000000000, -0.000000000000000000, 0.000000000000000000 ) ) ;
#20039 = DIRECTION ( 'NONE',  ( -1.000000000000000000, 0.000000000000000000, -0.000000000000000000 ) ) ;
#20040 = CIRCLE ( 'NONE', #15377, 16.00000000000000000 ) ;
#20041 = DIRECTION ( 'NONE',  ( 0.000000000000000000, 0.000000000000000000, 1.000000000000000000 ) ) ;
#20042 = SURFACE_SIDE_STYLE ('',( #1454 ) ) ;
#20043 = ORIENTED_EDGE ( 'NONE', *, *, #14729, .T. ) ;
#20044 = VECTOR ( 'NONE', #39849, 1000.000000000000000 ) ;
#20045 = CYLINDRICAL_SURFACE ( 'NONE', #12104, 42.00000000000000000 ) ;
#20046 = EDGE_CURVE ( 'NONE', #25493, #22407, #44606, .T. ) ;
#20047 = ORIENTED_EDGE ( 'NONE', *, *, #14626, .T. ) ;
#20048 = DIRECTION ( 'NONE',  ( -1.000000000000000000, -0.000000000000000000, -0.000000000000000000 ) ) ;
#20049 = AXIS2_PLACEMENT_3D ( 'NONE', #7268, #14386, #21955 ) ;
#20050 = CARTESIAN_POINT ( 'NONE',  ( 10.00000000000000000, -21.53537804866103045, 30.80686688397002371 ) ) ;
#20051 = ADVANCED_FACE ( 'NONE', ( #3456, #33323 ), #44821, .F. ) ;
#20052 = VERTEX_POINT ( 'NONE', #26958 ) ;
#20053 = EDGE_CURVE ( 'NONE', #5351, #929, #30616, .T. ) ;
#20054 = CIRCLE ( 'NONE', #14627, 37.49900000000000944 ) ;
#20056 = EDGE_LOOP ( 'NONE', ( #39333, #9955, #12983, #44553 ) ) ;
#20055 = EDGE_CURVE ( 'NONE', #8930, #48358, #32882, .T. ) ;
#20057 = ADVANCED_FACE ( 'NONE', ( #15935 ), #27676, .T. ) ;
#20058 = CARTESIAN_POINT ( 'NONE',  ( 10.00000000000000000, 2.956366410621684260, -75.11725578898465017 ) ) ;
#20059 = ORIENTED_EDGE ( 'NONE', *, *, #33154, .F. ) ;
#20060 = VERTEX_POINT ( 'NONE', #31603 ) ;
#20061 = VERTEX_POINT ( 'NONE', #23749 ) ;
#20062 = ORIENTED_EDGE ( 'NONE', *, *, #16425, .T. ) ;
#20063 = VERTEX_POINT ( 'NONE', #41888 ) ;
#20064 = EDGE_CURVE ( 'NONE', #46270, #12261, #41495, .T. ) ;
#20065 = AXIS2_PLACEMENT_3D ( 'NONE', #136, #41279, #44455 ) ;
#20066 = DIRECTION ( 'NONE',  ( -1.000000000000000000, 0.000000000000000000, 0.000000000000000000 ) ) ;
#20067 = ORIENTED_EDGE ( 'NONE', *, *, #29455, .T. ) ;
#20068 = ORIENTED_EDGE ( 'NONE', *, *, #549, .T. ) ;
#20069 = FACE_OUTER_BOUND ( 'NONE', #8677, .T. ) ;
#20070 = ADVANCED_FACE ( 'NONE', ( #42850 ), #12994, .T. ) ;
#20071 = VERTEX_POINT ( 'NONE', #985 ) ;
#20072 = APPLICATION_CONTEXT ( 'automotive_design' ) ;
#20073 = PLANE ( 'NONE',  #9489 ) ;
#20074 = VECTOR ( 'NONE', #39129, 1000.000000000000000 ) ;
#20075 = DIRECTION ( 'NONE',  ( 1.000000000000000000, 0.000000000000000000, 0.000000000000000000 ) ) ;
#20076 = CYLINDRICAL_SURFACE ( 'NONE', #45496, 82.00000000000000000 ) ;
#20077 = EDGE_LOOP ( 'NONE', ( #7565, #5263, #47468, #247 ) ) ;
#20078 = DIRECTION ( 'NONE',  ( -0.7533909544171996098, -0.6575728627325955200, 7.625282249115660656E-32 ) ) ;
#20079 = ORIENTED_EDGE ( 'NONE', *, *, #27471, .F. ) ;
#20080 = LINE ( 'NONE', #21035, #41472 ) ;
#20081 = ADVANCED_FACE ( 'NONE', ( #8811 ), #27196, .T. ) ;
#20082 = CARTESIAN_POINT ( 'NONE',  ( 11.99999999999999822, 68.27212725128275395, -31.46837873495001503 ) ) ;
#20083 = EDGE_LOOP ( 'NONE', ( #43212, #16659, #1709, #35284 ) ) ;
#20084 = CARTESIAN_POINT ( 'NONE',  ( 0.000000000000000000, 20.85821328998756385, -10.92862929874494959 ) ) ;
#20085 = VERTEX_POINT ( 'NONE', #12271 ) ;
#20086 = ORIENTED_EDGE ( 'NONE', *, *, #8356, .F. ) ;
#20087 = CYLINDRICAL_SURFACE ( 'NONE', #28370, 82.00000000000000000 ) ;
#20088 = DIRECTION ( 'NONE',  ( 0.000000000000000000, 0.000000000000000000, 1.000000000000000000 ) ) ;
#20089 = VERTEX_POINT ( 'NONE', #24233 ) ;
#20090 = DIRECTION ( 'NONE',  ( 0.000000000000000000, 0.000000000000000000, 1.000000000000000000 ) ) ;
#20091 = CARTESIAN_POINT ( 'NONE',  ( 10.00000000000000000, 24.73286445877808148, -73.44644590900034586 ) ) ;
#20092 = FACE_OUTER_BOUND ( 'NONE', #24867, .T. ) ;
#20093 = AXIS2_PLACEMENT_3D ( 'NONE', #25088, #2569, #6742 ) ;
#20094 = LINE ( 'NONE', #32320, #6238 ) ;
#20095 = CARTESIAN_POINT ( 'NONE',  ( -3.000000000000000000, 5.835314593368772229, -22.81335362449846826 ) ) ;
#20096 = AXIS2_PLACEMENT_3D ( 'NONE', #1875, #31753, #46898 ) ;
#20097 = DIRECTION ( 'NONE',  ( -1.000000000000000000, 0.000000000000000000, -0.000000000000000000 ) ) ;
#20098 = EDGE_CURVE ( 'NONE', #17381, #37423, #25056, .T. ) ;
#20099 = DIRECTION ( 'NONE',  ( 0.000000000000000000, 0.8910065241883690090, -0.4539904997395446395 ) ) ;
#20100 = LINE ( 'NONE', #12523, #41239 ) ;
#20101 = CARTESIAN_POINT ( 'NONE',  ( -3.000000000000000000, 26.50000000000000355, 1.500000000000000000 ) ) ;
#20102 = CARTESIAN_POINT ( 'NONE',  ( 18.80329974962065265, -105.8248132807389084, 5.500000000000000000 ) ) ;
#20103 = DIRECTION ( 'NONE',  ( 0.000000000000000000, 0.4999999999999938938, -0.8660254037844421493 ) ) ;
#20104 = DIRECTION ( 'NONE',  ( -1.000000000000000000, 0.000000000000000000, 0.000000000000000000 ) ) ;
#20105 = DIRECTION ( 'NONE',  ( -1.000000000000000000, 0.000000000000000000, 0.000000000000000000 ) ) ;
#20106 = VERTEX_POINT ( 'NONE', #42610 ) ;
#20107 = AXIS2_PLACEMENT_3D ( 'NONE', #40030, #36585, #28533 ) ;
#20108 = VERTEX_POINT ( 'NONE', #24005 ) ;
#20109 = AXIS2_PLACEMENT_3D ( 'NONE', #35362, #2545, #5513 ) ;
#20110 = CARTESIAN_POINT ( 'NONE',  ( -43.60332556124591719, -107.0000000000000000, 2.500000000000002220 ) ) ;
#20111 = ADVANCED_FACE ( 'NONE', ( #39167 ), #23276, .T. ) ;
#20112 = DIRECTION ( 'NONE',  ( 0.000000000000000000, 0.000000000000000000, 1.000000000000000000 ) ) ;
#20113 = ITEM_DEFINED_TRANSFORMATION ( 'NONE', 'NONE', #6922,  #11636 ) ;
#20115 = EDGE_CURVE ( 'NONE', #42670, #32991, #28183, .T. ) ;
#20114 = VECTOR ( 'NONE', #2880, 1000.000000000000000 ) ;
#20116 = CARTESIAN_POINT ( 'NONE',  ( 10.00000000000000000, 31.52238457039599595, 27.75498641678753842 ) ) ;
#20117 = ORIENTED_EDGE ( 'NONE', *, *, #44499, .T. ) ;
#20118 = ADVANCED_FACE ( 'NONE', ( #38207 ), #31360, .T. ) ;
#20119 = CIRCLE ( 'NONE', #24808, 31.99999999999998579 ) ;
#20120 = ADVANCED_FACE ( 'NONE', ( #8571 ), #42357, .T. ) ;
#20121 = CARTESIAN_POINT ( 'NONE',  ( 10.00000000000000000, 75.16055320797059380, -18.89407956138177269 ) ) ;
#20122 = EDGE_LOOP ( 'NONE', ( #30241, #38421, #17841, #40074 ) ) ;
#20123 = DIRECTION ( 'NONE',  ( -1.000000000000000000, -0.000000000000000000, -0.000000000000000000 ) ) ;
#20124 = VECTOR ( 'NONE', #47964, 999.9999999999998863 ) ;
#20125 = CARTESIAN_POINT ( 'NONE',  ( 11.99999999999999822, 0.000000000000000000, 0.000000000000000000 ) ) ;
#20126 = CARTESIAN_POINT ( 'NONE',  ( 0.000000000000000000, 22.90783923731741112, -78.73519480814930205 ) ) ;
#20127 = EDGE_LOOP ( 'NONE', ( #37470, #4132, #11360, #31543 ) ) ;
#20129 = EDGE_LOOP ( 'NONE', ( #3875, #21556, #2718, #37041 ) ) ;
#20128 = DIRECTION ( 'NONE',  ( 0.000000000000000000, 0.000000000000000000, -1.000000000000000000 ) ) ;
#20130 = ORIENTED_EDGE ( 'NONE', *, *, #10330, .T. ) ;
#20131 = ORIENTED_EDGE ( 'NONE', *, *, #36065, .T. ) ;
#20132 = CYLINDRICAL_SURFACE ( 'NONE', #43134, 31.99999999999998579 ) ;
#20133 = ORIENTED_EDGE ( 'NONE', *, *, #8328, .T. ) ;
#20134 = DIRECTION ( 'NONE',  ( -1.000000000000000000, 0.000000000000000000, -0.000000000000000000 ) ) ;
#20135 = DIRECTION ( 'NONE',  ( -1.000000000000000000, -0.000000000000000000, -0.000000000000000000 ) ) ;
#20136 = CARTESIAN_POINT ( 'NONE',  ( 0.000000000000000000, 0.000000000000000000, 52.00000000000002132 ) ) ;
#20138 = DIRECTION ( 'NONE',  ( 0.000000000000000000, 0.000000000000000000, -1.000000000000000000 ) ) ;
#20137 = AXIS2_PLACEMENT_3D ( 'NONE', #15937, #14970, #44823 ) ;
#20139 = ORIENTED_EDGE ( 'NONE', *, *, #12109, .T. ) ;
#20140 = PLANE ( 'NONE',  #23251 ) ;
#20141 = ORIENTED_EDGE ( 'NONE', *, *, #35820, .T. ) ;
#20142 = EDGE_LOOP ( 'NONE', ( #24294, #16221, #37606, #3500 ) ) ;
#20143 = DIRECTION ( 'NONE',  ( 0.000000000000000000, 0.000000000000000000, -1.000000000000000000 ) ) ;
#20144 = ORIENTED_EDGE ( 'NONE', *, *, #48112, .T. ) ;
#20145 =( GEOMETRIC_REPRESENTATION_CONTEXT ( 3 ) GLOBAL_UNCERTAINTY_ASSIGNED_CONTEXT ( ( #7096 ) ) GLOBAL_UNIT_ASSIGNED_CONTEXT ( ( #1273, #24029, #12055 ) ) REPRESENTATION_CONTEXT ( 'NONE', 'WORKASPACE' ) );
#20146 = DIRECTION ( 'NONE',  ( -1.000000000000000000, 0.000000000000000000, -0.000000000000000000 ) ) ;
#20147 = DIRECTION ( 'NONE',  ( 0.000000000000000000, 0.1564344650402313408, -0.9876883405951376593 ) ) ;
#20148 = FACE_OUTER_BOUND ( 'NONE', #21496, .T. ) ;
#20149 = ORIENTED_EDGE ( 'NONE', *, *, #39352, .T. ) ;
#20150 = CARTESIAN_POINT ( 'NONE',  ( -3.000000000000000000, -1.278221433540145391, -26.51162292216073979 ) ) ;
#20151 = DIRECTION ( 'NONE',  ( -1.000000000000000000, 0.000000000000000000, 0.000000000000000000 ) ) ;
#20152 = DIRECTION ( 'NONE',  ( 0.000000000000000000, 0.3090169943749480619, -0.9510565162951533091 ) ) ;
#20153 = LINE ( 'NONE', #5465, #31482 ) ;
#20154 = CYLINDRICAL_SURFACE ( 'NONE', #2068, 31.99999999999998579 ) ;
#20155 = LINE ( 'NONE', #39741, #20729 ) ;
#20156 = DIRECTION ( 'NONE',  ( 0.9966891607226785466, 0.08130631524009969413, 0.000000000000000000 ) ) ;
#20157 = DIRECTION ( 'NONE',  ( -1.000000000000000000, 0.000000000000000000, -0.000000000000000000 ) ) ;
#20158 = CARTESIAN_POINT ( 'NONE',  ( -17.26469406256017791, -140.1601175325492648, -5.500000000000000000 ) ) ;
#20159 = DIRECTION ( 'NONE',  ( 0.000000000000000000, 0.000000000000000000, 1.000000000000000000 ) ) ;
#20160 = EDGE_LOOP ( 'NONE', ( #43747, #30939, #23215, #18382 ) ) ;
#20161 = AXIS2_PLACEMENT_3D ( 'NONE', #38091, #19458, #45920 ) ;
#20162 = ORIENTED_EDGE ( 'NONE', *, *, #14705, .F. ) ;
#20163 = EDGE_CURVE ( 'NONE', #2616, #20736, #30875, .T. ) ;
#20164 = DIRECTION ( 'NONE',  ( 0.000000000000000000, 0.8526401643540897357, 0.5224985647159531288 ) ) ;
#20165 = ORIENTED_EDGE ( 'NONE', *, *, #29201, .F. ) ;
#20166 = EDGE_CURVE ( 'NONE', #24152, #33539, #45800, .T. ) ;
#20167 = LINE ( 'NONE', #2067, #44750 ) ;
#20168 = ORIENTED_EDGE ( 'NONE', *, *, #31869, .F. ) ;
#20169 = EDGE_CURVE ( 'NONE', #17121, #13194, #32108, .T. ) ;
#20170 = CARTESIAN_POINT ( 'NONE',  ( 10.00000000000000000, 12.42422080174688404, -35.38097989696498047 ) ) ;
#20171 = ORIENTED_EDGE ( 'NONE', *, *, #31180, .T. ) ;
#20172 = VECTOR ( 'NONE', #15096, 1000.000000000000000 ) ;
#20173 = EDGE_CURVE ( 'NONE', #28952, #12242, #46037, .T. ) ;
#20174 = EDGE_LOOP ( 'NONE', ( #37184, #38513, #10817, #25152 ) ) ;
#20175 = VECTOR ( 'NONE', #34538, 1000.000000000000000 ) ;
#20177 = EDGE_CURVE ( 'NONE', #33371, #3949, #42264, .T. ) ;
#20176 = ORIENTED_EDGE ( 'NONE', *, *, #18986, .F. ) ;
#20178 = ORIENTED_EDGE ( 'NONE', *, *, #13150, .F. ) ;
#20179 = CIRCLE ( 'NONE', #31919, 82.00000000000000000 ) ;
#20180 = ORIENTED_EDGE ( 'NONE', *, *, #17227, .T. ) ;
#20181 = LINE ( 'NONE', #5740, #12787 ) ;
#20182 = CARTESIAN_POINT ( 'NONE',  ( 0.000000000000000000, 31.46837873495072913, -68.27212725128242710 ) ) ;
#20184 = VERTEX_POINT ( 'NONE', #36209 ) ;
#20183 = DIRECTION ( 'NONE',  ( -1.000000000000000000, 0.000000000000000000, 0.000000000000000000 ) ) ;
#20185 = ADVANCED_FACE ( 'NONE', ( #43567 ), #35735, .T. ) ;
#20186 = ORIENTED_EDGE ( 'NONE', *, *, #21965, .T. ) ;
#20187 = DIRECTION ( 'NONE',  ( 0.000000000000000000, 0.000000000000000000, 1.000000000000000000 ) ) ;
#20188 = PRODUCT_DEFINITION_FORMATION_WITH_SPECIFIED_SOURCE ( 'ANY', '', #9689, .NOT_KNOWN. ) ;
#20189 = ORIENTED_EDGE ( 'NONE', *, *, #39317, .T. ) ;
#20190 = CARTESIAN_POINT ( 'NONE',  ( 10.00000000000000000, 0.000000000000000000, 0.000000000000000000 ) ) ;
#20191 = DIRECTION ( 'NONE',  ( -1.000000000000000000, -0.000000000000000000, 0.000000000000000000 ) ) ;
#20192 = DIRECTION ( 'NONE',  ( -1.000000000000000000, -0.000000000000000000, 0.000000000000000000 ) ) ;
#20193 = AXIS2_PLACEMENT_3D ( 'NONE', #12387, #34163, #636 ) ;
#20194 = ORIENTED_EDGE ( 'NONE', *, *, #37446, .F. ) ;
#20195 = ORIENTED_EDGE ( 'NONE', *, *, #19721, .T. ) ;
#20196 = DIRECTION ( 'NONE',  ( 0.000000000000000000, 0.000000000000000000, -1.000000000000000000 ) ) ;
#20197 = ORIENTED_EDGE ( 'NONE', *, *, #39740, .F. ) ;
#20198 = CARTESIAN_POINT ( 'NONE',  ( 11.99999999999999822, 0.000000000000000000, 0.000000000000000000 ) ) ;
#20199 = CARTESIAN_POINT ( 'NONE',  ( 0.000000000000000000, 18.89407956138257205, 75.16055320797038064 ) ) ;
#20200 = CARTESIAN_POINT ( 'NONE',  ( 11.99999999999999822, 0.000000000000000000, 0.000000000000000000 ) ) ;
#20201 = CARTESIAN_POINT ( 'NONE',  ( 11.99999999999999822, 58.39081064771751528, 50.95692526931350841 ) ) ;
#20202 = LINE ( 'NONE', #35125, #45462 ) ;
#20203 = DIRECTION ( 'NONE',  ( 1.000000000000000000, -0.000000000000000000, -0.000000000000000000 ) ) ;
#20204 = DIRECTION ( 'NONE',  ( -1.000000000000000000, -0.000000000000000000, 0.000000000000000000 ) ) ;
#20205 = ORIENTED_EDGE ( 'NONE', *, *, #520, .F. ) ;
#20206 = DIRECTION ( 'NONE',  ( -1.000000000000000000, 0.000000000000000000, -0.000000000000000000 ) ) ;
#20207 = FACE_OUTER_BOUND ( 'NONE', #44034, .T. ) ;
#20208 = PLANE ( 'NONE',  #2485 ) ;
#20209 = CARTESIAN_POINT ( 'NONE',  ( 10.00000000000000000, 74.65491531819118620, -8.830959090342659579 ) ) ;
#20210 = EDGE_CURVE ( 'NONE', #10102, #20931, #39420, .T. ) ;
#20211 = ORIENTED_EDGE ( 'NONE', *, *, #27581, .T. ) ;
#20212 = ORIENTED_EDGE ( 'NONE', *, *, #12231, .T. ) ;
#20213 = EDGE_CURVE ( 'NONE', #37878, #44222, #21978, .T. ) ;
#20214 = VECTOR ( 'NONE', #16597, 1000.000000000000000 ) ;
#20215 = DIRECTION ( 'NONE',  ( -1.000000000000000000, 0.000000000000000000, 0.000000000000000000 ) ) ;
#20216 = CARTESIAN_POINT ( 'NONE',  ( -7.572224309238338336, -145.4393675041377492, 2.500000000000000000 ) ) ;
#20217 = VECTOR ( 'NONE', #27796, 1000.000000000000000 ) ;
#20218 = ADVANCED_FACE ( 'NONE', ( #47470 ), #25180, .T. ) ;
#20219 = DIRECTION ( 'NONE',  ( -1.000000000000000000, -0.000000000000000000, -0.000000000000000000 ) ) ;
#20220 = DIRECTION ( 'NONE',  ( 0.000000000000000000, 0.9510565162951523099, 0.3090169943749517811 ) ) ;
#20221 = DIRECTION ( 'NONE',  ( -1.000000000000000000, -0.000000000000000000, -0.000000000000000000 ) ) ;
#20222 = DIRECTION ( 'NONE',  ( 0.000000000000000000, 0.6494480483301849905, -0.7604059656000299317 ) ) ;
#20223 = VERTEX_POINT ( 'NONE', #21271 ) ;
#20224 = ORIENTED_EDGE ( 'NONE', *, *, #16635, .T. ) ;
#20225 = EDGE_CURVE ( 'NONE', #29124, #10023, #3029, .T. ) ;
#20226 = EDGE_CURVE ( 'NONE', #46270, #36913, #13941, .T. ) ;
#20227 = PRESENTATION_STYLE_ASSIGNMENT (( #12652 ) ) ;
#20228 = CARTESIAN_POINT ( 'NONE',  ( 15.00000000000000000, -20.55727247249748402, -16.78983467731284307 ) ) ;
#20229 = EDGE_CURVE ( 'NONE', #36905, #26495, #4773, .T. ) ;
#20230 = ADVANCED_FACE ( 'NONE', ( #25426 ), #47692, .T. ) ;
#20231 = ORIENTED_EDGE ( 'NONE', *, *, #6854, .T. ) ;
#20232 = VECTOR ( 'NONE', #31628, 1000.000000000000114 ) ;
#20233 = ORIENTED_EDGE ( 'NONE', *, *, #41303, .T. ) ;
#20234 = ORIENTED_EDGE ( 'NONE', *, *, #5938, .F. ) ;
#20235 = DIRECTION ( 'NONE',  ( -0.000000000000000000, -0.000000000000000000, -1.000000000000000000 ) ) ;
#20236 = VERTEX_POINT ( 'NONE', #32547 ) ;
#20237 = ORIENTED_EDGE ( 'NONE', *, *, #40398, .F. ) ;
#20238 = AXIS2_PLACEMENT_3D ( 'NONE', #6823, #17585, #14162 ) ;
#20239 = DIRECTION ( 'NONE',  ( 1.000000000000000000, 0.000000000000000000, 0.000000000000000000 ) ) ;
#20241 = VERTEX_POINT ( 'NONE', #31849 ) ;
#20240 = FACE_OUTER_BOUND ( 'NONE', #12461, .T. ) ;
#20242 = AXIS2_PLACEMENT_3D ( 'NONE', #35883, #43717, #32228 ) ;
#20243 = VERTEX_POINT ( 'NONE', #39670 ) ;
#20244 = ORIENTED_EDGE ( 'NONE', *, *, #23956, .T. ) ;
#20245 = ORIENTED_EDGE ( 'NONE', *, *, #5360, .T. ) ;
#20246 = CARTESIAN_POINT ( 'NONE',  ( 10.00000000000000000, 41.91543099594818500, -2.663952781846293139 ) ) ;
#20248 = EDGE_LOOP ( 'NONE', ( #40894, #26149, #7855, #42592 ) ) ;
#20247 = CARTESIAN_POINT ( 'NONE',  ( 0.000000000000000000, -6.903761155838323837, 77.19088730480521576 ) ) ;
#20249 = DIRECTION ( 'NONE',  ( 0.000000000000000000, 0.000000000000000000, 1.000000000000000000 ) ) ;
#20250 = EDGE_LOOP ( 'NONE', ( #21597, #5425, #15156, #21303 ) ) ;
#20251 = DIRECTION ( 'NONE',  ( 0.000000000000000000, 0.000000000000000000, 1.000000000000000000 ) ) ;
#20252 = EDGE_LOOP ( 'NONE', ( #447, #8747, #33584, #2501 ) ) ;
#20253 = CYLINDRICAL_SURFACE ( 'NONE', #26728, 31.99999999999999289 ) ;
#20254 = CARTESIAN_POINT ( 'NONE',  ( 0.000000000000000000, 22.07842321921481243, 8.187992925817422218 ) ) ;
#20255 = ORIENTED_EDGE ( 'NONE', *, *, #5950, .F. ) ;
#20256 = CARTESIAN_POINT ( 'NONE',  ( 10.00000000000000000, 9.188173127307297960, 40.98264845739753071 ) ) ;
#20257 = DIRECTION ( 'NONE',  ( 0.000000000000000000, 0.07845909572784530439, -0.9969173337331279638 ) ) ;
#20258 = CARTESIAN_POINT ( 'NONE',  ( 11.99999999999999822, 0.000000000000000000, 0.000000000000000000 ) ) ;
#20259 = VERTEX_POINT ( 'NONE', #43796 ) ;
#20260 = ORIENTED_EDGE ( 'NONE', *, *, #27000, .F. ) ;
#20261 = ADVANCED_FACE ( 'NONE', ( #10260 ), #21530, .F. ) ;
#20262 = CYLINDRICAL_SURFACE ( 'NONE', #42269, 37.49900000000000233 ) ;
#20263 = DIRECTION ( 'NONE',  ( 1.000000000000000000, 0.000000000000000000, 0.000000000000000000 ) ) ;
#20264 = EDGE_CURVE ( 'NONE', #3749, #25146, #32077, .T. ) ;
#20265 = ORIENTED_EDGE ( 'NONE', *, *, #17431, .T. ) ;
#20266 = LINE ( 'NONE', #16853, #32716 ) ;
#20267 = ORIENTED_EDGE ( 'NONE', *, *, #11878, .T. ) ;
#20268 = EDGE_CURVE ( 'NONE', #1521, #23469, #10246, .T. ) ;
#20269 = DIRECTION ( 'NONE',  ( 0.000000000000000000, 0.000000000000000000, -1.000000000000000000 ) ) ;
#20270 = DIRECTION ( 'NONE',  ( -1.000000000000000000, 0.000000000000000000, 0.000000000000000000 ) ) ;
#20271 = CARTESIAN_POINT ( 'NONE',  ( 0.000000000000000000, -46.21855187248585395, -62.20884554314068993 ) ) ;
#20272 = LINE ( 'NONE', #1685, #40102 ) ;
#20273 = EDGE_CURVE ( 'NONE', #21915, #15144, #16896, .T. ) ;
#20274 = ORIENTED_EDGE ( 'NONE', *, *, #6913, .F. ) ;
#20275 = DIRECTION ( 'NONE',  ( 0.9435911131814395114, -0.3311129884571304971, 0.000000000000000000 ) ) ;
#20276 = CARTESIAN_POINT ( 'NONE',  ( 10.00000000000000000, 0.000000000000000000, 0.000000000000000000 ) ) ;
#20277 = DIRECTION ( 'NONE',  ( -1.000000000000000000, 0.000000000000000000, -0.000000000000000000 ) ) ;
#20278 = AXIS2_PLACEMENT_3D ( 'NONE', #35161, #20473, #12665 ) ;
#20279 = FACE_OUTER_BOUND ( 'NONE', #24647, .T. ) ;
#20280 = ORIENTED_EDGE ( 'NONE', *, *, #4841, .T. ) ;
#20281 = DIRECTION ( 'NONE',  ( -1.000000000000000000, -0.000000000000000000, 0.000000000000000000 ) ) ;
#20282 = ADVANCED_FACE ( 'NONE', ( #40381 ), #28385, .T. ) ;
#20283 = EDGE_CURVE ( 'NONE', #30855, #38126, #11024, .T. ) ;
#20284 = ORIENTED_EDGE ( 'NONE', *, *, #46634, .F. ) ;
#20285 = CIRCLE ( 'NONE', #14036, 32.00000000000000000 ) ;
#20286 = DIRECTION ( 'NONE',  ( 0.000000000000000000, 0.7071067811865437980, 0.7071067811865512365 ) ) ;
#20287 = LINE ( 'NONE', #28361, #46475 ) ;
#20288 = EDGE_LOOP ( 'NONE', ( #22587, #25831, #7181, #22314 ) ) ;
#20289 = EDGE_CURVE ( 'NONE', #18512, #7570, #20553, .T. ) ;
#20290 = DIRECTION ( 'NONE',  ( -1.000000000000000000, -0.000000000000000000, -0.000000000000000000 ) ) ;
#20291 = ORIENTED_EDGE ( 'NONE', *, *, #31701, .F. ) ;
#20292 = ORIENTED_EDGE ( 'NONE', *, *, #15963, .T. ) ;
#20293 = ORIENTED_EDGE ( 'NONE', *, *, #23938, .F. ) ;
#20294 = CIRCLE ( 'NONE', #11719, 82.00000000000000000 ) ;
#20295 = CARTESIAN_POINT ( 'NONE',  ( 0.000000000000000000, 0.000000000000000000, 0.000000000000000000 ) ) ;
#20296 = ORIENTED_EDGE ( 'NONE', *, *, #40882, .F. ) ;
#20297 = CARTESIAN_POINT ( 'NONE',  ( 10.00000000000000000, 41.76106447765580043, -62.50884508063379741 ) ) ;
#20298 = EDGE_LOOP ( 'NONE', ( #16775, #32897, #42550, #34916 ) ) ;
#20299 = LINE ( 'NONE', #27430, #40764 ) ;
#20300 = DIRECTION ( 'NONE',  ( 0.000000000000000000, 0.000000000000000000, -1.000000000000000000 ) ) ;
#20301 = CARTESIAN_POINT ( 'NONE',  ( 5.000000000000000000, 26.79245525562714292, 32.34446384429980981 ) ) ;
#20302 = ORIENTED_EDGE ( 'NONE', *, *, #13704, .F. ) ;
#20303 = AXIS2_PLACEMENT_3D ( 'NONE', #19244, #4081, #34169 ) ;
#20304 = CARTESIAN_POINT ( 'NONE',  ( 10.00000000000000000, -70.52718814184277107, 26.02418014898285037 ) ) ;
#20305 = ORIENTED_EDGE ( 'NONE', *, *, #38591, .F. ) ;
#20306 = DIRECTION ( 'NONE',  ( -1.000000000000000000, -0.000000000000000000, -0.000000000000000000 ) ) ;
#20307 = DIRECTION ( 'NONE',  ( -1.000000000000000000, 0.000000000000000000, 0.000000000000000000 ) ) ;
#20308 = FACE_OUTER_BOUND ( 'NONE', #48164, .T. ) ;
#20309 = ORIENTED_EDGE ( 'NONE', *, *, #38063, .T. ) ;
#20310 = AXIS2_PLACEMENT_3D ( 'NONE', #10574, #21812, #33070 ) ;
#20311 = ORIENTED_EDGE ( 'NONE', *, *, #3177, .T. ) ;
#20312 = DIRECTION ( 'NONE',  ( 0.000000000000000000, 0.7604059656000323741, -0.6494480483301819929 ) ) ;
#20313 = DIRECTION ( 'NONE',  ( -1.000000000000000000, -0.000000000000000000, 0.000000000000000000 ) ) ;
#20314 = ORIENTED_EDGE ( 'NONE', *, *, #19544, .F. ) ;
#20315 = EDGE_CURVE ( 'NONE', #33061, #38396, #47763, .T. ) ;
#20316 = FACE_OUTER_BOUND ( 'NONE', #15104, .T. ) ;
#20317 = CARTESIAN_POINT ( 'NONE',  ( 0.000000000000000000, 30.00120703465236716, -22.64427369931138756 ) ) ;
#20318 = DIRECTION ( 'NONE',  ( 0.000000000000000000, 0.000000000000000000, 1.000000000000000000 ) ) ;
#20319 = DIRECTION ( 'NONE',  ( -1.000000000000000000, 0.000000000000000000, 0.000000000000000000 ) ) ;
#20320 = ADVANCED_FACE ( 'NONE', ( #37421 ), #30087, .F. ) ;
#20321 = CARTESIAN_POINT ( 'NONE',  ( 11.99999999999999822, -31.47745569255189224, 68.26794271651249346 ) ) ;
#20322 = CARTESIAN_POINT ( 'NONE',  ( 0.000000000000000000, -64.81221759200306565, -50.23322058963418613 ) ) ;
#20323 = CARTESIAN_POINT ( 'NONE',  ( 10.00000000000000000, 16.65560815589464028, -38.55633173626993937 ) ) ;
#20324 = EDGE_CURVE ( 'NONE', #36936, #35718, #14942, .T. ) ;
#20325 = CARTESIAN_POINT ( 'NONE',  ( 11.99999999999999822, 35.91791733033570466, -68.67312586194960033 ) ) ;
#20326 = DIRECTION ( 'NONE',  ( -1.000000000000000000, -0.000000000000000000, 0.000000000000000000 ) ) ;
#20327 = VERTEX_POINT ( 'NONE', #3148 ) ;
#20328 = CARTESIAN_POINT ( 'NONE',  ( 10.00000000000000000, -33.79645857604501913, -16.45098606841161626 ) ) ;
#20329 = LINE ( 'NONE', #35986, #14413 ) ;
#20330 = DIRECTION ( 'NONE',  ( -1.000000000000000000, -0.000000000000000000, -0.000000000000000000 ) ) ;
#20331 = CARTESIAN_POINT ( 'NONE',  ( 15.00000000000000000, 0.000000000000000000, 0.000000000000000000 ) ) ;
#20332 = EDGE_LOOP ( 'NONE', ( #36211, #42143, #33986, #39927 ) ) ;
#20333 = ADVANCED_FACE ( 'NONE', ( #18077 ), #45249, .T. ) ;
#20334 = ORIENTED_EDGE ( 'NONE', *, *, #43498, .T. ) ;
#20335 = AXIS2_PLACEMENT_3D ( 'NONE', #35839, #46141, #27538 ) ;
#20336 = CARTESIAN_POINT ( 'NONE',  ( 15.00000000000000000, -19.89357724624986545, 12.59942793731086219 ) ) ;
#20337 = CIRCLE ( 'NONE', #43781, 37.49900000000001654 ) ;
#20338 = ADVANCED_FACE ( 'NONE', ( #30330 ), #41110, .T. ) ;
#20339 = LINE ( 'NONE', #31393, #10373 ) ;
#20340 = CIRCLE ( 'NONE', #5499, 31.99999999999998934 ) ;
#20341 = VECTOR ( 'NONE', #35230, 1000.000000000000000 ) ;
#20342 = CARTESIAN_POINT ( 'NONE',  ( 0.000000000000000000, 0.000000000000000000, -44.99999999999998579 ) ) ;
#20343 = ORIENTED_EDGE ( 'NONE', *, *, #36836, .T. ) ;
#20344 = AXIS2_PLACEMENT_3D ( 'NONE', #2557, #47373, #36341 ) ;
#20345 = VECTOR ( 'NONE', #272, 1000.000000000000000 ) ;
#20346 = ADVANCED_FACE ( 'NONE', ( #464 ), #44759, .T. ) ;
#20347 = AXIS2_PLACEMENT_3D ( 'NONE', #12270, #45799, #38440 ) ;
#20348 = DIRECTION ( 'NONE',  ( 0.000000000000000000, 0.000000000000000000, 1.000000000000000000 ) ) ;
#20349 = ORIENTED_EDGE ( 'NONE', *, *, #43165, .T. ) ;
#20350 = DIRECTION ( 'NONE',  ( 1.000000000000000000, 0.000000000000000000, 0.000000000000000000 ) ) ;
#20351 = ORIENTED_EDGE ( 'NONE', *, *, #18561, .T. ) ;
#20352 = PRESENTATION_STYLE_ASSIGNMENT (( #23545 ) ) ;
#20353 = EDGE_CURVE ( 'NONE', #42231, #44962, #28249, .T. ) ;
#20354 = CYLINDRICAL_SURFACE ( 'NONE', #35491, 82.00000000000000000 ) ;
#20355 = DIRECTION ( 'NONE',  ( 0.000000000000000000, 0.000000000000000000, 1.000000000000000000 ) ) ;
#20356 = VERTEX_POINT ( 'NONE', #29357 ) ;
#20357 = DIRECTION ( 'NONE',  ( 1.000000000000000000, 0.000000000000000000, 0.000000000000000000 ) ) ;
#20358 = ORIENTED_EDGE ( 'NONE', *, *, #43298, .F. ) ;
#20359 = VERTEX_POINT ( 'NONE', #22728 ) ;
#20360 = PLANE ( 'NONE',  #17327 ) ;
#20361 = DIRECTION ( 'NONE',  ( 0.000000000000000000, 0.000000000000000000, -1.000000000000000000 ) ) ;
#20362 = CARTESIAN_POINT ( 'NONE',  ( 10.00000000000000000, 0.000000000000000000, 0.000000000000000000 ) ) ;
#20363 = PLANE ( 'NONE',  #2476 ) ;
#20364 = VECTOR ( 'NONE', #1060, 1000.000000000000000 ) ;
#20365 = DIRECTION ( 'NONE',  ( 1.000000000000000000, 0.000000000000000000, 0.000000000000000000 ) ) ;
#20366 = VERTEX_POINT ( 'NONE', #3888 ) ;
#20367 = VECTOR ( 'NONE', #2361, 1000.000000000000114 ) ;
#20368 = CARTESIAN_POINT ( 'NONE',  ( 5.000000000000000000, 71.21200624218795383, 40.65526001592638039 ) ) ;
#20369 = EDGE_LOOP ( 'NONE', ( #7131, #31883, #4083, #19722 ) ) ;
#20370 = EDGE_LOOP ( 'NONE', ( #30596, #11361, #35690, #14216 ) ) ;
#20371 = ADVANCED_FACE ( 'NONE', ( #44516 ), #10993, .T. ) ;
#20372 = CARTESIAN_POINT ( 'NONE',  ( 0.000000000000000000, 30.80686688397041451, -21.53537804866048688 ) ) ;
#20373 = ORIENTED_EDGE ( 'NONE', *, *, #16636, .F. ) ;
#20374 = EDGE_CURVE ( 'NONE', #28683, #16330, #15158, .T. ) ;
#20375 = DIRECTION ( 'NONE',  ( -1.000000000000000000, 0.000000000000000000, 0.000000000000000000 ) ) ;
#20376 = CYLINDRICAL_SURFACE ( 'NONE', #13338, 16.00000000000000000 ) ;
#20377 = DIRECTION ( 'NONE',  ( 0.000000000000000000, 0.000000000000000000, 1.000000000000000000 ) ) ;
#20378 = ORIENTED_EDGE ( 'NONE', *, *, #6469, .T. ) ;
#20379 = LINE ( 'NONE', #20150, #2612 ) ;
#20380 = LINE ( 'NONE', #13529, #23710 ) ;
#20381 = EDGE_CURVE ( 'NONE', #36999, #18005, #26414, .T. ) ;
#20382 = DIRECTION ( 'NONE',  ( 0.000000000000000000, 0.000000000000000000, 1.000000000000000000 ) ) ;
#20383 = VECTOR ( 'NONE', #15463, 1000.000000000000000 ) ;
#20384 = DIRECTION ( 'NONE',  ( -1.000000000000000000, -0.000000000000000000, 0.000000000000000000 ) ) ;
#20385 = DIRECTION ( 'NONE',  ( 0.000000000000000000, -1.000000000000000000, -1.040834085586084257E-14 ) ) ;
#20386 = EDGE_CURVE ( 'NONE', #7735, #2104, #45015, .T. ) ;
#20387 = DIRECTION ( 'NONE',  ( 0.000000000000000000, -0.1564344650402170744, -0.9876883405951398798 ) ) ;
#20389 = EDGE_CURVE ( 'NONE', #15559, #10554, #12602, .T. ) ;
#20388 = CARTESIAN_POINT ( 'NONE',  ( 15.00000000000000000, 26.49999999999999645, 1.499999999999995781 ) ) ;
#20390 = CARTESIAN_POINT ( 'NONE',  ( 11.99999999999999822, 0.000000000000000000, 0.000000000000000000 ) ) ;
#20391 = CYLINDRICAL_SURFACE ( 'NONE', #13493, 37.49900000000000233 ) ;
#20392 = CARTESIAN_POINT ( 'NONE',  ( 10.00000000000000000, 21.40280677340421533, -36.13751322684397138 ) ) ;
#20393 = ORIENTED_EDGE ( 'NONE', *, *, #33417, .F. ) ;
#20394 = ORIENTED_EDGE ( 'NONE', *, *, #11672, .F. ) ;
#20395 = DIRECTION ( 'NONE',  ( -1.000000000000000000, 0.000000000000000000, -0.000000000000000000 ) ) ;
#20396 = ORIENTED_EDGE ( 'NONE', *, *, #23252, .F. ) ;
#20397 = CARTESIAN_POINT ( 'NONE',  ( -23.97194136764370498, -131.3950000906648938, 5.500000000000000000 ) ) ;
#20398 = CARTESIAN_POINT ( 'NONE',  ( 5.000000000000002665, -44.99326035066006568, -68.55367621811190304 ) ) ;
#20399 = VERTEX_POINT ( 'NONE', #15402 ) ;
#20400 = ADVANCED_FACE ( 'NONE', ( #26651 ), #6840, .F. ) ;
#20401 = VECTOR ( 'NONE', #25297, 1000.000000000000000 ) ;
#20402 = AXIS2_PLACEMENT_3D ( 'NONE', #21033, #2915, #2427 ) ;
#20403 = AXIS2_PLACEMENT_3D ( 'NONE', #47407, #6294, #6775 ) ;
#20404 = VERTEX_POINT ( 'NONE', #33266 ) ;
#20405 = DIRECTION ( 'NONE',  ( 0.000000000000000000, 0.000000000000000000, 1.000000000000000000 ) ) ;
#20406 = ORIENTED_EDGE ( 'NONE', *, *, #18711, .T. ) ;
#20407 = ORIENTED_EDGE ( 'NONE', *, *, #9291, .T. ) ;
#20408 = ADVANCED_FACE ( 'NONE', ( #14673 ), #29589, .T. ) ;
#20409 = ORIENTED_EDGE ( 'NONE', *, *, #38852, .T. ) ;
#20410 = AXIS2_PLACEMENT_3D ( 'NONE', #32308, #24950, #46769 ) ;
#20411 = CIRCLE ( 'NONE', #46219, 16.00000000000000000 ) ;
#20412 = DIRECTION ( 'NONE',  ( 0.000000000000000000, -0.9945218953682732899, 0.1045284632676548031 ) ) ;
#20413 = DIRECTION ( 'NONE',  ( 0.000000000000000000, 0.000000000000000000, 1.000000000000000000 ) ) ;
#20414 = CARTESIAN_POINT ( 'NONE',  ( 0.000000000000000000, 0.000000000000000000, 0.000000000000000000 ) ) ;
#20415 = CIRCLE ( 'NONE', #47773, 77.49900000000000944 ) ;
#20416 = ORIENTED_EDGE ( 'NONE', *, *, #33757, .F. ) ;
#20417 = DIRECTION ( 'NONE',  ( -1.000000000000000000, -0.000000000000000000, -0.000000000000000000 ) ) ;
#20418 = ORIENTED_EDGE ( 'NONE', *, *, #18477, .T. ) ;
#20419 = FACE_OUTER_BOUND ( 'NONE', #25528, .T. ) ;
#20420 = CARTESIAN_POINT ( 'NONE',  ( 0.000000000000000000, -41.76106447765443619, -62.50884508063471401 ) ) ;
#20421 = DIRECTION ( 'NONE',  ( -0.6575728627325955200, 0.7533909544171997208, 0.000000000000000000 ) ) ;
#20422 = AXIS2_PLACEMENT_3D ( 'NONE', #45090, #31315, #4869 ) ;
#20423 = ORIENTED_EDGE ( 'NONE', *, *, #40565, .T. ) ;
#20424 = EDGE_LOOP ( 'NONE', ( #11242, #4422, #25353, #39272 ) ) ;
#20425 = ORIENTED_EDGE ( 'NONE', *, *, #44542, .F. ) ;
#20426 = CARTESIAN_POINT ( 'NONE',  ( 0.000000000000000000, 0.000000000000000000, 0.000000000000000000 ) ) ;
#20427 = ORIENTED_EDGE ( 'NONE', *, *, #19755, .T. ) ;
#20428 = ADVANCED_FACE ( 'NONE', ( #22255 ), #37178, .F. ) ;
#20429 = DIRECTION ( 'NONE',  ( 0.000000000000000000, 0.000000000000000000, 1.000000000000000000 ) ) ;
#20430 = DIRECTION ( 'NONE',  ( 0.000000000000000000, -0.3090169943749349057, -0.9510565162951577500 ) ) ;
#20431 = CARTESIAN_POINT ( 'NONE',  ( 10.00000000000000000, -73.95703589263958122, -23.16143007188506431 ) ) ;
#20432 = CARTESIAN_POINT ( 'NONE',  ( 10.00000000000000000, -37.58145647212453611, -0.6853352020794456489 ) ) ;
#20433 = PLANE ( 'NONE',  #40686 ) ;
#20434 = EDGE_CURVE ( 'NONE', #38924, #7360, #38152, .T. ) ;
#20435 = CARTESIAN_POINT ( 'NONE',  ( 0.000000000000000000, -16.65972982744991882, 80.28980883073752750 ) ) ;
#20436 = CARTESIAN_POINT ( 'NONE',  ( -3.000000000000000000, 0.000000000000000000, 0.000000000000000000 ) ) ;
#20437 = ORIENTED_EDGE ( 'NONE', *, *, #1513, .F. ) ;
#20438 = CYLINDRICAL_SURFACE ( 'NONE', #14877, 13.90444123027096879 ) ;
#20439 = DIRECTION ( 'NONE',  ( 0.000000000000000000, 0.000000000000000000, 1.000000000000000000 ) ) ;
#20440 = AXIS2_PLACEMENT_3D ( 'NONE', #24135, #39066, #5529 ) ;
#20441 = DIRECTION ( 'NONE',  ( 0.000000000000000000, 0.000000000000000000, -1.000000000000000000 ) ) ;
#20442 = FACE_OUTER_BOUND ( 'NONE', #21745, .T. ) ;
#20443 = ORIENTED_EDGE ( 'NONE', *, *, #22330, .F. ) ;
#20444 = VERTEX_POINT ( 'NONE', #5349 ) ;
#20446 = ADVANCED_FACE ( 'NONE', ( #27617 ), #12219, .F. ) ;
#20445 = DIRECTION ( 'NONE',  ( 0.000000000000000000, 0.000000000000000000, -1.000000000000000000 ) ) ;
#20447 = CIRCLE ( 'NONE', #37676, 31.99999999999998579 ) ;
#20449 = EDGE_CURVE ( 'NONE', #26893, #34798, #30590, .T. ) ;
#20448 = ADVANCED_BREP_SHAPE_REPRESENTATION ( '', ( #19105, #11636 ), #21023 ) ;
#20450 = CARTESIAN_POINT ( 'NONE',  ( 10.00000000000000000, 12.93880638057314059, 76.41127070299278046 ) ) ;
#20451 = DIRECTION ( 'NONE',  ( 0.000000000000000000, 0.000000000000000000, 1.000000000000000000 ) ) ;
#20452 = AXIS2_PLACEMENT_3D ( 'NONE', #38524, #24081, #5716 ) ;
#20453 = VECTOR ( 'NONE', #28587, 1000.000000000000000 ) ;
#20454 = DIRECTION ( 'NONE',  ( 0.000000000000000000, 0.000000000000000000, -1.000000000000000000 ) ) ;
#20455 = DIRECTION ( 'NONE',  ( 0.000000000000000000, 0.7604059656000322631, -0.6494480483301821039 ) ) ;
#20456 = CARTESIAN_POINT ( 'NONE',  ( 0.000000000000000000, 0.000000000000000000, 0.000000000000000000 ) ) ;
#20457 = PLANE ( 'NONE',  #44105 ) ;
#20458 = ORIENTED_EDGE ( 'NONE', *, *, #15103, .F. ) ;
#20459 = CARTESIAN_POINT ( 'NONE',  ( 0.000000000000000000, -35.47612816024539484, 22.48208911017487921 ) ) ;
#20460 = AXIS2_PLACEMENT_3D ( 'NONE', #42058, #16584, #35178 ) ;
#20461 = EDGE_LOOP ( 'NONE', ( #31726, #37849, #38446, #47881 ) ) ;
#20462 = SURFACE_STYLE_USAGE ( .BOTH. , #35150 ) ;
#20463 = DIRECTION ( 'NONE',  ( 0.000000000000000000, 0.07845909572783793529, 0.9969173337331285190 ) ) ;
#20464 = ORIENTED_EDGE ( 'NONE', *, *, #11947, .T. ) ;
#20465 = VERTEX_POINT ( 'NONE', #45986 ) ;
#20466 = ORIENTED_EDGE ( 'NONE', *, *, #16272, .T. ) ;
#20467 = ORIENTED_EDGE ( 'NONE', *, *, #13515, .F. ) ;
#20468 = DIRECTION ( 'NONE',  ( -0.02332147558787930897, -0.9997280174009348652, 0.000000000000000000 ) ) ;
#20469 = ORIENTED_EDGE ( 'NONE', *, *, #13594, .F. ) ;
#20470 = ORIENTED_EDGE ( 'NONE', *, *, #19696, .T. ) ;
#20471 = AXIS2_PLACEMENT_3D ( 'NONE', #5299, #20215, #35137 ) ;
#20472 = EDGE_CURVE ( 'NONE', #1784, #12338, #15738, .T. ) ;
#20473 = DIRECTION ( 'NONE',  ( -1.000000000000000000, 0.000000000000000000, 0.000000000000000000 ) ) ;
#20474 = VECTOR ( 'NONE', #25174, 1000.000000000000000 ) ;
#20475 = CARTESIAN_POINT ( 'NONE',  ( 10.00000000000000000, 30.80686688397041451, -21.53537804866048688 ) ) ;
#20476 = EDGE_CURVE ( 'NONE', #39544, #28423, #7102, .T. ) ;
#20477 = EDGE_LOOP ( 'NONE', ( #21431, #9881, #7709, #43735 ) ) ;
#20478 = ORIENTED_EDGE ( 'NONE', *, *, #25070, .T. ) ;
#20479 = CIRCLE ( 'NONE', #26747, 31.99999999999998579 ) ;
#20480 = CARTESIAN_POINT ( 'NONE',  ( 0.000000000000000000, 0.000000000000000000, 0.000000000000000000 ) ) ;
#20482 = ORIENTED_EDGE ( 'NONE', *, *, #14549, .F. ) ;
#20481 = CARTESIAN_POINT ( 'NONE',  ( 0.000000000000000000, 0.000000000000000000, 40.80000000000001847 ) ) ;
#20483 = CYLINDRICAL_SURFACE ( 'NONE', #112, 16.00000000000000000 ) ;
#20484 = EDGE_LOOP ( 'NONE', ( #46254, #1109, #22771, #14399 ) ) ;
#20485 = ORIENTED_EDGE ( 'NONE', *, *, #22923, .F. ) ;
#20486 = CARTESIAN_POINT ( 'NONE',  ( -3.360000000000002096, 0.000000000000000000, 0.000000000000000000 ) ) ;
#20487 = EDGE_LOOP ( 'NONE', ( #6533, #37584, #38427, #31868 ) ) ;
#20488 = VERTEX_POINT ( 'NONE', #27145 ) ;
#20489 = DIRECTION ( 'NONE',  ( 0.000000000000000000, 0.000000000000000000, 1.000000000000000000 ) ) ;
#20490 = CARTESIAN_POINT ( 'NONE',  ( 11.99999999999999822, 0.000000000000000000, 0.000000000000000000 ) ) ;
#20491 = CIRCLE ( 'NONE', #21250, 42.00000000000000000 ) ;
#20492 = DIRECTION ( 'NONE',  ( -1.000000000000000000, 0.000000000000000000, 0.000000000000000000 ) ) ;
#20493 = CARTESIAN_POINT ( 'NONE',  ( 10.00000000000000000, 0.000000000000000000, 0.000000000000000000 ) ) ;
#20494 = EDGE_CURVE ( 'NONE', #44222, #40154, #12452, .T. ) ;
#20495 = DIRECTION ( 'NONE',  ( 0.000000000000000000, -0.7431448254773938000, -0.6691306063588585706 ) ) ;
#20496 = EDGE_LOOP ( 'NONE', ( #25345, #46856, #29047, #36828 ) ) ;
#20497 = EDGE_CURVE ( 'NONE', #43945, #27073, #31304, .T. ) ;
#20498 = ADVANCED_FACE ( 'NONE', ( #46221 ), #35190, .T. ) ;
#20499 = VERTEX_POINT ( 'NONE', #23693 ) ;
#20500 = CARTESIAN_POINT ( 'NONE',  ( 11.99999999999999822, -21.60688246758642705, 79.10210256391358996 ) ) ;
#20501 = CARTESIAN_POINT ( 'NONE',  ( 5.000000000000000000, -31.52238457039579345, -27.75498641678775158 ) ) ;
#20502 = ORIENTED_EDGE ( 'NONE', *, *, #2575, .F. ) ;
#20504 = EDGE_CURVE ( 'NONE', #35598, #17038, #46468, .T. ) ;
#20503 = DIRECTION ( 'NONE',  ( 0.000000000000000000, -0.8910065241883626808, -0.4539904997395569075 ) ) ;
#20505 = VERTEX_POINT ( 'NONE', #12942 ) ;
#20506 = CARTESIAN_POINT ( 'NONE',  ( 0.000000000000000000, -10.41901085202107247, 40.68715046381925049 ) ) ;
#20507 = DIRECTION ( 'NONE',  ( 0.000000000000000000, 0.000000000000000000, 1.000000000000000000 ) ) ;
#20508 = DIRECTION ( 'NONE',  ( -0.000000000000000000, -0.000000000000000000, 1.000000000000000000 ) ) ;
#20509 = EDGE_CURVE ( 'NONE', #2989, #38555, #41582, .T. ) ;
#20510 = ORIENTED_EDGE ( 'NONE', *, *, #4114, .F. ) ;
#20511 = DIRECTION ( 'NONE',  ( -1.000000000000000000, 0.000000000000000000, 0.000000000000000000 ) ) ;
#20512 = PRESENTATION_STYLE_ASSIGNMENT (( #24430 ) ) ;
#20514 = AXIS2_PLACEMENT_3D ( 'NONE', #11076, #18153, #22075 ) ;
#20513 = DIRECTION ( 'NONE',  ( -1.000000000000000000, -0.000000000000000000, -0.000000000000000000 ) ) ;
#20516 = ORIENTED_EDGE ( 'NONE', *, *, #28293, .T. ) ;
#20515 = CIRCLE ( 'NONE', #5673, 16.00000000000000355 ) ;
#20517 = DIRECTION ( 'NONE',  ( 1.000000000000000000, 0.000000000000000000, 0.000000000000000000 ) ) ;
#20518 = DIRECTION ( 'NONE',  ( 0.000000000000000000, 0.000000000000000000, -1.000000000000000000 ) ) ;
#20519 = DIRECTION ( 'NONE',  ( 0.000000000000000000, 0.000000000000000000, -1.000000000000000000 ) ) ;
#20520 = AXIS2_PLACEMENT_3D ( 'NONE', #20258, #24180, #12686 ) ;
#20521 = CARTESIAN_POINT ( 'NONE',  ( 0.000000000000000000, -34.94270380257692921, 74.18225833017875459 ) ) ;
#20522 = SHAPE_DEFINITION_REPRESENTATION ( #14010, #5957 ) ;
#20523 = ORIENTED_EDGE ( 'NONE', *, *, #18608, .T. ) ;
#20524 = ORIENTED_EDGE ( 'NONE', *, *, #39805, .T. ) ;
#20525 = ORIENTED_EDGE ( 'NONE', *, *, #30845, .T. ) ;
#20526 = VECTOR ( 'NONE', #35393, 1000.000000000000000 ) ;
#20527 = DIRECTION ( 'NONE',  ( 0.000000000000000000, 0.000000000000000000, 1.000000000000000000 ) ) ;
#20528 = CARTESIAN_POINT ( 'NONE',  ( 0.000000000000000000, 35.95386929396256903, -10.96151621346501237 ) ) ;
#20529 = EDGE_LOOP ( 'NONE', ( #38885, #27303, #20022, #38419 ) ) ;
#20530 = EDGE_CURVE ( 'NONE', #1080, #36243, #23954, .T. ) ;
#20531 = CARTESIAN_POINT ( 'NONE',  ( -10.00000000000000000, 0.000000000000000000, 0.000000000000000000 ) ) ;
#20532 = EDGE_CURVE ( 'NONE', #45521, #16029, #25098, .T. ) ;
#20533 = ORIENTED_EDGE ( 'NONE', *, *, #28958, .F. ) ;
#20534 = EDGE_LOOP ( 'NONE', ( #16035, #38492, #25539, #37460 ) ) ;
#20535 = ORIENTED_EDGE ( 'NONE', *, *, #23791, .F. ) ;
#20536 = EDGE_CURVE ( 'NONE', #34175, #1618, #37912, .T. ) ;
#20537 = VECTOR ( 'NONE', #23526, 1000.000000000000000 ) ;
#20538 = AXIS2_PLACEMENT_3D ( 'NONE', #27201, #19830, #8102 ) ;
#20539 = CARTESIAN_POINT ( 'NONE',  ( 0.000000000000000000, 26.01480285779933510, -70.53064760720289428 ) ) ;
#20540 = ORIENTED_EDGE ( 'NONE', *, *, #4322, .T. ) ;
#20541 = DIRECTION ( 'NONE',  ( -1.000000000000000000, 0.000000000000000000, -0.000000000000000000 ) ) ;
#20542 = VERTEX_POINT ( 'NONE', #41829 ) ;
#20543 = DIRECTION ( 'NONE',  ( 0.000000000000000000, 0.000000000000000000, 1.000000000000000000 ) ) ;
#20544 = FACE_OUTER_BOUND ( 'NONE', #31800, .T. ) ;
#20545 = CARTESIAN_POINT ( 'NONE',  ( 11.99999999999999822, 0.000000000000000000, 0.000000000000000000 ) ) ;
#20546 = CIRCLE ( 'NONE', #12738, 31.99999999999999289 ) ;
#20547 = ORIENTED_EDGE ( 'NONE', *, *, #37459, .F. ) ;
#20548 = ADVANCED_FACE ( 'NONE', ( #34222 ), #693, .F. ) ;
#20549 = CARTESIAN_POINT ( 'NONE',  ( 0.000000000000000000, 0.000000000000000000, 0.000000000000000000 ) ) ;
#20550 = ADVANCED_FACE ( 'NONE', ( #11965 ), #34953, .T. ) ;
#20551 = ORIENTED_EDGE ( 'NONE', *, *, #34429, .F. ) ;
#20552 = DIRECTION ( 'NONE',  ( -1.000000000000000000, 0.000000000000000000, 0.000000000000000000 ) ) ;
#20553 = LINE ( 'NONE', #13227, #6347 ) ;
#20554 = CIRCLE ( 'NONE', #8049, 42.00000000000000000 ) ;
#20555 = CARTESIAN_POINT ( 'NONE',  ( 10.00000000000000000, 0.000000000000000000, 0.000000000000000000 ) ) ;
#20556 = ORIENTED_EDGE ( 'NONE', *, *, #44991, .F. ) ;
#20557 = ORIENTED_EDGE ( 'NONE', *, *, #1437, .T. ) ;
#20558 = CARTESIAN_POINT ( 'NONE',  ( -10.90076147243505211, 0.000000000000000000, 13.71319123027096865 ) ) ;
#20559 = CARTESIAN_POINT ( 'NONE',  ( -10.00000000000000000, 0.000000000000000000, 0.000000000000000000 ) ) ;
#20560 = ORIENTED_EDGE ( 'NONE', *, *, #8962, .T. ) ;
#20561 = CIRCLE ( 'NONE', #8819, 42.00000000000000000 ) ;
#20562 = DIRECTION ( 'NONE',  ( 0.000000000000000000, 0.9945218953682732899, -0.1045284632676548031 ) ) ;
#20563 = CARTESIAN_POINT ( 'NONE',  ( 12.50000000000000000, -132.5000000000000000, -40.00000000000000000 ) ) ;
#20564 = CARTESIAN_POINT ( 'NONE',  ( 11.99999999999999822, -26.02418014898359289, 70.52718814184250107 ) ) ;
#20565 = DIRECTION ( 'NONE',  ( -1.000000000000000000, -0.000000000000000000, -0.000000000000000000 ) ) ;
#20566 = DIRECTION ( 'NONE',  ( 1.000000000000000000, -0.000000000000000000, -0.000000000000000000 ) ) ;
#20567 = EDGE_CURVE ( 'NONE', #37030, #44743, #45741, .T. ) ;
#20568 = CARTESIAN_POINT ( 'NONE',  ( -3.000000000000000000, -25.60904388321925396, 6.976881207771172377 ) ) ;
#20569 = EDGE_LOOP ( 'NONE', ( #7826, #20197, #25957, #25662 ) ) ;
#20570 = CARTESIAN_POINT ( 'NONE',  ( 10.00000000000000000, 65.64334221924909230, 41.19522573413756561 ) ) ;
#20571 = DIRECTION ( 'NONE',  ( 0.000000000000000000, -0.5000000000000046629, 0.8660254037844359321 ) ) ;
#20572 = CARTESIAN_POINT ( 'NONE',  ( 0.000000000000000000, 0.000000000000000000, 0.000000000000000000 ) ) ;
#20573 = CYLINDRICAL_SURFACE ( 'NONE', #47140, 31.99999999999999289 ) ;
#20574 = LINE ( 'NONE', #13245, #15993 ) ;
#20576 = AXIS2_PLACEMENT_3D ( 'NONE', #35993, #2229, #36235 ) ;
#20575 = LINE ( 'NONE', #16916, #46011 ) ;
#20577 = DIRECTION ( 'NONE',  ( -0.000000000000000000, -0.000000000000000000, 1.000000000000000000 ) ) ;
#20578 = DIRECTION ( 'NONE',  ( 0.000000000000000000, 0.9876883405951383255, -0.1564344650402277048 ) ) ;
#20579 = ORIENTED_EDGE ( 'NONE', *, *, #4980, .F. ) ;
#20580 = VECTOR ( 'NONE', #4410, 1000.000000000000000 ) ;
#20581 = ORIENTED_EDGE ( 'NONE', *, *, #24257, .F. ) ;
#20582 = CARTESIAN_POINT ( 'NONE',  ( 10.00000000000000000, 0.000000000000000000, 0.000000000000000000 ) ) ;
#20583 = DIRECTION ( 'NONE',  ( -1.000000000000000000, 0.000000000000000000, 0.000000000000000000 ) ) ;
#20584 = AXIS2_PLACEMENT_3D ( 'NONE', #10080, #32593, #24999 ) ;
#20585 = DIRECTION ( 'NONE',  ( 0.6862798483830554463, 0.7273375899149793211, -0.000000000000000000 ) ) ;
#20586 = VECTOR ( 'NONE', #2567, 1000.000000000000000 ) ;
#20587 = ORIENTED_EDGE ( 'NONE', *, *, #38760, .T. ) ;
#20588 = ADVANCED_FACE ( 'NONE', ( #2868 ), #24184, .T. ) ;
#20589 = VECTOR ( 'NONE', #30656, 1000.000000000000000 ) ;
#20590 = AXIS2_PLACEMENT_3D ( 'NONE', #37320, #37556, #22140 ) ;
#20591 = VERTEX_POINT ( 'NONE', #35913 ) ;
#20592 = CIRCLE ( 'NONE', #47942, 42.00000000000000000 ) ;
#20593 = CARTESIAN_POINT ( 'NONE',  ( 0.000000000000000000, 15.48615015657581750, 39.04073710021349797 ) ) ;
#20594 = CIRCLE ( 'NONE', #22138, 31.99999999999998934 ) ;
#20595 = VERTEX_POINT ( 'NONE', #39114 ) ;
#20596 = DIRECTION ( 'NONE',  ( -1.000000000000000000, 0.000000000000000000, 0.000000000000000000 ) ) ;
#20597 = EDGE_CURVE ( 'NONE', #1742, #40355, #17793, .T. ) ;
#20598 = ORIENTED_EDGE ( 'NONE', *, *, #3917, .F. ) ;
#20599 = DIRECTION ( 'NONE',  ( -1.000000000000000000, -0.000000000000000000, -0.000000000000000000 ) ) ;
#20600 = ADVANCED_FACE ( 'NONE', ( #35434 ), #20988, .T. ) ;
#20601 = DIRECTION ( 'NONE',  ( 0.000000000000000000, 0.000000000000000000, 1.000000000000000000 ) ) ;
#20602 = CARTESIAN_POINT ( 'NONE',  ( -10.00000000000000000, 0.000000000000000000, 0.000000000000000000 ) ) ;
#20603 = ORIENTED_EDGE ( 'NONE', *, *, #15202, .T. ) ;
#20604 = DIRECTION ( 'NONE',  ( -1.000000000000000000, 0.000000000000000000, -0.000000000000000000 ) ) ;
#20605 = EDGE_LOOP ( 'NONE', ( #2959, #39169, #33193, #4443 ) ) ;
#20606 = ORIENTED_EDGE ( 'NONE', *, *, #40519, .T. ) ;
#20607 = DIRECTION ( 'NONE',  ( 1.000000000000000000, 0.000000000000000000, 0.000000000000000000 ) ) ;
#20608 = ADVANCED_FACE ( 'NONE', ( #35689 ), #5839, .T. ) ;
#20609 = DIRECTION ( 'NONE',  ( -1.000000000000000000, -0.000000000000000000, 0.000000000000000000 ) ) ;
#20610 = DIRECTION ( 'NONE',  ( -1.000000000000000000, 0.000000000000000000, 0.000000000000000000 ) ) ;
#20611 = EDGE_CURVE ( 'NONE', #33987, #46736, #25134, .T. ) ;
#20612 = AXIS2_PLACEMENT_3D ( 'NONE', #16273, #38790, #35095 ) ;
#20613 = DIRECTION ( 'NONE',  ( 0.000000000000000000, 0.000000000000000000, 1.000000000000000000 ) ) ;
#20614 = VECTOR ( 'NONE', #9363, 1000.000000000000000 ) ;
#20615 = ORIENTED_EDGE ( 'NONE', *, *, #6821, .T. ) ;
#20616 = FACE_OUTER_BOUND ( 'NONE', #38877, .T. ) ;
#20617 = ORIENTED_EDGE ( 'NONE', *, *, #13483, .F. ) ;
#20618 = ORIENTED_EDGE ( 'NONE', *, *, #3989, .F. ) ;
#20619 = EDGE_CURVE ( 'NONE', #41225, #39728, #11869, .T. ) ;
#20620 = CIRCLE ( 'NONE', #45598, 16.00000000000000000 ) ;
#20621 = FACE_OUTER_BOUND ( 'NONE', #26812, .T. ) ;
#20622 = AXIS2_PLACEMENT_3D ( 'NONE', #31733, #27319, #24124 ) ;
#20623 = VECTOR ( 'NONE', #32216, 1000.000000000000000 ) ;
#20624 = CARTESIAN_POINT ( 'NONE',  ( 0.000000000000000000, 24.73286445877808148, -73.44644590900034586 ) ) ;
#20625 = CARTESIAN_POINT ( 'NONE',  ( 11.99999999999999822, 16.65972982745045528, -80.28980883073741381 ) ) ;
#20626 = DIRECTION ( 'NONE',  ( 0.000000000000000000, 0.000000000000000000, 1.000000000000000000 ) ) ;
#20627 = ORIENTED_EDGE ( 'NONE', *, *, #45939, .T. ) ;
#20628 = CARTESIAN_POINT ( 'NONE',  ( 10.00000000000000000, -25.88420570971381807, -27.13269053701123212 ) ) ;
#20629 = PRODUCT_DEFINITION_SHAPE ( 'NONE', 'NONE',  #29525 ) ;
#20630 = CYLINDRICAL_SURFACE ( 'NONE', #6492, 31.99999999999998579 ) ;
#20631 = DIRECTION ( 'NONE',  ( 0.000000000000000000, 0.000000000000000000, 1.000000000000000000 ) ) ;
#20632 = CYLINDRICAL_SURFACE ( 'NONE', #4900, 77.49899999999999523 ) ;
#20633 = EDGE_CURVE ( 'NONE', #6477, #33547, #21471, .T. ) ;
#20634 = CARTESIAN_POINT ( 'NONE',  ( 10.00000000000000000, 0.000000000000000000, 0.000000000000000000 ) ) ;
#20635 = VECTOR ( 'NONE', #42045, 1000.000000000000000 ) ;
#20636 = CARTESIAN_POINT ( 'NONE',  ( 12.00000000000000000, -11.95096189432345923, -23.69967320028757030 ) ) ;
#20637 = CARTESIAN_POINT ( 'NONE',  ( 0.000000000000000000, 0.000000000000000000, 0.000000000000000000 ) ) ;
#20638 = CARTESIAN_POINT ( 'NONE',  ( 10.00000000000000000, 26.01480285779837232, 70.53064760720326376 ) ) ;
#20639 = AXIS2_PLACEMENT_3D ( 'NONE', #35199, #1195, #8526 ) ;
#20640 = AXIS2_PLACEMENT_3D ( 'NONE', #11747, #30841, #11994 ) ;
#20641 = AXIS2_PLACEMENT_3D ( 'NONE', #41235, #4023, #25557 ) ;
#20642 = DIRECTION ( 'NONE',  ( 0.000000000000000000, 0.000000000000000000, 1.000000000000000000 ) ) ;
#20643 = LINE ( 'NONE', #2061, #10472 ) ;
#20644 = AXIS2_PLACEMENT_3D ( 'NONE', #3192, #29404, #44327 ) ;
#20645 = VERTEX_POINT ( 'NONE', #46713 ) ;
#20646 = LINE ( 'NONE', #24807, #4294 ) ;
#20647 = ORIENTED_EDGE ( 'NONE', *, *, #38577, .T. ) ;
#20648 = DIRECTION ( 'NONE',  ( -1.000000000000000000, 0.000000000000000000, 0.000000000000000000 ) ) ;
#20649 = DIRECTION ( 'NONE',  ( 0.000000000000000000, -0.6494480483301903195, 0.7604059656000251577 ) ) ;
#20650 = VERTEX_POINT ( 'NONE', #13651 ) ;
#20651 = CIRCLE ( 'NONE', #22201, 77.49900000000000944 ) ;
#20652 = VECTOR ( 'NONE', #28483, 1000.000000000000000 ) ;
#20653 = CARTESIAN_POINT ( 'NONE',  ( -10.00000000000000000, 0.000000000000000000, 0.000000000000000000 ) ) ;
#20654 = EDGE_CURVE ( 'NONE', #8389, #36993, #1925, .T. ) ;
#20655 = VERTEX_POINT ( 'NONE', #39842 ) ;
#20656 = AXIS2_PLACEMENT_3D ( 'NONE', #1777, #27493, #46324 ) ;
#20657 = ORIENTED_EDGE ( 'NONE', *, *, #48208, .F. ) ;
#20658 = ADVANCED_FACE ( 'NONE', ( #13171 ), #36402, .F. ) ;
#20659 = EDGE_LOOP ( 'NONE', ( #36103, #26147, #28629, #3013 ) ) ;
#20660 = EDGE_CURVE ( 'NONE', #19709, #42524, #8709, .T. ) ;
#20661 = EDGE_CURVE ( 'NONE', #11933, #15480, #24370, .T. ) ;
#20662 = VECTOR ( 'NONE', #850, 1000.000000000000000 ) ;
#20663 = VECTOR ( 'NONE', #44057, 1000.000000000000114 ) ;
#20664 = PLANE ( 'NONE',  #45622 ) ;
#20665 = EDGE_CURVE ( 'NONE', #7974, #42505, #2608, .T. ) ;
#20666 = VECTOR ( 'NONE', #31807, 1000.000000000000000 ) ;
#20667 = CARTESIAN_POINT ( 'NONE',  ( 0.000000000000000000, 71.91182617369187824, 28.89263327155770256 ) ) ;
#20668 = AXIS2_PLACEMENT_3D ( 'NONE', #29331, #39645, #6105 ) ;
#20669 = CARTESIAN_POINT ( 'NONE',  ( 10.00000000000000000, -46.54456581323762521, -59.03342792756313884 ) ) ;
#20670 = ORIENTED_EDGE ( 'NONE', *, *, #33105, .T. ) ;
#20671 = DIRECTION ( 'NONE',  ( 0.000000000000000000, -0.6691306063588672304, 0.7431448254773862505 ) ) ;
#20672 = ORIENTED_EDGE ( 'NONE', *, *, #46487, .T. ) ;
#20673 = ORIENTED_EDGE ( 'NONE', *, *, #18887, .F. ) ;
#20674 = VECTOR ( 'NONE', #31008, 1000.000000000000227 ) ;
#20675 = DIRECTION ( 'NONE',  ( 0.000000000000000000, 0.000000000000000000, -1.000000000000000000 ) ) ;
#20676 = CARTESIAN_POINT ( 'NONE',  ( -0.9515373497862389396, -96.47140937769621871, 2.500000000000000000 ) ) ;
#20677 = CARTESIAN_POINT ( 'NONE',  ( 0.000000000000000000, 0.000000000000000000, 0.000000000000000000 ) ) ;
#20678 = ORIENTED_EDGE ( 'NONE', *, *, #22471, .F. ) ;
#20679 = ORIENTED_EDGE ( 'NONE', *, *, #34911, .T. ) ;
#20680 = ORIENTED_EDGE ( 'NONE', *, *, #9482, .T. ) ;
#20681 = CARTESIAN_POINT ( 'NONE',  ( 15.00000000000000000, -19.89357724625003598, -12.59942793731059041 ) ) ;
#20682 = ORIENTED_EDGE ( 'NONE', *, *, #2335, .T. ) ;
#20683 = EDGE_CURVE ( 'NONE', #6225, #32049, #24901, .T. ) ;
#20684 = DIRECTION ( 'NONE',  ( 0.000000000000000000, 0.000000000000000000, 1.000000000000000000 ) ) ;
#20685 = CARTESIAN_POINT ( 'NONE',  ( -3.000000000000000000, -18.13022148937263012, 15.02647892043544608 ) ) ;
#20686 = DIRECTION ( 'NONE',  ( 0.7533909544171997208, 0.6575728627325956310, -6.162975822039155825E-32 ) ) ;
#20687 = DIRECTION ( 'NONE',  ( 0.000000000000000000, -0.1045284632676436454, 0.9945218953682744001 ) ) ;
#20688 = CARTESIAN_POINT ( 'NONE',  ( 10.00000000000000000, 0.000000000000000000, 0.000000000000000000 ) ) ;
#20689 = DIRECTION ( 'NONE',  ( 1.000000000000000000, 0.000000000000000000, 0.000000000000000000 ) ) ;
#20690 = CARTESIAN_POINT ( 'NONE',  ( 16.84844760790522145, -103.5491698323862124, -2.500000000000000000 ) ) ;
#20691 = CYLINDRICAL_SURFACE ( 'NONE', #27758, 16.00000000000000000 ) ;
#20692 = DIRECTION ( 'NONE',  ( -1.000000000000000000, 0.000000000000000000, 0.000000000000000000 ) ) ;
#20693 = ADVANCED_FACE ( 'NONE', ( #47422 ), #43746, .T. ) ;
#20694 = AXIS2_PLACEMENT_3D ( 'NONE', #37917, #1680, #23959 ) ;
#20695 = DIRECTION ( 'NONE',  ( 0.000000000000000000, 0.000000000000000000, 1.000000000000000000 ) ) ;
#20696 = EDGE_LOOP ( 'NONE', ( #43719, #45972, #8561, #10352 ) ) ;
#20697 = VERTEX_POINT ( 'NONE', #16851 ) ;
#20698 = DIRECTION ( 'NONE',  ( 0.000000000000000000, 0.2079116908177525702, 0.9781476007338071321 ) ) ;
#20699 = CIRCLE ( 'NONE', #33204, 16.00000000000000000 ) ;
#20700 = CYLINDRICAL_SURFACE ( 'NONE', #43895, 77.49899999999999523 ) ;
#20701 = CYLINDRICAL_SURFACE ( 'NONE', #43288, 82.00000000000000000 ) ;
#20702 = FACE_OUTER_BOUND ( 'NONE', #28507, .T. ) ;
#20703 = CARTESIAN_POINT ( 'NONE',  ( -3.000000000000000000, -25.60904388321916159, -6.976881207771517879 ) ) ;
#20704 = EDGE_CURVE ( 'NONE', #23653, #41663, #7175, .T. ) ;
#20705 = ORIENTED_EDGE ( 'NONE', *, *, #36028, .T. ) ;
#20706 = AXIS2_PLACEMENT_3D ( 'NONE', #43904, #40485, #36556 ) ;
#20707 = AXIS2_PLACEMENT_3D ( 'NONE', #6747, #28063, #9441 ) ;
#20708 = DIRECTION ( 'NONE',  ( 0.000000000000000000, 0.7604059656000276002, 0.6494480483301875440 ) ) ;
#20709 = DIRECTION ( 'NONE',  ( 0.2867529058022035837, -0.9580045777625452175, 0.000000000000000000 ) ) ;
#20710 = ORIENTED_EDGE ( 'NONE', *, *, #45778, .F. ) ;
#20711 = VECTOR ( 'NONE', #15826, 1000.000000000000114 ) ;
#20712 = CARTESIAN_POINT ( 'NONE',  ( 10.00000000000000000, 0.000000000000000000, 0.000000000000000000 ) ) ;
#20713 = VECTOR ( 'NONE', #7628, 1000.000000000000000 ) ;
#20714 = ORIENTED_EDGE ( 'NONE', *, *, #10364, .F. ) ;
#20715 = DIRECTION ( 'NONE',  ( -1.000000000000000000, -0.000000000000000000, -0.000000000000000000 ) ) ;
#20716 = CIRCLE ( 'NONE', #41825, 37.49900000000000944 ) ;
#20717 = EDGE_LOOP ( 'NONE', ( #41397, #37026, #32582, #39339 ) ) ;
#20718 = ORIENTED_EDGE ( 'NONE', *, *, #6963, .T. ) ;
#20719 = EDGE_LOOP ( 'NONE', ( #3371, #576, #16931, #22294 ) ) ;
#20720 = EDGE_CURVE ( 'NONE', #1751, #36740, #26721, .T. ) ;
#20721 =( REPRESENTATION_RELATIONSHIP ('NONE','NONE', #5957, #21223 ) REPRESENTATION_RELATIONSHIP_WITH_TRANSFORMATION ( #2462 )SHAPE_REPRESENTATION_RELATIONSHIP( ) );
#20722 = EDGE_CURVE ( 'NONE', #21510, #29992, #39222, .T. ) ;
#20723 = ORIENTED_EDGE ( 'NONE', *, *, #25075, .T. ) ;
#20724 = VECTOR ( 'NONE', #41846, 1000.000000000000000 ) ;
#20725 = DIRECTION ( 'NONE',  ( 1.000000000000000000, 0.000000000000000000, 0.000000000000000000 ) ) ;
#20726 = ORIENTED_EDGE ( 'NONE', *, *, #15540, .F. ) ;
#20727 = EDGE_CURVE ( 'NONE', #13754, #24474, #44709, .T. ) ;
#20728 = ORIENTED_EDGE ( 'NONE', *, *, #28958, .T. ) ;
#20729 = VECTOR ( 'NONE', #2506, 1000.000000000000000 ) ;
#20730 = EDGE_CURVE ( 'NONE', #9234, #48128, #36071, .T. ) ;
#20731 = DIRECTION ( 'NONE',  ( -1.000000000000000000, 0.000000000000000000, 0.000000000000000000 ) ) ;
#20732 = AXIS2_PLACEMENT_3D ( 'NONE', #32658, #32894, #18688 ) ;
#20734 = ORIENTED_EDGE ( 'NONE', *, *, #38354, .T. ) ;
#20733 = CARTESIAN_POINT ( 'NONE',  ( 0.000000000000000000, -78.73519480814971416, 22.90783923731599359 ) ) ;
#20735 = ORIENTED_EDGE ( 'NONE', *, *, #18718, .T. ) ;
#20736 = VERTEX_POINT ( 'NONE', #7518 ) ;
#20737 = VERTEX_POINT ( 'NONE', #18751 ) ;
#20738 = CARTESIAN_POINT ( 'NONE',  ( 10.00000000000000000, 35.95386929396256903, -10.96151621346501237 ) ) ;
#20740 = ORIENTED_EDGE ( 'NONE', *, *, #10790, .T. ) ;
#20739 = FACE_OUTER_BOUND ( 'NONE', #39088, .T. ) ;
#20741 = DIRECTION ( 'NONE',  ( 0.000000000000000000, 0.000000000000000000, 1.000000000000000000 ) ) ;
#20742 = AXIS2_PLACEMENT_3D ( 'NONE', #34554, #41939, #12081 ) ;
#20743 = CIRCLE ( 'NONE', #48096, 16.00000000000000000 ) ;
#20744 = ORIENTED_EDGE ( 'NONE', *, *, #20823, .T. ) ;
#20745 = ORIENTED_EDGE ( 'NONE', *, *, #24369, .T. ) ;
#20746 = FACE_OUTER_BOUND ( 'NONE', #2366, .T. ) ;
#20747 = ORIENTED_EDGE ( 'NONE', *, *, #34810, .T. ) ;
#20748 = LINE ( 'NONE', #27868, #5620 ) ;
#20749 = DIRECTION ( 'NONE',  ( 0.000000000000000000, 0.000000000000000000, -1.000000000000000000 ) ) ;
#20750 = VECTOR ( 'NONE', #1616, 1000.000000000000000 ) ;
#20751 = CARTESIAN_POINT ( 'NONE',  ( 10.00000000000000000, 36.13751322684419165, 21.40280677340384230 ) ) ;
#20752 = DIRECTION ( 'NONE',  ( 1.000000000000000000, 0.000000000000000000, 0.000000000000000000 ) ) ;
#20753 = PLANE ( 'NONE',  #41623 ) ;
#20754 = ORIENTED_EDGE ( 'NONE', *, *, #40112, .T. ) ;
#20755 = VECTOR ( 'NONE', #36910, 1000.000000000000000 ) ;
#20756 = VERTEX_POINT ( 'NONE', #21945 ) ;
#20757 = CARTESIAN_POINT ( 'NONE',  ( 0.000000000000000000, -41.91543099594819921, 2.663952781846001816 ) ) ;
#20758 = CARTESIAN_POINT ( 'NONE',  ( 16.30584220631899228, -140.9432449716519784, -5.500000000000000000 ) ) ;
#20759 = ORIENTED_EDGE ( 'NONE', *, *, #19042, .T. ) ;
#20760 = LINE ( 'NONE', #5352, #20214 ) ;
#20761 = ORIENTED_EDGE ( 'NONE', *, *, #14418, .T. ) ;
#20762 = PLANE ( 'NONE',  #19915 ) ;
#20763 = DIRECTION ( 'NONE',  ( 0.000000000000000000, 0.000000000000000000, 1.000000000000000000 ) ) ;
#20764 = CARTESIAN_POINT ( 'NONE',  ( 10.00000000000000000, 4.992566952385523393, -37.16516213103272293 ) ) ;
#20765 = VECTOR ( 'NONE', #39274, 1000.000000000000000 ) ;
#20766 = CARTESIAN_POINT ( 'NONE',  ( 0.000000000000000000, 81.34940948281337114, 10.30890764327411446 ) ) ;
#20767 =( NAMED_UNIT ( * ) SI_UNIT ( $, .STERADIAN. ) SOLID_ANGLE_UNIT ( ) );
#20768 = DIRECTION ( 'NONE',  ( 0.000000000000000000, -0.5224985647159380298, -0.8526401643540988395 ) ) ;
#20769 = ADVANCED_FACE ( 'NONE', ( #22675 ), #18991, .F. ) ;
#20770 = VERTEX_POINT ( 'NONE', #44469 ) ;
#20771 = CARTESIAN_POINT ( 'NONE',  ( 0.000000000000000000, -44.88180994100329713, -63.18004540533077318 ) ) ;
#20772 = CARTESIAN_POINT ( 'NONE',  ( 10.00000000000000000, 0.000000000000000000, 0.000000000000000000 ) ) ;
#20773 = FACE_OUTER_BOUND ( 'NONE', #38764, .T. ) ;
#20774 = DIRECTION ( 'NONE',  ( 0.000000000000000000, 0.000000000000000000, 1.000000000000000000 ) ) ;
#20775 =( NAMED_UNIT ( * ) SI_UNIT ( $, .STERADIAN. ) SOLID_ANGLE_UNIT ( ) );
#20776 = ORIENTED_EDGE ( 'NONE', *, *, #32121, .F. ) ;
#20777 = ORIENTED_EDGE ( 'NONE', *, *, #45483, .T. ) ;
#20778 = ORIENTED_EDGE ( 'NONE', *, *, #27561, .T. ) ;
#20779 = ADVANCED_FACE ( 'NONE', ( #26109 ), #18269, .F. ) ;
#20780 = VECTOR ( 'NONE', #28373, 1000.000000000000000 ) ;
#20781 = ADVANCED_FACE ( 'NONE', ( #14858 ), #33455, .T. ) ;
#20782 = AXIS2_PLACEMENT_3D ( 'NONE', #32204, #47118, #20695 ) ;
#20783 = DIRECTION ( 'NONE',  ( 0.000000000000000000, 0.000000000000000000, 1.000000000000000000 ) ) ;
#20784 = EDGE_CURVE ( 'NONE', #2670, #11996, #44959, .T. ) ;
#20785 = DIRECTION ( 'NONE',  ( 0.000000000000000000, 0.1564344650402311743, -0.9876883405951377704 ) ) ;
#20786 = VECTOR ( 'NONE', #19178, 1000.000000000000000 ) ;
#20787 = EDGE_LOOP ( 'NONE', ( #40190, #18840, #23973, #40817 ) ) ;
#20788 = ORIENTED_EDGE ( 'NONE', *, *, #29556, .F. ) ;
#20789 = EDGE_CURVE ( 'NONE', #16544, #4123, #30028, .T. ) ;
#20790 = CARTESIAN_POINT ( 'NONE',  ( 11.99999999999999822, 55.38113227695783536, 54.21277698773694453 ) ) ;
#20791 = ORIENTED_EDGE ( 'NONE', *, *, #32925, .T. ) ;
#20792 = EDGE_LOOP ( 'NONE', ( #8729, #27053, #15949, #7435 ) ) ;
#20793 = EDGE_CURVE ( 'NONE', #23206, #21915, #26359, .T. ) ;
#20794 = ORIENTED_EDGE ( 'NONE', *, *, #23798, .F. ) ;
#20795 = AXIS2_PLACEMENT_3D ( 'NONE', #16710, #46579, #12087 ) ;
#20796 = AXIS2_PLACEMENT_3D ( 'NONE', #7085, #2935, #10771 ) ;
#20797 = DIRECTION ( 'NONE',  ( -1.000000000000000000, 0.000000000000000000, 0.000000000000000000 ) ) ;
#20798 = EDGE_LOOP ( 'NONE', ( #17109, #44848, #25593, #44439 ) ) ;
#20799 = DIRECTION ( 'NONE',  ( 0.000000000000000000, 0.2079116908177555123, -0.9781476007338064660 ) ) ;
#20800 = VERTEX_POINT ( 'NONE', #25852 ) ;
#20801 = LINE ( 'NONE', #32069, #30595 ) ;
#20802 = CARTESIAN_POINT ( 'NONE',  ( 0.000000000000000000, 0.000000000000000000, 0.000000000000000000 ) ) ;
#20803 = CARTESIAN_POINT ( 'NONE',  ( 0.000000000000000000, 0.000000000000000000, 0.000000000000000000 ) ) ;
#20804 = AXIS2_PLACEMENT_3D ( 'NONE', #39562, #46168, #45933 ) ;
#20805 = ORIENTED_EDGE ( 'NONE', *, *, #46558, .F. ) ;
#20806 = DIRECTION ( 'NONE',  ( 0.000000000000000000, 0.000000000000000000, 1.000000000000000000 ) ) ;
#20807 = ORIENTED_EDGE ( 'NONE', *, *, #14596, .F. ) ;
#20808 = FACE_OUTER_BOUND ( 'NONE', #38153, .T. ) ;
#20809 = CARTESIAN_POINT ( 'NONE',  ( 12.00000000000000000, 18.84667830672579569, -18.68964196561269375 ) ) ;
#20810 = VECTOR ( 'NONE', #45728, 1000.000000000000000 ) ;
#20811 = DIRECTION ( 'NONE',  ( 0.000000000000000000, -0.9238795325112906243, 0.3826834323650805114 ) ) ;
#20812 = VERTEX_POINT ( 'NONE', #25376 ) ;
#20813 = ORIENTED_EDGE ( 'NONE', *, *, #25032, .T. ) ;
#20814 = DIRECTION ( 'NONE',  ( 0.000000000000000000, 0.3826834323650905589, -0.9238795325112864054 ) ) ;
#20815 = CARTESIAN_POINT ( 'NONE',  ( 10.00000000000000000, 0.8828120875905820508, -37.48860685352290290 ) ) ;
#20816 = ORIENTED_EDGE ( 'NONE', *, *, #23713, .T. ) ;
#20817 = CARTESIAN_POINT ( 'NONE',  ( 50.00005079999999680, 0.000000000000000000, 0.000000000000000000 ) ) ;
#20818 = VECTOR ( 'NONE', #31, 1000.000000000000000 ) ;
#20819 = CARTESIAN_POINT ( 'NONE',  ( 11.99999999999999822, 72.35432306680485226, -20.40083707022909110 ) ) ;
#20820 = CARTESIAN_POINT ( 'NONE',  ( 10.00000000000000000, -46.54456581323847786, 59.03342792756247093 ) ) ;
#20821 = CARTESIAN_POINT ( 'NONE',  ( 11.99999999999999822, -24.73286445877655382, -73.44644590900085745 ) ) ;
#20822 = CARTESIAN_POINT ( 'NONE',  ( 11.99999999999999822, -14.67089635893658794, -73.72996012237454977 ) ) ;
#20823 = EDGE_CURVE ( 'NONE', #31993, #6127, #48142, .T. ) ;
#20824 = AXIS2_PLACEMENT_3D ( 'NONE', #7927, #19193, #822 ) ;
#20825 = FACE_OUTER_BOUND ( 'NONE', #38609, .T. ) ;
#20826 = CARTESIAN_POINT ( 'NONE',  ( -10.00000000000000000, 0.000000000000000000, 0.000000000000000000 ) ) ;
#20827 = EDGE_CURVE ( 'NONE', #23361, #22815, #40337, .T. ) ;
#20828 = AXIS2_PLACEMENT_3D ( 'NONE', #5658, #27454, #8588 ) ;
#20829 = DIRECTION ( 'NONE',  ( -1.000000000000000000, 0.000000000000000000, 0.000000000000000000 ) ) ;
#20830 = CARTESIAN_POINT ( 'NONE',  ( 11.99999999999999822, 75.54627589209970040, -17.28742895386005785 ) ) ;
#20831 = PRESENTATION_STYLE_ASSIGNMENT (( #6142 ) ) ;
#20832 = VECTOR ( 'NONE', #13280, 1000.000000000000000 ) ;
#20833 = DIRECTION ( 'NONE',  ( -1.000000000000000000, 0.000000000000000000, -0.000000000000000000 ) ) ;
#20834 = EDGE_CURVE ( 'NONE', #13485, #3749, #29541, .T. ) ;
#20835 = FACE_OUTER_BOUND ( 'NONE', #18739, .T. ) ;
#20836 = ORIENTED_EDGE ( 'NONE', *, *, #45048, .F. ) ;
#20837 = ORIENTED_EDGE ( 'NONE', *, *, #28624, .F. ) ;
#20838 = VECTOR ( 'NONE', #34720, 1000.000000000000000 ) ;
#20839 = LINE ( 'NONE', #24261, #42509 ) ;
#20840 = PRODUCT_DEFINITION_CONTEXT ( 'detailed design', #9147, 'design' ) ;
#20841 = CARTESIAN_POINT ( 'NONE',  ( -3.000000000000000000, 20.85821328998756385, -10.92862929874494959 ) ) ;
#20842 = EDGE_CURVE ( 'NONE', #31342, #28723, #30632, .T. ) ;
#20843 = DIRECTION ( 'NONE',  ( -0.7273375899149793211, 0.6862798483830554463, 0.000000000000000000 ) ) ;
#20844 = ORIENTED_EDGE ( 'NONE', *, *, #7687, .T. ) ;
#20845 = EDGE_CURVE ( 'NONE', #42290, #41629, #43900, .T. ) ;
#20846 = EDGE_CURVE ( 'NONE', #551, #20465, #14374, .T. ) ;
#20847 = ORIENTED_EDGE ( 'NONE', *, *, #34926, .F. ) ;
#20848 = AXIS2_PLACEMENT_3D ( 'NONE', #24603, #16778, #39779 ) ;
#20849 = DIRECTION ( 'NONE',  ( 0.000000000000000000, 0.000000000000000000, 1.000000000000000000 ) ) ;
#20850 = VERTEX_POINT ( 'NONE', #22196 ) ;
#20851 = PLANE ( 'NONE',  #6556 ) ;
#20852 = AXIS2_PLACEMENT_3D ( 'NONE', #28873, #10273, #25194 ) ;
#20853 = VERTEX_POINT ( 'NONE', #44236 ) ;
#20854 = CARTESIAN_POINT ( 'NONE',  ( -3.000000000000000000, 16.61724383029361718, 20.69703378468926402 ) ) ;
#20855 = ORIENTED_EDGE ( 'NONE', *, *, #5867, .F. ) ;
#20856 = PRODUCT_RELATED_PRODUCT_CATEGORY ( 'part', '', ( #13210 ) ) ;
#20857 = DIRECTION ( 'NONE',  ( -1.000000000000000000, -0.000000000000000000, -0.000000000000000000 ) ) ;
#20858 = CIRCLE ( 'NONE', #25525, 15.99999999999999822 ) ;
#20859 = DIRECTION ( 'NONE',  ( 0.8225049752423776450, 0.5687579148473765889, -0.000000000000000000 ) ) ;
#20861 = EDGE_LOOP ( 'NONE', ( #38186, #44253, #10391, #22059 ) ) ;
#20860 = FACE_OUTER_BOUND ( 'NONE', #38038, .T. ) ;
#20862 = ORIENTED_EDGE ( 'NONE', *, *, #18856, .T. ) ;
#20863 = ORIENTED_EDGE ( 'NONE', *, *, #15688, .T. ) ;
#20864 = CIRCLE ( 'NONE', #32569, 31.99999999999998934 ) ;
#20865 = CARTESIAN_POINT ( 'NONE',  ( 11.99999999999999822, 0.000000000000000000, 0.000000000000000000 ) ) ;
#20866 = FACE_OUTER_BOUND ( 'NONE', #12025, .T. ) ;
#20867 = DIRECTION ( 'NONE',  ( 1.000000000000000000, 0.000000000000000000, 0.000000000000000000 ) ) ;
#20868 = CIRCLE ( 'NONE', #42754, 82.00000000000000000 ) ;
#20870 = VERTEX_POINT ( 'NONE', #10710 ) ;
#20869 = FACE_OUTER_BOUND ( 'NONE', #40634, .T. ) ;
#20871 = DIRECTION ( 'NONE',  ( 0.000000000000000000, 0.000000000000000000, 1.000000000000000000 ) ) ;
#20872 = ORIENTED_EDGE ( 'NONE', *, *, #28703, .F. ) ;
#20873 = DIRECTION ( 'NONE',  ( 0.000000000000000000, -0.2079116908177651990, -0.9781476007338044676 ) ) ;
#20874 = ORIENTED_EDGE ( 'NONE', *, *, #15479, .T. ) ;
#20875 = ORIENTED_EDGE ( 'NONE', *, *, #30974, .F. ) ;
#20876 = CYLINDRICAL_SURFACE ( 'NONE', #6706, 31.99999999999999289 ) ;
#20877 = ORIENTED_EDGE ( 'NONE', *, *, #45778, .T. ) ;
#20878 = CARTESIAN_POINT ( 'NONE',  ( 11.99999999999999822, -70.52718814184240159, -26.02418014898383802 ) ) ;
#20879 = CARTESIAN_POINT ( 'NONE',  ( 0.000000000000000000, 0.000000000000000000, 0.000000000000000000 ) ) ;
#20880 = DIRECTION ( 'NONE',  ( -1.000000000000000000, 0.000000000000000000, 0.000000000000000000 ) ) ;
#20881 = EDGE_LOOP ( 'NONE', ( #41516, #3143, #36730, #1280 ) ) ;
#20882 = LINE ( 'NONE', #17186, #26115 ) ;
#20883 = CARTESIAN_POINT ( 'NONE',  ( 11.99999999999999822, 0.000000000000000000, 0.000000000000000000 ) ) ;
#20884 = PLANE ( 'NONE',  #18053 ) ;
#20885 = FACE_OUTER_BOUND ( 'NONE', #19088, .T. ) ;
#20886 = DIRECTION ( 'NONE',  ( 1.000000000000000000, 0.000000000000000000, 0.000000000000000000 ) ) ;
#20887 = VECTOR ( 'NONE', #18916, 1000.000000000000000 ) ;
#20888 = EDGE_LOOP ( 'NONE', ( #24814, #44746, #34475, #7420 ) ) ;
#20889 = EDGE_CURVE ( 'NONE', #29937, #29716, #25616, .T. ) ;
#20890 = CARTESIAN_POINT ( 'NONE',  ( 11.99999999999999822, -68.26794271651286294, 31.47745569255117104 ) ) ;
#20891 = CARTESIAN_POINT ( 'NONE',  ( 0.000000000000000000, 0.000000000000000000, 53.20000000000001705 ) ) ;
#20892 = CARTESIAN_POINT ( 'NONE',  ( -11.70000000000000107, 2.137572712735109784E-15, -17.45460580326810174 ) ) ;
#20893 = FACE_OUTER_BOUND ( 'NONE', #47147, .T. ) ;
#20894 = EDGE_CURVE ( 'NONE', #29688, #18977, #115, .T. ) ;
#20895 = AXIS2_PLACEMENT_3D ( 'NONE', #37192, #36931, #22267 ) ;
#20896 = DIRECTION ( 'NONE',  ( 0.000000000000000000, 0.000000000000000000, 1.000000000000000000 ) ) ;
#20897 = CARTESIAN_POINT ( 'NONE',  ( 0.000000000000000000, -36.13751322684434797, 21.40280677340357940 ) ) ;
#20898 = EDGE_CURVE ( 'NONE', #34042, #11749, #11669, .T. ) ;
#20899 = ORIENTED_EDGE ( 'NONE', *, *, #45460, .F. ) ;
#20900 = CARTESIAN_POINT ( 'NONE',  ( 10.00000000000000000, 0.000000000000000000, 0.000000000000000000 ) ) ;
#20901 = VECTOR ( 'NONE', #39743, 1000.000000000000000 ) ;
#20902 = VERTEX_POINT ( 'NONE', #8232 ) ;
#20903 = CARTESIAN_POINT ( 'NONE',  ( 0.000000000000000000, -6.903761155838323837, 77.19088730480521576 ) ) ;
#20904 = DIRECTION ( 'NONE',  ( -1.000000000000000000, 0.000000000000000000, -0.000000000000000000 ) ) ;
#20905 = VERTEX_POINT ( 'NONE', #4336 ) ;
#20906 = EDGE_CURVE ( 'NONE', #12269, #41614, #40795, .T. ) ;
#20907 = ADVANCED_FACE ( 'NONE', ( #19247 ), #31009, .T. ) ;
#20908 = AXIS2_PLACEMENT_3D ( 'NONE', #14080, #43939, #48097 ) ;
#20909 = CYLINDRICAL_SURFACE ( 'NONE', #40251, 16.00000000000000000 ) ;
#20910 = ORIENTED_EDGE ( 'NONE', *, *, #22697, .F. ) ;
#20911 = ORIENTED_EDGE ( 'NONE', *, *, #31569, .F. ) ;
#20912 = ADVANCED_FACE ( 'NONE', ( #42242 ), #34173, .T. ) ;
#20913 = VECTOR ( 'NONE', #17416, 1000.000000000000000 ) ;
#20914 = DIRECTION ( 'NONE',  ( -0.000000000000000000, 0.1045284632676548031, 0.9945218953682732899 ) ) ;
#20915 = VERTEX_POINT ( 'NONE', #646 ) ;
#20916 = CARTESIAN_POINT ( 'NONE',  ( 15.00000000000000000, -10.45096189432344502, -21.10159698893425784 ) ) ;
#20917 = CARTESIAN_POINT ( 'NONE',  ( 10.00000000000000000, 20.40083707022882820, 72.35432306680490910 ) ) ;
#20918 = VERTEX_POINT ( 'NONE', #15575 ) ;
#20919 = AXIS2_PLACEMENT_3D ( 'NONE', #3849, #18758, #43997 ) ;
#20920 = DIRECTION ( 'NONE',  ( -1.000000000000000000, -0.000000000000000000, -0.000000000000000000 ) ) ;
#20921 = ORIENTED_EDGE ( 'NONE', *, *, #35464, .F. ) ;
#20922 = ORIENTED_EDGE ( 'NONE', *, *, #2913, .T. ) ;
#20923 = ORIENTED_EDGE ( 'NONE', *, *, #3127, .F. ) ;
#20924 = CARTESIAN_POINT ( 'NONE',  ( 10.00000000000000000, 0.000000000000000000, 0.000000000000000000 ) ) ;
#20925 = CARTESIAN_POINT ( 'NONE',  ( 0.000000000000000000, -89.50000000000000000, 2.500000000000000000 ) ) ;
#20926 = DIRECTION ( 'NONE',  ( -1.000000000000000000, -0.000000000000000000, 0.000000000000000000 ) ) ;
#20927 = VERTEX_POINT ( 'NONE', #38333 ) ;
#20928 = VECTOR ( 'NONE', #4925, 1000.000000000000227 ) ;
#20929 = ORIENTED_EDGE ( 'NONE', *, *, #12131, .F. ) ;
#20930 = CARTESIAN_POINT ( 'NONE',  ( 0.000000000000000000, 0.000000000000000000, 0.000000000000000000 ) ) ;
#20931 = VERTEX_POINT ( 'NONE', #45929 ) ;
#20932 = CARTESIAN_POINT ( 'NONE',  ( 0.000000000000000000, 0.000000000000000000, -43.79999999999998295 ) ) ;
#20933 = CARTESIAN_POINT ( 'NONE',  ( 6.377742925735834234, -145.7647898336707897, -2.500000000000000000 ) ) ;
#20934 = DIRECTION ( 'NONE',  ( -1.000000000000000000, -0.000000000000000000, 0.000000000000000000 ) ) ;
#20935 = LINE ( 'NONE', #39287, #18865 ) ;
#20936 = DIRECTION ( 'NONE',  ( -1.000000000000000000, -0.000000000000000000, 0.000000000000000000 ) ) ;
#20937 = DIRECTION ( 'NONE',  ( 1.000000000000000000, 0.000000000000000000, 0.000000000000000000 ) ) ;
#20938 = CARTESIAN_POINT ( 'NONE',  ( 0.000000000000000000, 22.48208911017500355, 35.47612816024530957 ) ) ;
#20939 = CARTESIAN_POINT ( 'NONE',  ( 11.99999999999999822, -75.54627589209931671, -17.28742895386162814 ) ) ;
#20940 = AXIS2_PLACEMENT_3D ( 'NONE', #2226, #9810, #10050 ) ;
#20941 = CARTESIAN_POINT ( 'NONE',  ( -11.70000000000000107, 0.000000000000000000, 17.45460580326810174 ) ) ;
#20942 = DIRECTION ( 'NONE',  ( -1.000000000000000000, -0.000000000000000000, 0.000000000000000000 ) ) ;
#20943 = VERTEX_POINT ( 'NONE', #30506 ) ;
#20944 = EDGE_CURVE ( 'NONE', #45638, #488, #19468, .T. ) ;
#20945 = LINE ( 'NONE', #10658, #17353 ) ;
#20946 = LINE ( 'NONE', #28771, #20586 ) ;
#20947 = EDGE_CURVE ( 'NONE', #15373, #29567, #12396, .T. ) ;
#20948 = LINE ( 'NONE', #31255, #7588 ) ;
#20949 = CIRCLE ( 'NONE', #6108, 35.50000000000000711 ) ;
#20950 = DIRECTION ( 'NONE',  ( -1.000000000000000000, 0.000000000000000000, 0.000000000000000000 ) ) ;
#20951 = DIRECTION ( 'NONE',  ( -1.000000000000000000, 0.000000000000000000, 0.000000000000000000 ) ) ;
#20953 = EDGE_CURVE ( 'NONE', #16941, #14753, #37644, .T. ) ;
#20952 = ORIENTED_EDGE ( 'NONE', *, *, #8275, .F. ) ;
#20954 = DIRECTION ( 'NONE',  ( -1.000000000000000000, -0.000000000000000000, -0.000000000000000000 ) ) ;
#20955 = VERTEX_POINT ( 'NONE', #45429 ) ;
#20956 = CIRCLE ( 'NONE', #30362, 82.00000000000000000 ) ;
#20957 = CARTESIAN_POINT ( 'NONE',  ( 11.99999999999999822, -41.19522573413689059, -65.64334221924951862 ) ) ;
#20958 = ORIENTED_EDGE ( 'NONE', *, *, #19805, .F. ) ;
#20959 = EDGE_LOOP ( 'NONE', ( #32412, #11548, #39599, #17020 ) ) ;
#20960 = EDGE_CURVE ( 'NONE', #31411, #36422, #32212, .T. ) ;
#20961 = ADVANCED_FACE ( 'NONE', ( #45200 ), #20208, .F. ) ;
#20962 = ORIENTED_EDGE ( 'NONE', *, *, #43492, .T. ) ;
#20963 = LINE ( 'NONE', #40527, #34312 ) ;
#20964 = ORIENTED_EDGE ( 'NONE', *, *, #21197, .T. ) ;
#20965 = VECTOR ( 'NONE', #30108, 1000.000000000000000 ) ;
#20966 = ORIENTED_EDGE ( 'NONE', *, *, #17344, .F. ) ;
#20967 = EDGE_CURVE ( 'NONE', #46842, #10502, #40035, .T. ) ;
#20968 = DIRECTION ( 'NONE',  ( 0.000000000000000000, 0.000000000000000000, -1.000000000000000000 ) ) ;
#20969 = CYLINDRICAL_SURFACE ( 'NONE', #8158, 31.99999999999999289 ) ;
#20970 = ORIENTED_EDGE ( 'NONE', *, *, #4927, .T. ) ;
#20971 = ORIENTED_EDGE ( 'NONE', *, *, #29735, .F. ) ;
#20972 = DIRECTION ( 'NONE',  ( 0.000000000000000000, 0.8526401643540935105, -0.5224985647159468005 ) ) ;
#20973 = LINE ( 'NONE', #42779, #3172 ) ;
#20974 = EDGE_CURVE ( 'NONE', #14404, #24169, #31448, .T. ) ;
#20975 = CARTESIAN_POINT ( 'NONE',  ( 0.000000000000000000, 30.00120703465236716, -22.64427369931138756 ) ) ;
#20976 = ORIENTED_EDGE ( 'NONE', *, *, #44541, .T. ) ;
#20977 = ORIENTED_EDGE ( 'NONE', *, *, #42134, .F. ) ;
#20978 = DIRECTION ( 'NONE',  ( 0.3090169943749573878, -0.9510565162951503115, 0.000000000000000000 ) ) ;
#20979 = ORIENTED_EDGE ( 'NONE', *, *, #31239, .F. ) ;
#20980 = DIRECTION ( 'NONE',  ( 0.000000000000000000, 0.9510565162951543083, -0.3090169943749448977 ) ) ;
#20981 = DIRECTION ( 'NONE',  ( 1.000000000000000000, 0.000000000000000000, -0.000000000000000000 ) ) ;
#20982 = CIRCLE ( 'NONE', #27241, 77.49899999999999523 ) ;
#20984 = DIRECTION ( 'NONE',  ( -1.000000000000000000, 0.000000000000000000, 0.000000000000000000 ) ) ;
#20983 = AXIS2_PLACEMENT_3D ( 'NONE', #3597, #22199, #24903 ) ;
#20985 = DIRECTION ( 'NONE',  ( 0.000000000000000000, 0.5877852522924741363, -0.8090169943749465631 ) ) ;
#20986 = LINE ( 'NONE', #17790, #29924 ) ;
#20987 = CARTESIAN_POINT ( 'NONE',  ( 0.000000000000000000, 55.19960302592066625, 51.03279382321107249 ) ) ;
#20988 = CYLINDRICAL_SURFACE ( 'NONE', #36869, 31.99999999999998579 ) ;
#20989 = ORIENTED_EDGE ( 'NONE', *, *, #46447, .F. ) ;
#20990 = ADVANCED_FACE ( 'NONE', ( #38583 ), #5048, .T. ) ;
#20991 = LINE ( 'NONE', #5842, #12404 ) ;
#20992 = VERTEX_POINT ( 'NONE', #27325 ) ;
#20993 = DIRECTION ( 'NONE',  ( 0.000000000000000000, 0.000000000000000000, 1.000000000000000000 ) ) ;
#20994 = ADVANCED_FACE ( 'NONE', ( #34897 ), #12165, .T. ) ;
#20995 = DIRECTION ( 'NONE',  ( -1.000000000000000000, 0.000000000000000000, 0.000000000000000000 ) ) ;
#20996 = DIRECTION ( 'NONE',  ( 0.000000000000000000, 0.000000000000000000, 1.000000000000000000 ) ) ;
#20997 = AXIS2_PLACEMENT_3D ( 'NONE', #13328, #14285, #47801 ) ;
#20998 = DIRECTION ( 'NONE',  ( -1.000000000000000000, -0.000000000000000000, -0.000000000000000000 ) ) ;
#20999 = EDGE_CURVE ( 'NONE', #39605, #28052, #29853, .T. ) ;
#21000 = CARTESIAN_POINT ( 'NONE',  ( -25.50183398199384754, -112.6408924756582053, 5.500000000000000000 ) ) ;
#21001 = DIRECTION ( 'NONE',  ( -1.000000000000000000, -0.000000000000000000, -0.000000000000000000 ) ) ;
#21002 = ORIENTED_EDGE ( 'NONE', *, *, #22914, .F. ) ;
#21003 = DIRECTION ( 'NONE',  ( -0.000000000000000000, -0.000000000000000000, -1.000000000000000000 ) ) ;
#21004 = DIRECTION ( 'NONE',  ( 0.000000000000000000, 0.9510565162951546414, -0.3090169943749446202 ) ) ;
#21005 = CARTESIAN_POINT ( 'NONE',  ( 11.99999999999999822, -12.93880638057260946, -76.41127070299286572 ) ) ;
#21006 = EDGE_CURVE ( 'NONE', #35973, #36243, #947, .T. ) ;
#21007 = CARTESIAN_POINT ( 'NONE',  ( 0.000000000000000000, 23.16143007188426850, 73.95703589263983702 ) ) ;
#21008 = ORIENTED_EDGE ( 'NONE', *, *, #31417, .F. ) ;
#21009 = ORIENTED_EDGE ( 'NONE', *, *, #3886, .T. ) ;
#21010 = VECTOR ( 'NONE', #17645, 1000.000000000000000 ) ;
#21011 = AXIS2_PLACEMENT_3D ( 'NONE', #9043, #35216, #9508 ) ;
#21012 = FACE_OUTER_BOUND ( 'NONE', #20252, .T. ) ;
#21013 = CARTESIAN_POINT ( 'NONE',  ( -23.30023580412278505, -123.4057321492263384, -5.500000000000000000 ) ) ;
#21014 = AXIS2_PLACEMENT_3D ( 'NONE', #11476, #11220, #22481 ) ;
#21015 = ORIENTED_EDGE ( 'NONE', *, *, #32944, .F. ) ;
#21016 = EDGE_CURVE ( 'NONE', #1488, #2398, #46286, .T. ) ;
#21017 = DIRECTION ( 'NONE',  ( -1.000000000000000000, 0.000000000000000000, 0.000000000000000000 ) ) ;
#21018 = VERTEX_POINT ( 'NONE', #17246 ) ;
#21019 = VECTOR ( 'NONE', #36162, 1000.000000000000000 ) ;
#21020 = VERTEX_POINT ( 'NONE', #16791 ) ;
#21021 = VERTEX_POINT ( 'NONE', #28274 ) ;
#21022 = ORIENTED_EDGE ( 'NONE', *, *, #18055, .F. ) ;
#21023 =( GEOMETRIC_REPRESENTATION_CONTEXT ( 3 ) GLOBAL_UNCERTAINTY_ASSIGNED_CONTEXT ( ( #15898 ) ) GLOBAL_UNIT_ASSIGNED_CONTEXT ( ( #23466, #38408, #15179 ) ) REPRESENTATION_CONTEXT ( 'NONE', 'WORKASPACE' ) );
#21024 = DIRECTION ( 'NONE',  ( 1.000000000000000000, 0.000000000000000000, 0.000000000000000000 ) ) ;
#21025 = ORIENTED_EDGE ( 'NONE', *, *, #31417, .T. ) ;
#21026 = VERTEX_POINT ( 'NONE', #9921 ) ;
#21027 = DIRECTION ( 'NONE',  ( 0.000000000000000000, 0.000000000000000000, 1.000000000000000000 ) ) ;
#21028 = ORIENTED_EDGE ( 'NONE', *, *, #36083, .T. ) ;
#21029 = CARTESIAN_POINT ( 'NONE',  ( 10.00000000000000000, -26.08949754953044220, 27.05870788708222818 ) ) ;
#21030 = CYLINDRICAL_SURFACE ( 'NONE', #6677, 77.49899999999999523 ) ;
#21031 = CARTESIAN_POINT ( 'NONE',  ( 10.00000000000000000, -4.992566952384716927, -37.16516213103282951 ) ) ;
#21032 = ORIENTED_EDGE ( 'NONE', *, *, #3501, .T. ) ;
#21033 = CARTESIAN_POINT ( 'NONE',  ( 11.99999999999999822, 0.000000000000000000, 0.000000000000000000 ) ) ;
#21034 = VERTEX_POINT ( 'NONE', #43465 ) ;
#21035 = CARTESIAN_POINT ( 'NONE',  ( -20.30386590532152979, -102.9045904027214959, -5.500000000000000000 ) ) ;
#21036 = CIRCLE ( 'NONE', #46072, 16.00000000000000000 ) ;
#21037 = CARTESIAN_POINT ( 'NONE',  ( 0.000000000000000000, 65.58780272294129077, -36.73666225445822420 ) ) ;
#21038 = ORIENTED_EDGE ( 'NONE', *, *, #28624, .T. ) ;
#21039 = VECTOR ( 'NONE', #10971, 1000.000000000000000 ) ;
#21040 = ORIENTED_EDGE ( 'NONE', *, *, #13088, .F. ) ;
#21041 = EDGE_CURVE ( 'NONE', #37092, #17765, #43209, .T. ) ;
#21042 = DIRECTION ( 'NONE',  ( -1.000000000000000000, 0.000000000000000000, -0.000000000000000000 ) ) ;
#21043 = DIRECTION ( 'NONE',  ( -1.000000000000000000, 0.000000000000000000, 0.000000000000000000 ) ) ;
#21044 = VERTEX_POINT ( 'NONE', #13590 ) ;
#21045 = CARTESIAN_POINT ( 'NONE',  ( -11.99999999999999645, 1.574895783703496238E-15, -12.85999999999999943 ) ) ;
#21046 = DIRECTION ( 'NONE',  ( 0.000000000000000000, 0.000000000000000000, 1.000000000000000000 ) ) ;
#21047 = CYLINDRICAL_SURFACE ( 'NONE', #1850, 31.99999999999997868 ) ;
#21048 = EDGE_CURVE ( 'NONE', #33987, #25896, #43689, .T. ) ;
#21049 = CARTESIAN_POINT ( 'NONE',  ( 11.99999999999999822, 6.903761155837791819, 77.19088730480525840 ) ) ;
#21050 = DIRECTION ( 'NONE',  ( -1.000000000000000000, -0.000000000000000000, -0.000000000000000000 ) ) ;
#21051 = CARTESIAN_POINT ( 'NONE',  ( 0.000000000000000000, 59.03342792756263435, 46.54456581323825048 ) ) ;
#21052 = CIRCLE ( 'NONE', #7005, 31.99999999999998579 ) ;
#21053 = DIRECTION ( 'NONE',  ( -1.000000000000000000, -0.000000000000000000, 0.000000000000000000 ) ) ;
#21054 = EDGE_CURVE ( 'NONE', #17275, #7609, #46406, .T. ) ;
#21056 = EDGE_CURVE ( 'NONE', #34673, #17574, #39257, .T. ) ;
#21055 = ADVANCED_BREP_SHAPE_REPRESENTATION ( '', ( #2931, #11636 ), #21829 ) ;
#21057 = LINE ( 'NONE', #28657, #25250 ) ;
#21058 = DIRECTION ( 'NONE',  ( -1.000000000000000000, -0.000000000000000000, -0.000000000000000000 ) ) ;
#21059 = FACE_OUTER_BOUND ( 'NONE', #39791, .T. ) ;
#21060 = CARTESIAN_POINT ( 'NONE',  ( -21.33958957442910886, -129.9559990355020034, -2.500000000000000000 ) ) ;
#21061 = VERTEX_POINT ( 'NONE', #28529 ) ;
#21062 = ORIENTED_EDGE ( 'NONE', *, *, #5306, .T. ) ;
#21063 = DIRECTION ( 'NONE',  ( -0.000000000000000000, -0.000000000000000000, 1.000000000000000000 ) ) ;
#21064 = ADVANCED_FACE ( 'NONE', ( #24614 ), #21166, .F. ) ;
#21065 = CARTESIAN_POINT ( 'NONE',  ( 11.99999999999999822, 51.03279382321166224, -55.19960302592011914 ) ) ;
#21066 = EDGE_LOOP ( 'NONE', ( #15328, #40422, #8255, #34806 ) ) ;
#21067 = AXIS2_PLACEMENT_3D ( 'NONE', #13471, #2216, #42369 ) ;
#21068 = VECTOR ( 'NONE', #36379, 1000.000000000000000 ) ;
#21069 = CARTESIAN_POINT ( 'NONE',  ( 15.00000000000000000, -19.89357724625003598, -12.59942793731059041 ) ) ;
#21070 = ORIENTED_EDGE ( 'NONE', *, *, #20055, .T. ) ;
#21071 = DIRECTION ( 'NONE',  ( 0.000000000000000000, 0.5877852522924797984, -0.8090169943749426773 ) ) ;
#21072 = AXIS2_PLACEMENT_3D ( 'NONE', #44201, #28554, #10675 ) ;
#21073 = VERTEX_POINT ( 'NONE', #24358 ) ;
#21074 = FACE_OUTER_BOUND ( 'NONE', #44135, .T. ) ;
#21075 = ORIENTED_EDGE ( 'NONE', *, *, #11250, .F. ) ;
#21076 = DIRECTION ( 'NONE',  ( 0.000000000000000000, 0.000000000000000000, 1.000000000000000000 ) ) ;
#21077 = AXIS2_PLACEMENT_3D ( 'NONE', #44820, #36981, #43850 ) ;
#21078 = DIRECTION ( 'NONE',  ( 0.000000000000000000, -0.07845909572783056618, -0.9969173337331290741 ) ) ;
#21079 = CARTESIAN_POINT ( 'NONE',  ( 10.00000000000000000, -40.68715046381937128, 10.41901085202062660 ) ) ;
#21080 = EDGE_CURVE ( 'NONE', #41947, #37711, #35859, .T. ) ;
#21081 = VERTEX_POINT ( 'NONE', #2559 ) ;
#21082 = VERTEX_POINT ( 'NONE', #31740 ) ;
#21083 = LINE ( 'NONE', #17408, #42365 ) ;
#21084 = EDGE_CURVE ( 'NONE', #13194, #28502, #47375, .T. ) ;
#21085 = PLANE ( 'NONE',  #31626 ) ;
#21086 = CYLINDRICAL_SURFACE ( 'NONE', #23948, 11.59999999999999787 ) ;
#21087 = CYLINDRICAL_SURFACE ( 'NONE', #39089, 11.59999999999999787 ) ;
#21088 = CYLINDRICAL_SURFACE ( 'NONE', #4338, 82.00000000000000000 ) ;
#21089 = EDGE_LOOP ( 'NONE', ( #8020, #30785, #20744, #37558 ) ) ;
#21090 = LINE ( 'NONE', #42417, #6079 ) ;
#21091 = VERTEX_POINT ( 'NONE', #1862 ) ;
#21092 = FACE_OUTER_BOUND ( 'NONE', #47814, .T. ) ;
#21093 = ORIENTED_EDGE ( 'NONE', *, *, #27420, .F. ) ;
#21094 = DIRECTION ( 'NONE',  ( -1.000000000000000000, -0.000000000000000000, 0.000000000000000000 ) ) ;
#21095 = DIRECTION ( 'NONE',  ( -1.000000000000000000, 0.000000000000000000, -0.000000000000000000 ) ) ;
#21096 = CARTESIAN_POINT ( 'NONE',  ( 0.000000000000000000, 0.000000000000000000, 0.000000000000000000 ) ) ;
#21097 = VERTEX_POINT ( 'NONE', #42977 ) ;
#21098 = CARTESIAN_POINT ( 'NONE',  ( 15.00000000000000000, -25.60904388321916159, 6.976881207771517879 ) ) ;
#21099 = EDGE_CURVE ( 'NONE', #12494, #26652, #39294, .T. ) ;
#21100 = FACE_OUTER_BOUND ( 'NONE', #23955, .T. ) ;
#21101 = EDGE_CURVE ( 'NONE', #41161, #33614, #1615, .T. ) ;
#21102 = EDGE_CURVE ( 'NONE', #14954, #20060, #46655, .T. ) ;
#21103 = CARTESIAN_POINT ( 'NONE',  ( 0.000000000000000000, 0.000000000000000000, -56.19999999999998863 ) ) ;
#21105 = AXIS2_PLACEMENT_3D ( 'NONE', #9404, #35607, #16996 ) ;
#21104 = DIRECTION ( 'NONE',  ( 0.000000000000000000, 0.000000000000000000, 1.000000000000000000 ) ) ;
#21106 = AXIS2_PLACEMENT_3D ( 'NONE', #8923, #23860, #42949 ) ;
#21107 = CARTESIAN_POINT ( 'NONE',  ( 10.00000000000000000, 20.40083707022987625, -72.35432306680462489 ) ) ;
#21108 = LINE ( 'NONE', #17691, #45777 ) ;
#21109 = CARTESIAN_POINT ( 'NONE',  ( 21.07894319797337701, -103.8699611390234878, 5.500000000000000000 ) ) ;
#21110 = CARTESIAN_POINT ( 'NONE',  ( 15.00000000000000000, 18.84667830672579569, -18.68964196561269375 ) ) ;
#21111 = CIRCLE ( 'NONE', #10863, 42.00000000000000000 ) ;
#21112 = EDGE_LOOP ( 'NONE', ( #3929, #39093, #39602, #12399, #15835, #10432 ) ) ;
#21113 = ORIENTED_EDGE ( 'NONE', *, *, #28353, .F. ) ;
#21114 = EDGE_CURVE ( 'NONE', #18029, #40235, #15814, .T. ) ;
#21115 = CARTESIAN_POINT ( 'NONE',  ( 10.00000000000000000, 0.000000000000000000, 0.000000000000000000 ) ) ;
#21116 = DIRECTION ( 'NONE',  ( -1.000000000000000000, 0.000000000000000000, 0.000000000000000000 ) ) ;
#21117 = CIRCLE ( 'NONE', #25031, 32.00000000000000000 ) ;
#21118 = AXIS2_PLACEMENT_3D ( 'NONE', #33150, #36337, #6248 ) ;
#21119 = ORIENTED_EDGE ( 'NONE', *, *, #38753, .T. ) ;
#21120 = CYLINDRICAL_SURFACE ( 'NONE', #46495, 31.99999999999999289 ) ;
#21121 = VECTOR ( 'NONE', #9299, 1000.000000000000000 ) ;
#21122 = ORIENTED_EDGE ( 'NONE', *, *, #43282, .F. ) ;
#21123 = DIRECTION ( 'NONE',  ( -1.000000000000000000, 0.000000000000000000, 0.000000000000000000 ) ) ;
#21124 = EDGE_CURVE ( 'NONE', #24556, #17554, #35629, .T. ) ;
#21125 = CARTESIAN_POINT ( 'NONE',  ( 10.00000000000000000, 81.96053171279901051, -2.543863470248666658 ) ) ;
#21126 = ORIENTED_EDGE ( 'NONE', *, *, #33546, .F. ) ;
#21127 = CARTESIAN_POINT ( 'NONE',  ( 11.99999999999999822, 0.000000000000000000, 0.000000000000000000 ) ) ;
#21128 = ORIENTED_EDGE ( 'NONE', *, *, #24768, .T. ) ;
#21129 = ORIENTED_EDGE ( 'NONE', *, *, #11621, .T. ) ;
#21130 = EDGE_CURVE ( 'NONE', #37827, #15854, #38458, .T. ) ;
#21131 = EDGE_CURVE ( 'NONE', #36385, #18965, #2327, .T. ) ;
#21132 = DIRECTION ( 'NONE',  ( 0.000000000000000000, 0.000000000000000000, -1.000000000000000000 ) ) ;
#21133 = VERTEX_POINT ( 'NONE', #39557 ) ;
#21134 = AXIS2_PLACEMENT_3D ( 'NONE', #27004, #35051, #12548 ) ;
#21135 = LINE ( 'NONE', #40250, #3923 ) ;
#21136 = FACE_OUTER_BOUND ( 'NONE', #11956, .T. ) ;
#21137 = AXIS2_PLACEMENT_3D ( 'NONE', #13058, #20626, #16960 ) ;
#21138 = CIRCLE ( 'NONE', #37538, 16.00000000000000000 ) ;
#21139 = EDGE_CURVE ( 'NONE', #13671, #38915, #6023, .T. ) ;
#21140 = EDGE_LOOP ( 'NONE', ( #29756, #16766, #37454, #7247 ) ) ;
#21141 = FACE_OUTER_BOUND ( 'NONE', #13258, .T. ) ;
#21142 = ORIENTED_EDGE ( 'NONE', *, *, #32101, .F. ) ;
#21143 = EDGE_CURVE ( 'NONE', #4357, #37720, #18695, .T. ) ;
#21144 = ORIENTED_EDGE ( 'NONE', *, *, #34467, .F. ) ;
#21145 = PRESENTATION_LAYER_ASSIGNMENT (  '', '', ( #7879 ) ) ;
#21146 = FACE_OUTER_BOUND ( 'NONE', #28313, .T. ) ;
#21147 = DIRECTION ( 'NONE',  ( -0.9997280174009349762, 0.02332147558787671729, 0.000000000000000000 ) ) ;
#21148 = AXIS2_PLACEMENT_3D ( 'NONE', #13524, #43398, #41409 ) ;
#21149 = DIRECTION ( 'NONE',  ( 0.000000000000000000, 0.000000000000000000, 1.000000000000000000 ) ) ;
#21150 = VERTEX_POINT ( 'NONE', #14568 ) ;
#21151 = VECTOR ( 'NONE', #32961, 1000.000000000000000 ) ;
#21152 = CARTESIAN_POINT ( 'NONE',  ( 10.00000000000000000, 0.000000000000000000, 0.000000000000000000 ) ) ;
#21153 = EDGE_LOOP ( 'NONE', ( #18470, #23859, #21998, #21590 ) ) ;
#21154 = ORIENTED_EDGE ( 'NONE', *, *, #33210, .T. ) ;
#21155 = EDGE_CURVE ( 'NONE', #29636, #8637, #29961, .T. ) ;
#21156 = DIRECTION ( 'NONE',  ( 1.000000000000000000, -0.000000000000000000, -0.000000000000000000 ) ) ;
#21157 = DIRECTION ( 'NONE',  ( -0.000000000000000000, -0.5877852522924789103, 0.8090169943749432324 ) ) ;
#21158 = LINE ( 'NONE', #44407, #31316 ) ;
#21159 = CARTESIAN_POINT ( 'NONE',  ( 10.00000000000000000, -2.946379043145784582, -75.11764819372150725 ) ) ;
#21160 = DIRECTION ( 'NONE',  ( 0.000000000000000000, 0.7431448254773863615, -0.6691306063588670083 ) ) ;
#21161 = DIRECTION ( 'NONE',  ( -1.000000000000000000, 0.000000000000000000, 0.000000000000000000 ) ) ;
#21162 = EDGE_CURVE ( 'NONE', #8930, #451, #30658, .T. ) ;
#21163 = EDGE_CURVE ( 'NONE', #2768, #894, #9547, .T. ) ;
#21164 = CARTESIAN_POINT ( 'NONE',  ( -6.509281303079589520, -14.89695620656361008, 0.000000000000000000 ) ) ;
#21165 = DIRECTION ( 'NONE',  ( -1.000000000000000000, 0.000000000000000000, 0.000000000000000000 ) ) ;
#21166 = PLANE ( 'NONE',  #45500 ) ;
#21167 = DIRECTION ( 'NONE',  ( -1.000000000000000000, 0.000000000000000000, 0.000000000000000000 ) ) ;
#21168 = EDGE_LOOP ( 'NONE', ( #6161, #30780, #10414, #41573 ) ) ;
#21169 = DIRECTION ( 'NONE',  ( -1.000000000000000000, -0.000000000000000000, 0.000000000000000000 ) ) ;
#21170 = CYLINDRICAL_SURFACE ( 'NONE', #35330, 37.49900000000000233 ) ;
#21171 = CYLINDRICAL_SURFACE ( 'NONE', #40132, 32.00000000000000000 ) ;
#21172 = CARTESIAN_POINT ( 'NONE',  ( 10.00000000000000000, -29.81001611431024756, 22.74946021919122785 ) ) ;
#21173 = ADVANCED_FACE ( 'NONE', ( #11382 ), #29718, .F. ) ;
#21174 = CIRCLE ( 'NONE', #11791, 42.00000000000000000 ) ;
#21175 = LINE ( 'NONE', #10662, #45897 ) ;
#21176 = CARTESIAN_POINT ( 'NONE',  ( 0.000000000000000000, 0.000000000000000000, 0.000000000000000000 ) ) ;
#21177 = AXIS2_PLACEMENT_3D ( 'NONE', #46695, #13631, #20004 ) ;
#21178 = ORIENTED_EDGE ( 'NONE', *, *, #7578, .F. ) ;
#21179 = CARTESIAN_POINT ( 'NONE',  ( 15.00000000000000000, 26.50000000000000355, -1.500000000000000000 ) ) ;
#21180 = VECTOR ( 'NONE', #24230, 1000.000000000000000 ) ;
#21181 = CIRCLE ( 'NONE', #17262, 31.99999999999999289 ) ;
#21182 = CARTESIAN_POINT ( 'NONE',  ( 10.00000000000000000, -14.66109333815410487, -73.73191006444587003 ) ) ;
#21183 = VECTOR ( 'NONE', #10512, 1000.000000000000114 ) ;
#21184 = ORIENTED_EDGE ( 'NONE', *, *, #48330, .T. ) ;
#21185 = ORIENTED_EDGE ( 'NONE', *, *, #21571, .F. ) ;
#21186 = CIRCLE ( 'NONE', #43070, 77.49900000000000944 ) ;
#21187 = AXIS2_PLACEMENT_3D ( 'NONE', #37366, #30025, #23161 ) ;
#21188 = DIRECTION ( 'NONE',  ( 0.000000000000000000, 0.000000000000000000, 1.000000000000000000 ) ) ;
#21189 = ORIENTED_EDGE ( 'NONE', *, *, #10459, .T. ) ;
#21190 = ORIENTED_EDGE ( 'NONE', *, *, #25529, .F. ) ;
#21191 = LINE ( 'NONE', #25826, #15598 ) ;
#21192 = DIRECTION ( 'NONE',  ( -1.000000000000000000, -0.000000000000000000, -0.000000000000000000 ) ) ;
#21193 = ADVANCED_FACE ( 'NONE', ( #17742 ), #32667, .T. ) ;
#21194 = ORIENTED_EDGE ( 'NONE', *, *, #2379, .F. ) ;
#21195 = ORIENTED_EDGE ( 'NONE', *, *, #18495, .T. ) ;
#21196 = ORIENTED_EDGE ( 'NONE', *, *, #40618, .F. ) ;
#21197 = EDGE_CURVE ( 'NONE', #6467, #20013, #25315, .T. ) ;
#21198 = DIRECTION ( 'NONE',  ( -1.000000000000000000, 0.000000000000000000, 0.000000000000000000 ) ) ;
#21200 = VERTEX_POINT ( 'NONE', #3775 ) ;
#21199 = LINE ( 'NONE', #29033, #1628 ) ;
#21201 = VECTOR ( 'NONE', #29660, 1000.000000000000114 ) ;
#21202 = DIRECTION ( 'NONE',  ( 0.9781476007338069101, 2.546183866652752180E-17, 0.2079116908177528755 ) ) ;
#21203 = ORIENTED_EDGE ( 'NONE', *, *, #19165, .T. ) ;
#21204 = EDGE_LOOP ( 'NONE', ( #40323, #41985, #3415, #47567 ) ) ;
#21205 = ORIENTED_EDGE ( 'NONE', *, *, #14704, .F. ) ;
#21206 = DIRECTION ( 'NONE',  ( 0.000000000000000000, 0.000000000000000000, -1.000000000000000000 ) ) ;
#21207 = ORIENTED_EDGE ( 'NONE', *, *, #251, .T. ) ;
#21208 = AXIS2_PLACEMENT_3D ( 'NONE', #23026, #30869, #45797 ) ;
#21209 = CIRCLE ( 'NONE', #7902, 82.00000000000000000 ) ;
#21210 = DIRECTION ( 'NONE',  ( -1.000000000000000000, 0.000000000000000000, 0.000000000000000000 ) ) ;
#21211 = FACE_BOUND ( 'NONE', #36963, .T. ) ;
#21212 = DIRECTION ( 'NONE',  ( 0.000000000000000000, 0.9781476007338045786, -0.2079116908177641720 ) ) ;
#21213 = DIRECTION ( 'NONE',  ( -0.000000000000000000, -0.000000000000000000, -1.000000000000000000 ) ) ;
#21214 = VECTOR ( 'NONE', #3593, 1000.000000000000000 ) ;
#21215 = EDGE_CURVE ( 'NONE', #47807, #13122, #40994, .T. ) ;
#21216 = EDGE_CURVE ( 'NONE', #44810, #44505, #47084, .T. ) ;
#21217 = DIRECTION ( 'NONE',  ( -1.000000000000000000, 0.000000000000000000, 0.000000000000000000 ) ) ;
#21218 = DIRECTION ( 'NONE',  ( -1.000000000000000000, 0.000000000000000000, 0.000000000000000000 ) ) ;
#21219 = ORIENTED_EDGE ( 'NONE', *, *, #26537, .F. ) ;
#21220 = ADVANCED_FACE ( 'NONE', ( #48321 ), #3279, .T. ) ;
#21221 = VECTOR ( 'NONE', #28758, 1000.000000000000000 ) ;
#21222 = LINE ( 'NONE', #25381, #3790 ) ;
#21223 = SHAPE_REPRESENTATION ( 'CIRCLIP DIN 471 - 25 \X2\00d7\X0\ 1.2_GB_CONNECTING_PIECE_RING_RRA 25', ( #11636 ), #12375 ) ;
#21224 = EDGE_LOOP ( 'NONE', ( #20734, #18956, #23876, #37586 ) ) ;
#21225 = CIRCLE ( 'NONE', #43115, 82.00000000000000000 ) ;
#21226 = CARTESIAN_POINT ( 'NONE',  ( 15.00000000000000000, -23.29833615347104470, 3.418703333116808629 ) ) ;
#21227 = DIRECTION ( 'NONE',  ( -1.000000000000000000, 0.000000000000000000, 0.000000000000000000 ) ) ;
#21228 = DIRECTION ( 'NONE',  ( 9.814797785686868941E-17, -1.000000000000000000, 0.000000000000000000 ) ) ;
#21229 = VERTEX_POINT ( 'NONE', #6968 ) ;
#21230 = DIRECTION ( 'NONE',  ( -1.000000000000000000, 0.000000000000000000, 0.000000000000000000 ) ) ;
#21231 = DIRECTION ( 'NONE',  ( 0.000000000000000000, 0.000000000000000000, 1.000000000000000000 ) ) ;
#21232 = ADVANCED_FACE ( 'NONE', ( #14313 ), #40274, .F. ) ;
#21233 = LINE ( 'NONE', #10224, #25531 ) ;
#21234 = LINE ( 'NONE', #17317, #44037 ) ;
#21235 = DIRECTION ( 'NONE',  ( 0.000000000000000000, 0.000000000000000000, 1.000000000000000000 ) ) ;
#21236 = DIRECTION ( 'NONE',  ( -0.6575728627325954090, 0.7533909544171998318, 0.000000000000000000 ) ) ;
#21237 = PRESENTATION_STYLE_ASSIGNMENT (( #47661 ) ) ;
#21238 = ORIENTED_EDGE ( 'NONE', *, *, #36353, .F. ) ;
#21239 = ORIENTED_EDGE ( 'NONE', *, *, #23866, .T. ) ;
#21240 = VECTOR ( 'NONE', #44716, 1000.000000000000000 ) ;
#21241 = VECTOR ( 'NONE', #22601, 1000.000000000000000 ) ;
#21242 = ORIENTED_EDGE ( 'NONE', *, *, #32808, .T. ) ;
#21243 = CARTESIAN_POINT ( 'NONE',  ( 0.000000000000000000, -35.91791733033427647, -68.67312586195032509 ) ) ;
#21244 = AXIS2_PLACEMENT_3D ( 'NONE', #46113, #30955, #39009 ) ;
#21245 = DIRECTION ( 'NONE',  ( 0.000000000000000000, 0.000000000000000000, 1.000000000000000000 ) ) ;
#21246 = ORIENTED_EDGE ( 'NONE', *, *, #3937, .F. ) ;
#21247 = VECTOR ( 'NONE', #26299, 1000.000000000000000 ) ;
#21248 = EDGE_CURVE ( 'NONE', #4261, #20756, #21658, .T. ) ;
#21249 = CARTESIAN_POINT ( 'NONE',  ( 10.00000000000000000, -74.18225833017913828, 34.94270380257611919 ) ) ;
#21250 = AXIS2_PLACEMENT_3D ( 'NONE', #28853, #13931, #32759 ) ;
#21251 = EDGE_CURVE ( 'NONE', #24549, #43507, #36582, .T. ) ;
#21252 = ORIENTED_EDGE ( 'NONE', *, *, #43071, .T. ) ;
#21253 = ORIENTED_EDGE ( 'NONE', *, *, #14704, .T. ) ;
#21254 = ORIENTED_EDGE ( 'NONE', *, *, #14302, .F. ) ;
#21255 = EDGE_CURVE ( 'NONE', #15376, #46628, #44704, .T. ) ;
#21256 = EDGE_CURVE ( 'NONE', #20697, #23468, #36109, .T. ) ;
#21257 = DIRECTION ( 'NONE',  ( -1.000000000000000000, -0.000000000000000000, -0.000000000000000000 ) ) ;
#21258 = ORIENTED_EDGE ( 'NONE', *, *, #45319, .T. ) ;
#21259 = DIRECTION ( 'NONE',  ( -1.000000000000000000, -0.000000000000000000, 0.000000000000000000 ) ) ;
#21260 = EDGE_CURVE ( 'NONE', #28358, #35358, #36815, .T. ) ;
#21261 = VERTEX_POINT ( 'NONE', #11126 ) ;
#21262 = DIRECTION ( 'NONE',  ( -1.000000000000000000, 0.000000000000000000, -0.000000000000000000 ) ) ;
#21263 = AXIS2_PLACEMENT_3D ( 'NONE', #8762, #15631, #33737 ) ;
#21264 = FACE_OUTER_BOUND ( 'NONE', #2513, .T. ) ;
#21265 = CARTESIAN_POINT ( 'NONE',  ( 6.000000000000000000, -81.34940948281344220, 10.30890764327355846 ) ) ;
#21266 = ORIENTED_EDGE ( 'NONE', *, *, #19536, .F. ) ;
#21267 = CARTESIAN_POINT ( 'NONE',  ( 15.00000000000000000, -1.278221433540145391, 26.51162292216073979 ) ) ;
#21268 = ORIENTED_EDGE ( 'NONE', *, *, #27683, .F. ) ;
#21269 = VECTOR ( 'NONE', #42495, 1000.000000000000000 ) ;
#21270 = CARTESIAN_POINT ( 'NONE',  ( 0.000000000000000000, -14.54903810567676636, 22.19967320028756319 ) ) ;
#21271 = CARTESIAN_POINT ( 'NONE',  ( 11.99999999999999822, -64.81221759200306565, -50.23322058963420034 ) ) ;
#21272 = ORIENTED_EDGE ( 'NONE', *, *, #10899, .F. ) ;
#21273 = VERTEX_POINT ( 'NONE', #26047 ) ;
#21274 = EDGE_CURVE ( 'NONE', #18013, #919, #23597, .T. ) ;
#21275 = CARTESIAN_POINT ( 'NONE',  ( 5.999999999999999112, 2.543863470248399761, 81.96053171279903893 ) ) ;
#21276 = CARTESIAN_POINT ( 'NONE',  ( 5.000000000000000000, -40.65526001592664329, 71.21200624218782593 ) ) ;
#21277 = EDGE_LOOP ( 'NONE', ( #37152, #13698, #32189, #25163 ) ) ;
#21278 = ORIENTED_EDGE ( 'NONE', *, *, #48286, .T. ) ;
#21279 = CARTESIAN_POINT ( 'NONE',  ( 10.00000000000000000, -18.89407956138203204, -75.16055320797050854 ) ) ;
#21280 = DIRECTION ( 'NONE',  ( 0.000000000000000000, 0.000000000000000000, 1.000000000000000000 ) ) ;
#21281 = DIRECTION ( 'NONE',  ( 0.8774505977381971134, 0.4796670183876317051, -0.000000000000000000 ) ) ;
#21282 = EDGE_LOOP ( 'NONE', ( #10509, #18331, #21015, #42897, #1716, #19230 ) ) ;
#21283 = DIRECTION ( 'NONE',  ( 0.000000000000000000, 0.000000000000000000, 1.000000000000000000 ) ) ;
#21284 = VECTOR ( 'NONE', #34231, 1000.000000000000000 ) ;
#21285 = CARTESIAN_POINT ( 'NONE',  ( 10.00000000000000000, 5.256550761632864166, 77.32052557432842832 ) ) ;
#21286 = EDGE_CURVE ( 'NONE', #36432, #25492, #20479, .T. ) ;
#21287 = CARTESIAN_POINT ( 'NONE',  ( 0.000000000000000000, 0.000000000000000000, 0.000000000000000000 ) ) ;
#21288 = DIRECTION ( 'NONE',  ( 1.000000000000000000, 0.000000000000000000, 0.000000000000000000 ) ) ;
#21289 = AXIS2_PLACEMENT_3D ( 'NONE', #2577, #5546, #43708 ) ;
#21290 = CARTESIAN_POINT ( 'NONE',  ( 5.000000000000000000, 16.65560815589464028, -38.55633173626993226 ) ) ;
#21291 = DIRECTION ( 'NONE',  ( -1.000000000000000000, -0.000000000000000000, 0.000000000000000000 ) ) ;
#21292 = CARTESIAN_POINT ( 'NONE',  ( 19.29194287201271862, -133.5026271600380880, 5.500000000000000000 ) ) ;
#21293 = ADVANCED_FACE ( 'NONE', ( #34841 ), #45612, .T. ) ;
#21294 = CARTESIAN_POINT ( 'NONE',  ( 0.000000000000000000, 0.000000000000000000, 0.000000000000000000 ) ) ;
#21295 = LINE ( 'NONE', #3668, #42041 ) ;
#21296 = ORIENTED_EDGE ( 'NONE', *, *, #6010, .T. ) ;
#21297 = ORIENTED_EDGE ( 'NONE', *, *, #35529, .F. ) ;
#21298 = EDGE_CURVE ( 'NONE', #40177, #35673, #27525, .T. ) ;
#21299 = DIRECTION ( 'NONE',  ( 0.000000000000000000, 0.4067366430757888285, 0.9135454576426060846 ) ) ;
#21300 = CIRCLE ( 'NONE', #10369, 82.00000000000000000 ) ;
#21301 = AXIS2_PLACEMENT_3D ( 'NONE', #42880, #24037, #39203 ) ;
#21302 = LINE ( 'NONE', #36240, #15926 ) ;
#21303 = ORIENTED_EDGE ( 'NONE', *, *, #38695, .T. ) ;
#21304 = CIRCLE ( 'NONE', #41617, 31.99999999999998579 ) ;
#21305 = EDGE_CURVE ( 'NONE', #28952, #38166, #36930, .T. ) ;
#21306 = ORIENTED_EDGE ( 'NONE', *, *, #39812, .T. ) ;
#21307 = VECTOR ( 'NONE', #14735, 1000.000000000000000 ) ;
#21308 = ADVANCED_FACE ( 'NONE', ( #12107 ), #22856, .T. ) ;
#21309 = CARTESIAN_POINT ( 'NONE',  ( 10.00000000000000000, 0.000000000000000000, 0.000000000000000000 ) ) ;
#21310 = VECTOR ( 'NONE', #38386, 1000.000000000000000 ) ;
#21311 = ORIENTED_EDGE ( 'NONE', *, *, #45248, .T. ) ;
#21312 = FACE_BOUND ( 'NONE', #631, .T. ) ;
#21313 = EDGE_LOOP ( 'NONE', ( #47974, #43117, #12509, #30870 ) ) ;
#21315 = ADVANCED_FACE ( 'NONE', ( #46107 ), #7923, .T. ) ;
#21314 = DIRECTION ( 'NONE',  ( 0.000000000000000000, 0.000000000000000000, 1.000000000000000000 ) ) ;
#21316 = EDGE_CURVE ( 'NONE', #20223, #27571, #11135, .T. ) ;
#21317 = ORIENTED_EDGE ( 'NONE', *, *, #19635, .T. ) ;
#21318 = DIRECTION ( 'NONE',  ( 0.000000000000000000, 0.1045284632676558162, 0.9945218953682731788 ) ) ;
#21319 = AXIS2_PLACEMENT_3D ( 'NONE', #43403, #27996, #1557 ) ;
#21320 = EDGE_CURVE ( 'NONE', #5793, #17817, #2519, .T. ) ;
#21321 = DIRECTION ( 'NONE',  ( 0.4796670183876317051, -0.8774505977381972244, 0.000000000000000000 ) ) ;
#21322 = ORIENTED_EDGE ( 'NONE', *, *, #22221, .F. ) ;
#21323 = DIRECTION ( 'NONE',  ( -1.000000000000000000, 0.000000000000000000, 0.000000000000000000 ) ) ;
#21324 = VECTOR ( 'NONE', #28011, 1000.000000000000000 ) ;
#21325 = ORIENTED_EDGE ( 'NONE', *, *, #12922, .F. ) ;
#21326 = FACE_OUTER_BOUND ( 'NONE', #8410, .T. ) ;
#21327 = ORIENTED_EDGE ( 'NONE', *, *, #33255, .T. ) ;
#21328 = CARTESIAN_POINT ( 'NONE',  ( 10.00000000000000000, -18.89407956138310496, 75.16055320797023853 ) ) ;
#21329 = CARTESIAN_POINT ( 'NONE',  ( 6.000000000000000000, -16.65972982744991171, 80.28980883073752750 ) ) ;
#21330 = DIRECTION ( 'NONE',  ( 0.000000000000000000, 0.000000000000000000, -1.000000000000000000 ) ) ;
#21332 = ORIENTED_EDGE ( 'NONE', *, *, #14592, .F. ) ;
#21331 = DIRECTION ( 'NONE',  ( 0.000000000000000000, 0.000000000000000000, 1.000000000000000000 ) ) ;
#21333 = FACE_OUTER_BOUND ( 'NONE', #39941, .T. ) ;
#21334 = VERTEX_POINT ( 'NONE', #27031 ) ;
#21335 = CARTESIAN_POINT ( 'NONE',  ( 12.00000000000000000, -4.261787119645322974, -26.19803753235774479 ) ) ;
#21336 = EDGE_LOOP ( 'NONE', ( #44274, #12470, #30652, #40638 ) ) ;
#21337 = ORIENTED_EDGE ( 'NONE', *, *, #32121, .T. ) ;
#21338 = CARTESIAN_POINT ( 'NONE',  ( 0.000000000000000000, -68.67312586194971402, -35.91791733033549860 ) ) ;
#21339 = CARTESIAN_POINT ( 'NONE',  ( 0.000000000000000000, 0.000000000000000000, 21.00000000000000000 ) ) ;
#21340 = ORIENTED_EDGE ( 'NONE', *, *, #7535, .F. ) ;
#21341 = DIRECTION ( 'NONE',  ( -1.000000000000000000, 0.000000000000000000, -0.000000000000000000 ) ) ;
#21342 = CARTESIAN_POINT ( 'NONE',  ( 10.00000000000000000, -17.80606268964516659, -33.00180498840066434 ) ) ;
#21343 = CARTESIAN_POINT ( 'NONE',  ( 0.000000000000000000, 20.41045688087930898, -72.35160999960793049 ) ) ;
#21344 = ORIENTED_EDGE ( 'NONE', *, *, #7904, .T. ) ;
#21345 = CARTESIAN_POINT ( 'NONE',  ( 0.000000000000000000, 0.000000000000000000, -54.99999999999998579 ) ) ;
#21346 = CIRCLE ( 'NONE', #16674, 42.00000000000000000 ) ;
#21347 = CARTESIAN_POINT ( 'NONE',  ( 6.782329983125267248, 10.49999999999999645, -105.0000000000000000 ) ) ;
#21348 = CARTESIAN_POINT ( 'NONE',  ( 11.99999999999999822, 0.000000000000000000, 0.000000000000000000 ) ) ;
#21349 = CIRCLE ( 'NONE', #44790, 77.49899999999999523 ) ;
#21350 = CARTESIAN_POINT ( 'NONE',  ( 0.000000000000000000, 0.000000000000000000, 0.000000000000000000 ) ) ;
#21351 = CARTESIAN_POINT ( 'NONE',  ( 0.000000000000000000, 0.000000000000000000, 0.000000000000000000 ) ) ;
#21352 = PLANE ( 'NONE',  #19171 ) ;
#21353 = CARTESIAN_POINT ( 'NONE',  ( 0.000000000000000000, 75.11725578898472122, -2.956366410619845730 ) ) ;
#21354 = CARTESIAN_POINT ( 'NONE',  ( 12.49999999999999822, -120.0000000000000000, 125.0000000000000000 ) ) ;
#21355 = AXIS2_PLACEMENT_3D ( 'NONE', #25847, #7256, #22189 ) ;
#21356 = AXIS2_PLACEMENT_3D ( 'NONE', #42792, #39612, #20985 ) ;
#21357 = CIRCLE ( 'NONE', #19010, 37.49900000000000233 ) ;
#21358 = CARTESIAN_POINT ( 'NONE',  ( -13.05994868825747446, -139.5943292883446532, 5.500000000000000000 ) ) ;
#21359 = CARTESIAN_POINT ( 'NONE',  ( 0.000000000000000000, 41.76937507738788469, 62.50329211542452157 ) ) ;
#21360 = CIRCLE ( 'NONE', #26855, 31.99999999999998224 ) ;
#21361 = ORIENTED_EDGE ( 'NONE', *, *, #43823, .F. ) ;
#21362 = CARTESIAN_POINT ( 'NONE',  ( 0.000000000000000000, 37.22597642581150268, 5.202137450157037435 ) ) ;
#21363 = CIRCLE ( 'NONE', #12013, 42.00000000000000000 ) ;
#21364 = VERTEX_POINT ( 'NONE', #12343 ) ;
#21365 = DIRECTION ( 'NONE',  ( 0.000000000000000000, -0.9510565162951499785, -0.3090169943749582204 ) ) ;
#21366 = CIRCLE ( 'NONE', #42479, 31.99999999999999645 ) ;
#21367 = FACE_OUTER_BOUND ( 'NONE', #37270, .T. ) ;
#21368 = AXIS2_PLACEMENT_3D ( 'NONE', #23472, #45505, #26927 ) ;
#21369 = VERTEX_POINT ( 'NONE', #4985 ) ;
#21370 = EDGE_CURVE ( 'NONE', #41616, #24887, #32238, .T. ) ;
#21371 = DIRECTION ( 'NONE',  ( 0.000000000000000000, 0.000000000000000000, -1.000000000000000000 ) ) ;
#21372 = VERTEX_POINT ( 'NONE', #27510 ) ;
#21373 = EDGE_CURVE ( 'NONE', #17814, #20223, #23630, .T. ) ;
#21374 = ORIENTED_EDGE ( 'NONE', *, *, #44526, .T. ) ;
#21375 = AXIS2_PLACEMENT_3D ( 'NONE', #12469, #42319, #19311 ) ;
#21376 = ADVANCED_FACE ( 'NONE', ( #37790 ), #41964, .F. ) ;
#21377 = DIRECTION ( 'NONE',  ( -0.8090169943749504489, 0.5877852522924689183, 0.000000000000000000 ) ) ;
#21378 = ORIENTED_EDGE ( 'NONE', *, *, #11064, .T. ) ;
#21379 = EDGE_CURVE ( 'NONE', #12299, #25561, #19187, .T. ) ;
#21380 = DIRECTION ( 'NONE',  ( -1.000000000000000000, 0.000000000000000000, 0.000000000000000000 ) ) ;
#21381 = VECTOR ( 'NONE', #813, 1000.000000000000000 ) ;
#21382 = AXIS2_PLACEMENT_3D ( 'NONE', #21940, #14852, #43513 ) ;
#21383 = CARTESIAN_POINT ( 'NONE',  ( 5.822613034544236399, -142.8165987265839760, -5.500000000000000000 ) ) ;
#21384 = AXIS2_PLACEMENT_3D ( 'NONE', #12771, #27467, #35038 ) ;
#21385 = ORIENTED_EDGE ( 'NONE', *, *, #1337, .T. ) ;
#21386 = DIRECTION ( 'NONE',  ( -1.000000000000000000, -0.000000000000000000, -0.000000000000000000 ) ) ;
#21387 = ADVANCED_FACE ( 'NONE', ( #45370 ), #34113, .T. ) ;
#21388 = ORIENTED_EDGE ( 'NONE', *, *, #47620, .T. ) ;
#21389 = DIRECTION ( 'NONE',  ( 0.000000000000000000, -0.4539904997395351471, -0.8910065241883737830 ) ) ;
#21390 = CARTESIAN_POINT ( 'NONE',  ( -3.000000000000000000, 0.000000000000000000, 0.000000000000000000 ) ) ;
#21391 = CYLINDRICAL_SURFACE ( 'NONE', #46275, 82.00000000000000000 ) ;
#21392 = AXIS2_PLACEMENT_3D ( 'NONE', #26505, #8140, #30190 ) ;
#21393 = CIRCLE ( 'NONE', #37049, 77.49899999999999523 ) ;
#21394 = VERTEX_POINT ( 'NONE', #11849 ) ;
#21395 = CARTESIAN_POINT ( 'NONE',  ( 23.41451323550360186, -132.5004227906269989, 5.500000000000000000 ) ) ;
#21396 = ORIENTED_EDGE ( 'NONE', *, *, #20720, .T. ) ;
#21397 = ORIENTED_EDGE ( 'NONE', *, *, #45642, .F. ) ;
#21398 = VECTOR ( 'NONE', #15464, 1000.000000000000000 ) ;
#21399 = DIRECTION ( 'NONE',  ( -1.000000000000000000, 0.000000000000000000, 0.000000000000000000 ) ) ;
#21400 = AXIS2_PLACEMENT_3D ( 'NONE', #34011, #15429, #30361 ) ;
#21401 = CARTESIAN_POINT ( 'NONE',  ( 6.000000000000000000, -79.10210256391383155, 21.60688246758558506 ) ) ;
#21402 = DIRECTION ( 'NONE',  ( 1.000000000000000000, 0.000000000000000000, 0.000000000000000000 ) ) ;
#21403 = DIRECTION ( 'NONE',  ( -1.000000000000000000, 0.000000000000000000, 0.000000000000000000 ) ) ;
#21404 = DIRECTION ( 'NONE',  ( 0.000000000000000000, -0.9510565162951565288, 0.3090169943749384029 ) ) ;
#21405 = AXIS2_PLACEMENT_3D ( 'NONE', #21855, #26276, #8385 ) ;
#21406 = LINE ( 'NONE', #9193, #38536 ) ;
#21407 = DIRECTION ( 'NONE',  ( 0.000000000000000000, -0.9723699203976789995, 0.2334453638558956212 ) ) ;
#21408 = DIRECTION ( 'NONE',  ( -1.000000000000000000, -0.000000000000000000, 0.000000000000000000 ) ) ;
#21409 = CARTESIAN_POINT ( 'NONE',  ( -3.000000000000000000, -14.54903810567645195, -22.19967320028775504 ) ) ;
#21410 = DIRECTION ( 'NONE',  ( -1.000000000000000000, -0.000000000000000000, -0.000000000000000000 ) ) ;
#21411 = VERTEX_POINT ( 'NONE', #26774 ) ;
#21412 = VERTEX_POINT ( 'NONE', #23341 ) ;
#21413 = DIRECTION ( 'NONE',  ( -1.000000000000000000, 0.000000000000000000, -0.000000000000000000 ) ) ;
#21414 = CARTESIAN_POINT ( 'NONE',  ( 0.000000000000000000, -25.60904388321925396, 6.976881207771172377 ) ) ;
#21415 = CARTESIAN_POINT ( 'NONE',  ( 16.84844760790522855, -103.5491698323862124, -5.500000000000000000 ) ) ;
#21416 = DIRECTION ( 'NONE',  ( 0.000000000000000000, 0.000000000000000000, -1.000000000000000000 ) ) ;
#21417 = AXIS2_PLACEMENT_3D ( 'NONE', #3854, #14394, #169 ) ;
#21418 = CIRCLE ( 'NONE', #16058, 82.00000000000000000 ) ;
#21419 = EDGE_CURVE ( 'NONE', #12997, #31342, #47864, .T. ) ;
#21420 = LINE ( 'NONE', #17256, #38872 ) ;
#21421 = DIRECTION ( 'NONE',  ( 0.000000000000000000, 0.000000000000000000, 1.000000000000000000 ) ) ;
#21422 = VERTEX_POINT ( 'NONE', #4509 ) ;
#21423 = CIRCLE ( 'NONE', #37854, 82.00000000000000000 ) ;
#21424 = CARTESIAN_POINT ( 'NONE',  ( 11.99999999999999822, 0.000000000000000000, 0.000000000000000000 ) ) ;
#21425 = CIRCLE ( 'NONE', #25329, 31.99999999999998579 ) ;
#21426 = ADVANCED_FACE ( 'NONE', ( #19414 ), #817, .T. ) ;
#21427 = VECTOR ( 'NONE', #39475, 1000.000000000000000 ) ;
#21428 = PRODUCT ( 'BR-543', 'BR-543', '', ( #38169 ) ) ;
#21429 = ADVANCED_FACE ( 'NONE', ( #39496 ), #9606, .T. ) ;
#21430 = CARTESIAN_POINT ( 'NONE',  ( 10.00000000000000000, 35.38097989696512968, 12.42422080174651100 ) ) ;
#21431 = ORIENTED_EDGE ( 'NONE', *, *, #35086, .F. ) ;
#21432 = ORIENTED_EDGE ( 'NONE', *, *, #31497, .T. ) ;
#21433 = AXIS2_PLACEMENT_3D ( 'NONE', #16610, #31562, #12959 ) ;
#21434 = AXIS2_PLACEMENT_3D ( 'NONE', #16205, #46061, #24028 ) ;
#21435 = ORIENTED_EDGE ( 'NONE', *, *, #9013, .F. ) ;
#21436 = AXIS2_PLACEMENT_3D ( 'NONE', #31090, #46247, #27647 ) ;
#21437 = CARTESIAN_POINT ( 'NONE',  ( 6.509281303079589520, -14.89695620656361008, -1.199999999999999956 ) ) ;
#21438 = EDGE_CURVE ( 'NONE', #42832, #14950, #29881, .T. ) ;
#21439 = EDGE_LOOP ( 'NONE', ( #8491, #31290, #19297, #21008 ) ) ;
#21440 = CIRCLE ( 'NONE', #16770, 16.00000000000000000 ) ;
#21441 = EDGE_CURVE ( 'NONE', #8888, #1459, #39290, .T. ) ;
#21442 = ADVANCED_FACE ( 'NONE', ( #20885 ), #35809, .T. ) ;
#21443 = EDGE_LOOP ( 'NONE', ( #46183, #17631, #3250, #47845 ) ) ;
#21444 = CARTESIAN_POINT ( 'NONE',  ( -3.000000000000000000, 5.835314593368477354, 22.81335362449854642 ) ) ;
#21445 = CARTESIAN_POINT ( 'NONE',  ( -10.00000000000000000, 0.000000000000000000, 0.000000000000000000 ) ) ;
#21446 = CARTESIAN_POINT ( 'NONE',  ( 10.00000000000000000, -78.73519480814938731, -22.90783923731713756 ) ) ;
#21447 = VERTEX_POINT ( 'NONE', #24796 ) ;
#21448 = DIRECTION ( 'NONE',  ( -1.000000000000000000, -0.000000000000000000, -0.000000000000000000 ) ) ;
#21449 = EDGE_LOOP ( 'NONE', ( #43239, #32247, #30607, #30354 ) ) ;
#21450 = AXIS2_PLACEMENT_3D ( 'NONE', #41415, #22806, #44837 ) ;
#21451 = VERTEX_POINT ( 'NONE', #5711 ) ;
#21452 = ORIENTED_EDGE ( 'NONE', *, *, #30261, .T. ) ;
#21453 = DIRECTION ( 'NONE',  ( -1.000000000000000000, -0.000000000000000000, -0.000000000000000000 ) ) ;
#21454 = ADVANCED_FACE ( 'NONE', ( #47066 ), #31924, .T. ) ;
#21456 = ORIENTED_EDGE ( 'NONE', *, *, #35320, .F. ) ;
#21455 = CARTESIAN_POINT ( 'NONE',  ( 10.00000000000000000, 0.000000000000000000, 0.000000000000000000 ) ) ;
#21458 = DIRECTION ( 'NONE',  ( 1.000000000000000000, -0.000000000000000000, 0.000000000000000000 ) ) ;
#21457 = AXIS2_PLACEMENT_3D ( 'NONE', #7805, #14916, #15881 ) ;
#21459 = ORIENTED_EDGE ( 'NONE', *, *, #12315, .F. ) ;
#21460 = ORIENTED_EDGE ( 'NONE', *, *, #24042, .F. ) ;
#21461 = DIRECTION ( 'NONE',  ( 1.000000000000000000, 0.000000000000000000, -0.000000000000000000 ) ) ;
#21462 = ORIENTED_EDGE ( 'NONE', *, *, #16951, .F. ) ;
#21463 = VECTOR ( 'NONE', #31731, 1000.000000000000114 ) ;
#21464 = DIRECTION ( 'NONE',  ( 0.000000000000000000, 0.000000000000000000, 1.000000000000000000 ) ) ;
#21465 = VECTOR ( 'NONE', #37561, 1000.000000000000000 ) ;
#21466 = DIRECTION ( 'NONE',  ( 0.000000000000000000, -0.3090169943749349057, -0.9510565162951576390 ) ) ;
#21467 = ORIENTED_EDGE ( 'NONE', *, *, #35655, .F. ) ;
#21468 = DIRECTION ( 'NONE',  ( -1.000000000000000000, -0.000000000000000000, -0.000000000000000000 ) ) ;
#21469 = CARTESIAN_POINT ( 'NONE',  ( 0.000000000000000000, -41.91543099594816368, -2.663952781846588014 ) ) ;
#21470 = FILL_AREA_STYLE_COLOUR ( '', #12500 ) ;
#21471 = LINE ( 'NONE', #9972, #38420 ) ;
#21472 = AXIS2_PLACEMENT_3D ( 'NONE', #32935, #14348, #29278 ) ;
#21473 = CIRCLE ( 'NONE', #30072, 77.49899999999999523 ) ;
#21474 = ORIENTED_EDGE ( 'NONE', *, *, #37861, .F. ) ;
#21475 = AXIS2_PLACEMENT_3D ( 'NONE', #14382, #14632, #48384 ) ;
#21476 = CARTESIAN_POINT ( 'NONE',  ( 11.99999999999999822, -46.54456581323847786, 59.03342792756247093 ) ) ;
#21477 = ORIENTED_EDGE ( 'NONE', *, *, #28636, .F. ) ;
#21478 = VECTOR ( 'NONE', #11814, 1000.000000000000000 ) ;
#21479 = AXIS2_PLACEMENT_3D ( 'NONE', #14736, #37242, #11313 ) ;
#21480 = CARTESIAN_POINT ( 'NONE',  ( 10.00000000000000000, 81.96053171279901051, 2.543863470248666658 ) ) ;
#21481 = FACE_OUTER_BOUND ( 'NONE', #13452, .T. ) ;
#21482 = LINE ( 'NONE', #32505, #43240 ) ;
#21483 = AXIS2_PLACEMENT_3D ( 'NONE', #26585, #7966, #19236 ) ;
#21484 = EDGE_CURVE ( 'NONE', #25099, #34175, #47953, .T. ) ;
#21485 = FACE_OUTER_BOUND ( 'NONE', #29192, .T. ) ;
#21486 = DIRECTION ( 'NONE',  ( 1.000000000000000000, -0.000000000000000000, 0.000000000000000000 ) ) ;
#21487 = ORIENTED_EDGE ( 'NONE', *, *, #27844, .T. ) ;
#21488 = EDGE_CURVE ( 'NONE', #8273, #15618, #38487, .T. ) ;
#21489 = CARTESIAN_POINT ( 'NONE',  ( 4.999999999999999112, 2.663952781846732343, -41.91543099594814947 ) ) ;
#21490 = CARTESIAN_POINT ( 'NONE',  ( 10.00000000000000000, -10.41901085202050403, -40.68715046381940681 ) ) ;
#21491 = DIRECTION ( 'NONE',  ( -1.000000000000000000, 0.000000000000000000, -0.000000000000000000 ) ) ;
#21492 = EDGE_CURVE ( 'NONE', #22246, #30938, #28221, .T. ) ;
#21493 = PLANE ( 'NONE',  #44019 ) ;
#21494 = SHAPE_REPRESENTATION_RELATIONSHIP ( 'NONE' , 'NONE' ,  #12525, #21055 ) ;
#21495 = EDGE_CURVE ( 'NONE', #4190, #42528, #20153, .T. ) ;
#21496 = EDGE_LOOP ( 'NONE', ( #21921, #35043, #39977, #12275 ) ) ;
#21497 = ORIENTED_EDGE ( 'NONE', *, *, #48082, .T. ) ;
#21498 = ORIENTED_EDGE ( 'NONE', *, *, #9276, .F. ) ;
#21499 = VECTOR ( 'NONE', #31553, 1000.000000000000000 ) ;
#21500 = AXIS2_PLACEMENT_3D ( 'NONE', #7448, #22380, #3766 ) ;
#21501 = VERTEX_POINT ( 'NONE', #28465 ) ;
#21502 = CARTESIAN_POINT ( 'NONE',  ( 0.000000000000000000, -51.29473840253269401, 63.97538442413407012 ) ) ;
#21503 = CYLINDRICAL_SURFACE ( 'NONE', #4268, 77.49899999999999523 ) ;
#21504 = ORIENTED_EDGE ( 'NONE', *, *, #27527, .T. ) ;
#21505 = ADVANCED_FACE ( 'NONE', ( #13297 ), #20632, .T. ) ;
#21506 = ADVANCED_FACE ( 'NONE', ( #23835 ), #35321, .T. ) ;
#21507 = CIRCLE ( 'NONE', #24624, 31.99999999999998579 ) ;
#21508 = CIRCLE ( 'NONE', #14456, 31.99999999999999289 ) ;
#21509 = DIRECTION ( 'NONE',  ( -1.000000000000000000, -0.000000000000000000, -0.000000000000000000 ) ) ;
#21510 = VERTEX_POINT ( 'NONE', #39738 ) ;
#21511 = EDGE_LOOP ( 'NONE', ( #21119, #19392, #14353, #23478 ) ) ;
#21512 = AXIS2_PLACEMENT_3D ( 'NONE', #45430, #14185, #14678 ) ;
#21513 = ORIENTED_EDGE ( 'NONE', *, *, #12767, .F. ) ;
#21514 = CIRCLE ( 'NONE', #416, 31.99999999999998934 ) ;
#21515 = CIRCLE ( 'NONE', #3554, 16.00000000000000000 ) ;
#21516 = ADVANCED_FACE ( 'NONE', ( #1560 ), #35574, .T. ) ;
#21517 = CARTESIAN_POINT ( 'NONE',  ( 2.874421927457452952, -143.3717286177755739, 5.500000000000000000 ) ) ;
#21518 = CIRCLE ( 'NONE', #420, 16.00000000000000000 ) ;
#21519 = EDGE_LOOP ( 'NONE', ( #39768, #24972, #32474, #21258 ) ) ;
#21520 = LINE ( 'NONE', #47458, #47377 ) ;
#21521 = ORIENTED_EDGE ( 'NONE', *, *, #20494, .T. ) ;
#21522 = LINE ( 'NONE', #25171, #8751 ) ;
#21523 = DIRECTION ( 'NONE',  ( -1.000000000000000000, -0.000000000000000000, -0.000000000000000000 ) ) ;
#21524 = CARTESIAN_POINT ( 'NONE',  ( 0.000000000000000000, -5.256550761632340141, -77.32052557432847095 ) ) ;
#21525 = VERTEX_POINT ( 'NONE', #38778 ) ;
#21526 = CARTESIAN_POINT ( 'NONE',  ( 11.99999999999999822, 0.000000000000000000, 0.000000000000000000 ) ) ;
#21527 = ORIENTED_EDGE ( 'NONE', *, *, #40914, .F. ) ;
#21528 = DIRECTION ( 'NONE',  ( -1.000000000000000000, -0.000000000000000000, -0.000000000000000000 ) ) ;
#21529 = AXIS2_PLACEMENT_3D ( 'NONE', #30455, #15764, #30691 ) ;
#21530 = PLANE ( 'NONE',  #41538 ) ;
#21531 = ORIENTED_EDGE ( 'NONE', *, *, #6612, .T. ) ;
#21532 = ORIENTED_EDGE ( 'NONE', *, *, #661, .T. ) ;
#21533 = DIRECTION ( 'NONE',  ( 0.000000000000000000, 0.000000000000000000, 1.000000000000000000 ) ) ;
#21534 = CARTESIAN_POINT ( 'NONE',  ( 11.99999999999999822, 73.44644590900061587, 24.73286445877730699 ) ) ;
#21535 = EDGE_LOOP ( 'NONE', ( #20976, #37410, #8484, #43497 ) ) ;
#21536 = ORIENTED_EDGE ( 'NONE', *, *, #41321, .F. ) ;
#21537 = DIRECTION ( 'NONE',  ( 0.000000000000000000, 0.000000000000000000, 1.000000000000000000 ) ) ;
#21538 = PLANE ( 'NONE',  #75 ) ;
#21539 = CYLINDRICAL_SURFACE ( 'NONE', #10427, 32.00000000000000000 ) ;
#21540 = ORIENTED_EDGE ( 'NONE', *, *, #25375, .T. ) ;
#21541 = DIRECTION ( 'NONE',  ( 0.000000000000000000, 0.000000000000000000, -1.000000000000000000 ) ) ;
#21542 = CARTESIAN_POINT ( 'NONE',  ( 0.000000000000000000, 73.44644590900061587, 24.73286445877730699 ) ) ;
#21543 = AXIS2_PLACEMENT_3D ( 'NONE', #35783, #6172, #43379 ) ;
#21544 = AXIS2_PLACEMENT_3D ( 'NONE', #28971, #18443, #25290 ) ;
#21545 = DIRECTION ( 'NONE',  ( 1.000000000000000000, 0.000000000000000000, 0.000000000000000000 ) ) ;
#21546 = FACE_OUTER_BOUND ( 'NONE', #13139, .T. ) ;
#21547 = EDGE_CURVE ( 'NONE', #27887, #42524, #24308, .T. ) ;
#21548 = AXIS2_PLACEMENT_3D ( 'NONE', #4280, #7205, #22133 ) ;
#21549 = DIRECTION ( 'NONE',  ( 0.000000000000000000, 0.9723699203976773342, -0.2334453638559026156 ) ) ;
#21550 = FACE_OUTER_BOUND ( 'NONE', #34320, .T. ) ;
#21551 = EDGE_CURVE ( 'NONE', #22095, #30146, #8777, .T. ) ;
#21552 =( LENGTH_UNIT ( ) NAMED_UNIT ( * ) SI_UNIT ( .MILLI., .METRE. ) );
#21553 = VECTOR ( 'NONE', #12332, 999.9999999999998863 ) ;
#21554 = CYLINDRICAL_SURFACE ( 'NONE', #47483, 31.99999999999999289 ) ;
#21555 = EDGE_CURVE ( 'NONE', #4566, #24540, #31681, .T. ) ;
#21556 = ORIENTED_EDGE ( 'NONE', *, *, #10799, .F. ) ;
#21557 = ORIENTED_EDGE ( 'NONE', *, *, #45938, .T. ) ;
#21558 = EDGE_CURVE ( 'NONE', #28265, #13104, #28352, .T. ) ;
#21559 = CARTESIAN_POINT ( 'NONE',  ( 0.000000000000000000, -37.58145647212453611, -0.6853352020794456489 ) ) ;
#21560 = AXIS2_PLACEMENT_3D ( 'NONE', #12378, #20191, #35355 ) ;
#21561 = VECTOR ( 'NONE', #33167, 1000.000000000000114 ) ;
#21562 = DIRECTION ( 'NONE',  ( -0.000000000000000000, 0.9510565162951539753, -0.3090169943749460635 ) ) ;
#21563 = ORIENTED_EDGE ( 'NONE', *, *, #25668, .F. ) ;
#21564 = EDGE_CURVE ( 'NONE', #199, #9856, #41357, .T. ) ;
#21565 = VECTOR ( 'NONE', #18646, 1000.000000000000000 ) ;
#21566 = ORIENTED_EDGE ( 'NONE', *, *, #12331, .T. ) ;
#21567 = ADVANCED_FACE ( 'NONE', ( #18812 ), #22983, .T. ) ;
#21568 = CARTESIAN_POINT ( 'NONE',  ( 10.00000000000000000, 0.000000000000000000, 0.000000000000000000 ) ) ;
#21569 = DIRECTION ( 'NONE',  ( 0.000000000000000000, 0.000000000000000000, 1.000000000000000000 ) ) ;
#21570 = ORIENTED_EDGE ( 'NONE', *, *, #15106, .F. ) ;
#21571 = EDGE_CURVE ( 'NONE', #1311, #15059, #18342, .T. ) ;
#21572 = VECTOR ( 'NONE', #42838, 1000.000000000000000 ) ;
#21573 = DIRECTION ( 'NONE',  ( 0.000000000000000000, 0.000000000000000000, 1.000000000000000000 ) ) ;
#21574 = DIRECTION ( 'NONE',  ( -1.000000000000000000, -0.000000000000000000, -0.000000000000000000 ) ) ;
#21575 = EDGE_LOOP ( 'NONE', ( #28498, #2796, #12473, #17207, #42594 ) ) ;
#21576 = CARTESIAN_POINT ( 'NONE',  ( -11.59999999999999787, 0.000000000000000000, -43.79999999999998295 ) ) ;
#21577 = ORIENTED_EDGE ( 'NONE', *, *, #46858, .F. ) ;
#21578 = VECTOR ( 'NONE', #14507, 1000.000000000000000 ) ;
#21579 = DIRECTION ( 'NONE',  ( -1.000000000000000000, -0.000000000000000000, -0.000000000000000000 ) ) ;
#21580 = ORIENTED_EDGE ( 'NONE', *, *, #28892, .T. ) ;
#21581 = CARTESIAN_POINT ( 'NONE',  ( 10.00000000000000000, -30.41916302227060598, -71.27951684758059514 ) ) ;
#21582 = CIRCLE ( 'NONE', #486, 77.49899999999999523 ) ;
#21583 = ORIENTED_EDGE ( 'NONE', *, *, #2078, .T. ) ;
#21584 = CARTESIAN_POINT ( 'NONE',  ( 6.000000000000000000, -40.65526001592564853, -71.21200624218839437 ) ) ;
#21585 = LINE ( 'NONE', #14234, #26282 ) ;
#21586 = EDGE_CURVE ( 'NONE', #14862, #45459, #14919, .T. ) ;
#21588 = ORIENTED_EDGE ( 'NONE', *, *, #5423, .T. ) ;
#21587 = CARTESIAN_POINT ( 'NONE',  ( 15.00000000000000000, 23.59884966291538078, 12.14883922797231008 ) ) ;
#21589 = DIRECTION ( 'NONE',  ( -1.000000000000000000, -0.000000000000000000, -0.000000000000000000 ) ) ;
#21590 = ORIENTED_EDGE ( 'NONE', *, *, #24155, .F. ) ;
#21591 = AXIS2_PLACEMENT_3D ( 'NONE', #11140, #34356, #602 ) ;
#21592 = CARTESIAN_POINT ( 'NONE',  ( 5.000000000000000000, -36.13751322684404244, -21.40280677340410165 ) ) ;
#21593 = VERTEX_POINT ( 'NONE', #4149 ) ;
#21594 = ORIENTED_EDGE ( 'NONE', *, *, #16928, .F. ) ;
#21595 = CARTESIAN_POINT ( 'NONE',  ( 15.00000000000000000, 20.85821328998741109, -10.92862929874522671 ) ) ;
#21596 = CARTESIAN_POINT ( 'NONE',  ( 0.000000000000000000, -39.04073710021332744, -15.48615015657624028 ) ) ;
#21597 = ORIENTED_EDGE ( 'NONE', *, *, #42796, .F. ) ;
#21598 = DIRECTION ( 'NONE',  ( -1.000000000000000000, 0.000000000000000000, 0.000000000000000000 ) ) ;
#21599 = VECTOR ( 'NONE', #26488, 1000.000000000000000 ) ;
#21600 = DIRECTION ( 'NONE',  ( 0.000000000000000000, 0.9510565162951544194, -0.3090169943749448977 ) ) ;
#21601 = CARTESIAN_POINT ( 'NONE',  ( 10.00000000000000000, -27.05870788708213226, -26.08949754953053102 ) ) ;
#21602 = ORIENTED_EDGE ( 'NONE', *, *, #29938, .T. ) ;
#21603 = DIRECTION ( 'NONE',  ( 0.000000000000000000, 0.000000000000000000, -1.000000000000000000 ) ) ;
#21604 = CARTESIAN_POINT ( 'NONE',  ( 0.000000000000000000, 2.663952781846728790, -41.91543099594814947 ) ) ;
#21605 = VECTOR ( 'NONE', #14923, 1000.000000000000000 ) ;
#21606 = DIRECTION ( 'NONE',  ( -0.02332147558787823691, -0.9997280174009349762, 0.000000000000000000 ) ) ;
#21607 = ORIENTED_EDGE ( 'NONE', *, *, #22115, .F. ) ;
#21608 = CARTESIAN_POINT ( 'NONE',  ( 10.00000000000000000, 59.03961581697465277, -46.53671651293886669 ) ) ;
#21609 = DIRECTION ( 'NONE',  ( -1.000000000000000000, 0.000000000000000000, -0.000000000000000000 ) ) ;
#21610 = CARTESIAN_POINT ( 'NONE',  ( 10.00000000000000000, -79.10210256391383155, 21.60688246758557796 ) ) ;
#21611 = CARTESIAN_POINT ( 'NONE',  ( 11.99999999999999822, 74.65491531819118620, 23.16904090965732621 ) ) ;
#21612 = EDGE_CURVE ( 'NONE', #17963, #48059, #15413, .T. ) ;
#21613 = EDGE_CURVE ( 'NONE', #8546, #44380, #33744, .T. ) ;
#21614 = VERTEX_POINT ( 'NONE', #702 ) ;
#21615 = LINE ( 'NONE', #43415, #16607 ) ;
#21616 = DIRECTION ( 'NONE',  ( 0.000000000000000000, 0.9969173337331276308, 0.07845909572784873220 ) ) ;
#21617 = CARTESIAN_POINT ( 'NONE',  ( 10.00000000000000000, -75.16055320797043748, 18.89407956138229494 ) ) ;
#21618 = CARTESIAN_POINT ( 'NONE',  ( 0.000000000000000000, -50.95692526931287603, -58.39081064771804819 ) ) ;
#21619 = EDGE_CURVE ( 'NONE', #8377, #36404, #29367, .T. ) ;
#21620 = ORIENTED_EDGE ( 'NONE', *, *, #47504, .T. ) ;
#21621 = ORIENTED_EDGE ( 'NONE', *, *, #7540, .T. ) ;
#21622 = FACE_OUTER_BOUND ( 'NONE', #31668, .T. ) ;
#21623 = ORIENTED_EDGE ( 'NONE', *, *, #24428, .F. ) ;
#21624 = ADVANCED_FACE ( 'NONE', ( #10767 ), #15171, .F. ) ;
#21625 = CARTESIAN_POINT ( 'NONE',  ( 0.000000000000000000, 0.000000000000000000, 0.000000000000000000 ) ) ;
#21626 = ORIENTED_EDGE ( 'NONE', *, *, #9842, .F. ) ;
#21627 = VECTOR ( 'NONE', #45816, 1000.000000000000000 ) ;
#21628 = DIRECTION ( 'NONE',  ( -1.000000000000000000, -0.000000000000000000, -0.000000000000000000 ) ) ;
#21629 = ORIENTED_EDGE ( 'NONE', *, *, #27527, .F. ) ;
#21630 = AXIS2_PLACEMENT_3D ( 'NONE', #26905, #38158, #8296 ) ;
#21631 = LINE ( 'NONE', #7658, #38564 ) ;
#21632 = EDGE_LOOP ( 'NONE', ( #48383, #2190, #37883, #26513 ) ) ;
#21633 = AXIS2_PLACEMENT_3D ( 'NONE', #10949, #25866, #40808 ) ;
#21634 = PLANE ( 'NONE',  #37025 ) ;
#21635 = CYLINDRICAL_SURFACE ( 'NONE', #20997, 31.99999999999998579 ) ;
#21636 = CYLINDRICAL_SURFACE ( 'NONE', #15263, 12.49999999999999822 ) ;
#21637 = ORIENTED_EDGE ( 'NONE', *, *, #16352, .F. ) ;
#21638 = CYLINDRICAL_SURFACE ( 'NONE', #1997, 31.99999999999999289 ) ;
#21639 = VERTEX_POINT ( 'NONE', #30097 ) ;
#21640 = AXIS2_PLACEMENT_3D ( 'NONE', #4514, #346, #22860 ) ;
#21641 = FACE_OUTER_BOUND ( 'NONE', #10434, .T. ) ;
#21642 = DIRECTION ( 'NONE',  ( -1.000000000000000000, 0.000000000000000000, 0.000000000000000000 ) ) ;
#21643 = CARTESIAN_POINT ( 'NONE',  ( 0.000000000000000000, -22.64427369931191336, 30.00120703465197280 ) ) ;
#21644 = CIRCLE ( 'NONE', #31836, 31.99999999999998934 ) ;
#21645 = ORIENTED_EDGE ( 'NONE', *, *, #19790, .F. ) ;
#21646 = DIRECTION ( 'NONE',  ( 0.8541291221503261033, -0.5200609990133016058, 0.000000000000000000 ) ) ;
#21647 = EDGE_LOOP ( 'NONE', ( #31406, #34882, #21566, #9060 ) ) ;
#21648 = ORIENTED_EDGE ( 'NONE', *, *, #20894, .T. ) ;
#21649 = CARTESIAN_POINT ( 'NONE',  ( 10.00000000000000000, -69.42325613327466272, 34.44570377933573724 ) ) ;
#21650 = AXIS2_PLACEMENT_3D ( 'NONE', #46726, #13184, #20768 ) ;
#21651 = DIRECTION ( 'NONE',  ( 1.000000000000000000, 0.000000000000000000, -0.000000000000000000 ) ) ;
#21652 = DIRECTION ( 'NONE',  ( -1.000000000000000000, -0.000000000000000000, -0.000000000000000000 ) ) ;
#21653 = CARTESIAN_POINT ( 'NONE',  ( 11.99999999999999822, -5.256550761632340141, -77.32052557432847095 ) ) ;
#21654 = ORIENTED_EDGE ( 'NONE', *, *, #30904, .F. ) ;
#21655 = CARTESIAN_POINT ( 'NONE',  ( -10.00000000000000000, 0.000000000000000000, 0.000000000000000000 ) ) ;
#21656 = CYLINDRICAL_SURFACE ( 'NONE', #40105, 35.50000000000001421 ) ;
#21657 = CARTESIAN_POINT ( 'NONE',  ( 10.00000000000000000, -72.35432306680469594, -20.40083707022958848 ) ) ;
#21658 = LINE ( 'NONE', #14799, #13472 ) ;
#21659 = DIRECTION ( 'NONE',  ( 0.000000000000000000, 0.2334453638558990907, 0.9723699203976781114 ) ) ;
#21660 = ORIENTED_EDGE ( 'NONE', *, *, #37797, .T. ) ;
#21661 = AXIS2_PLACEMENT_3D ( 'NONE', #22622, #38048, #595 ) ;
#21662 = VERTEX_POINT ( 'NONE', #45260 ) ;
#21663 = CARTESIAN_POINT ( 'NONE',  ( 10.00000000000000000, 69.42325613327439271, 34.44570377933623462 ) ) ;
#21664 = EDGE_CURVE ( 'NONE', #42774, #32530, #40062, .T. ) ;
#21665 = DIRECTION ( 'NONE',  ( -0.7273375899149812085, 0.6862798483830533369, 0.000000000000000000 ) ) ;
#21666 = LINE ( 'NONE', #10892, #44851 ) ;
#21667 = EDGE_CURVE ( 'NONE', #43612, #26338, #10357, .T. ) ;
#21668 = CARTESIAN_POINT ( 'NONE',  ( -0.8815729230226008184, -93.47222532549339746, 5.500000000000000000 ) ) ;
#21669 = AXIS2_PLACEMENT_3D ( 'NONE', #23408, #20221, #28060 ) ;
#21670 = CARTESIAN_POINT ( 'NONE',  ( 0.000000000000000000, 0.000000000000000000, 0.000000000000000000 ) ) ;
#21671 = LINE ( 'NONE', #44426, #40970 ) ;
#21672 = ORIENTED_EDGE ( 'NONE', *, *, #10431, .T. ) ;
#21673 = EDGE_CURVE ( 'NONE', #14404, #46520, #22004, .T. ) ;
#21674 = FACE_OUTER_BOUND ( 'NONE', #48009, .T. ) ;
#21675 = EDGE_CURVE ( 'NONE', #6884, #21962, #36928, .T. ) ;
#21676 = CARTESIAN_POINT ( 'NONE',  ( 13.83832728059186046, -142.6495187161941089, 5.500000000000000000 ) ) ;
#21677 = VERTEX_POINT ( 'NONE', #7325 ) ;
#21678 = CIRCLE ( 'NONE', #24033, 82.00000000000000000 ) ;
#21679 = EDGE_LOOP ( 'NONE', ( #857, #45954, #39666, #17116 ) ) ;
#21680 = CIRCLE ( 'NONE', #43559, 32.00000000000000000 ) ;
#21681 = LINE ( 'NONE', #13619, #45292 ) ;
#21682 = ORIENTED_EDGE ( 'NONE', *, *, #18676, .T. ) ;
#21683 = EDGE_CURVE ( 'NONE', #6694, #17845, #37431, .T. ) ;
#21684 = ORIENTED_EDGE ( 'NONE', *, *, #15873, .F. ) ;
#21685 = AXIS2_PLACEMENT_3D ( 'NONE', #37987, #18648, #38225 ) ;
#21686 = DIRECTION ( 'NONE',  ( -1.000000000000000000, 0.000000000000000000, 0.000000000000000000 ) ) ;
#21687 = FACE_OUTER_BOUND ( 'NONE', #8097, .T. ) ;
#21688 = CYLINDRICAL_SURFACE ( 'NONE', #26932, 77.49899999999999523 ) ;
#21689 = EDGE_LOOP ( 'NONE', ( #46912, #38966, #42775, #40657 ) ) ;
#21690 = CARTESIAN_POINT ( 'NONE',  ( 0.000000000000000000, 0.000000000000000000, 0.000000000000000000 ) ) ;
#21691 = ORIENTED_EDGE ( 'NONE', *, *, #25873, .F. ) ;
#21692 = VERTEX_POINT ( 'NONE', #29599 ) ;
#21693 = ORIENTED_EDGE ( 'NONE', *, *, #13169, .F. ) ;
#21694 = DIRECTION ( 'NONE',  ( 0.000000000000000000, 0.000000000000000000, 1.000000000000000000 ) ) ;
#21695 = CARTESIAN_POINT ( 'NONE',  ( 0.000000000000000000, 62.50329211542494789, -41.76937507738723099 ) ) ;
#21696 = VECTOR ( 'NONE', #26917, 1000.000000000000000 ) ;
#21697 = CARTESIAN_POINT ( 'NONE',  ( 0.000000000000000000, -33.17418723428294669, -17.67226234102862747 ) ) ;
#21698 = EDGE_CURVE ( 'NONE', #36999, #45459, #44530, .T. ) ;
#21699 = ORIENTED_EDGE ( 'NONE', *, *, #6468, .T. ) ;
#21700 = ORIENTED_EDGE ( 'NONE', *, *, #7233, .T. ) ;
#21701 = DIRECTION ( 'NONE',  ( 0.000000000000000000, 0.000000000000000000, -1.000000000000000000 ) ) ;
#21702 = ORIENTED_EDGE ( 'NONE', *, *, #7428, .F. ) ;
#21703 = DIRECTION ( 'NONE',  ( 0.000000000000000000, 0.000000000000000000, 1.000000000000000000 ) ) ;
#21704 = ADVANCED_FACE ( 'NONE', ( #44770 ), #3899, .T. ) ;
#21705 = DIRECTION ( 'NONE',  ( 0.000000000000000000, 0.5224985647159500202, -0.8526401643540916231 ) ) ;
#21706 = FACE_BOUND ( 'NONE', #14315, .T. ) ;
#21707 = DIRECTION ( 'NONE',  ( -0.000000000000000000, -0.9135454576426058626, -0.4067366430757889395 ) ) ;
#21708 = DIRECTION ( 'NONE',  ( -1.000000000000000000, 0.000000000000000000, -0.000000000000000000 ) ) ;
#21709 = EDGE_CURVE ( 'NONE', #39901, #5700, #14310, .T. ) ;
#21710 = DIRECTION ( 'NONE',  ( -1.000000000000000000, -0.000000000000000000, -0.000000000000000000 ) ) ;
#21711 = CARTESIAN_POINT ( 'NONE',  ( 0.000000000000000000, -8.830959090342926032, 74.65491531819115778 ) ) ;
#21712 = CARTESIAN_POINT ( 'NONE',  ( 5.000000000000000000, 21.40280677340421889, -36.13751322684397138 ) ) ;
#21713 = VECTOR ( 'NONE', #40199, 1000.000000000000000 ) ;
#21714 = VERTEX_POINT ( 'NONE', #7579 ) ;
#21715 = LINE ( 'NONE', #36638, #17101 ) ;
#21716 = ORIENTED_EDGE ( 'NONE', *, *, #28295, .F. ) ;
#21717 = AXIS2_PLACEMENT_3D ( 'NONE', #26255, #33582, #11078 ) ;
#21718 = CARTESIAN_POINT ( 'NONE',  ( 11.99999999999999822, -16.65972982744876774, -80.28980883073775487 ) ) ;
#21719 = VERTEX_POINT ( 'NONE', #38660 ) ;
#21720 = DIRECTION ( 'NONE',  ( -1.000000000000000000, 0.000000000000000000, 0.000000000000000000 ) ) ;
#21721 = CARTESIAN_POINT ( 'NONE',  ( 11.99999999999999822, 36.73666225445894185, 65.58780272294090707 ) ) ;
#21722 = EDGE_CURVE ( 'NONE', #14957, #32083, #23963, .T. ) ;
#21723 = EDGE_CURVE ( 'NONE', #30126, #10449, #27894, .T. ) ;
#21724 = ADVANCED_FACE ( 'NONE', ( #5121 ), #5357, .T. ) ;
#21725 = CARTESIAN_POINT ( 'NONE',  ( 0.000000000000000000, -120.0000000000000000, 2.500000000000000000 ) ) ;
#21726 = DIRECTION ( 'NONE',  ( -1.000000000000000000, 0.000000000000000000, -0.000000000000000000 ) ) ;
#21727 = LINE ( 'NONE', #32514, #48179 ) ;
#21728 = LINE ( 'NONE', #10721, #44880 ) ;
#21729 = EDGE_LOOP ( 'NONE', ( #36347, #23486, #2726, #48341 ) ) ;
#21730 = CARTESIAN_POINT ( 'NONE',  ( 11.99999999999999822, -16.65972982744991171, 80.28980883073751329 ) ) ;
#21731 = PLANE ( 'NONE',  #40167 ) ;
#21732 = ORIENTED_EDGE ( 'NONE', *, *, #30655, .T. ) ;
#21733 = VERTEX_POINT ( 'NONE', #38898 ) ;
#21734 = AXIS2_PLACEMENT_3D ( 'NONE', #27162, #30833, #33755 ) ;
#21735 = EDGE_LOOP ( 'NONE', ( #18052, #13190, #44342, #5882 ) ) ;
#21736 = DIRECTION ( 'NONE',  ( 0.000000000000000000, 0.000000000000000000, 1.000000000000000000 ) ) ;
#21737 = DIRECTION ( 'NONE',  ( -1.000000000000000000, -0.000000000000000000, -0.000000000000000000 ) ) ;
#21738 = ORIENTED_EDGE ( 'NONE', *, *, #32443, .F. ) ;
#21739 = DIRECTION ( 'NONE',  ( 0.000000000000000000, 0.000000000000000000, 1.000000000000000000 ) ) ;
#21740 = ORIENTED_EDGE ( 'NONE', *, *, #15216, .F. ) ;
#21741 = AXIS2_PLACEMENT_3D ( 'NONE', #36614, #47866, #20972 ) ;
#21742 = EDGE_CURVE ( 'NONE', #37732, #13922, #20272, .T. ) ;
#21743 = LINE ( 'NONE', #5879, #29781 ) ;
#21744 = EDGE_CURVE ( 'NONE', #10422, #13639, #15639, .T. ) ;
#21745 = EDGE_LOOP ( 'NONE', ( #10999, #7362, #34962, #12416 ) ) ;
#21746 = CARTESIAN_POINT ( 'NONE',  ( 10.00000000000000000, -80.28980883073768382, 16.65972982744906972 ) ) ;
#21747 = EDGE_LOOP ( 'NONE', ( #11429, #31544, #34212, #36276 ) ) ;
#21748 = CARTESIAN_POINT ( 'NONE',  ( 10.00000000000000000, -37.16516213103280108, 4.992566952384862589 ) ) ;
#21749 = ADVANCED_FACE ( 'NONE', ( #35201 ), #31556, .T. ) ;
#21750 = DIRECTION ( 'NONE',  ( 0.000000000000000000, 0.000000000000000000, 1.000000000000000000 ) ) ;
#21751 = COLOUR_RGB ( '', 0.09019608, 0.27058824, 0.51372549) ;
#21752 = LINE ( 'NONE', #32762, #16613 ) ;
#21753 = EDGE_CURVE ( 'NONE', #37621, #21091, #47906, .T. ) ;
#21754 = VERTEX_POINT ( 'NONE', #8767 ) ;
#21755 = ORIENTED_EDGE ( 'NONE', *, *, #28786, .F. ) ;
#21756 = VECTOR ( 'NONE', #26986, 1000.000000000000000 ) ;
#21757 = CARTESIAN_POINT ( 'NONE',  ( 10.00000000000000000, 0.000000000000000000, 0.000000000000000000 ) ) ;
#21758 = DIRECTION ( 'NONE',  ( -1.000000000000000000, -0.000000000000000000, 0.000000000000000000 ) ) ;
#21759 = EDGE_LOOP ( 'NONE', ( #19299, #2563, #39212, #44384 ) ) ;
#21760 = EDGE_LOOP ( 'NONE', ( #42993, #7309, #31592, #34603 ) ) ;
#21761 = PLANE ( 'NONE',  #25205 ) ;
#21762 = CARTESIAN_POINT ( 'NONE',  ( 0.000000000000000000, 24.73286445877704764, 73.44644590900067271 ) ) ;
#21763 = EDGE_LOOP ( 'NONE', ( #6164, #26287, #28132, #5932 ) ) ;
#21764 = VERTEX_POINT ( 'NONE', #34963 ) ;
#21765 = DIRECTION ( 'NONE',  ( 1.000000000000000000, -0.000000000000000000, -0.000000000000000000 ) ) ;
#21766 = DIRECTION ( 'NONE',  ( 0.000000000000000000, 0.000000000000000000, 1.000000000000000000 ) ) ;
#21767 = DIRECTION ( 'NONE',  ( 0.000000000000000000, -1.000000000000000000, -1.040834085586084730E-14 ) ) ;
#21768 = CARTESIAN_POINT ( 'NONE',  ( -3.000000000000000000, 16.61724383029390140, -20.69703378468903665 ) ) ;
#21769 = DIRECTION ( 'NONE',  ( -1.000000000000000000, 0.000000000000000000, 0.000000000000000000 ) ) ;
#21770 = EDGE_CURVE ( 'NONE', #15509, #7240, #26907, .T. ) ;
#21771 = EDGE_CURVE ( 'NONE', #23939, #2410, #11202, .T. ) ;
#21772 = CARTESIAN_POINT ( 'NONE',  ( 10.00000000000000000, -70.52718814184277107, 26.02418014898285037 ) ) ;
#21773 = PLANE ( 'NONE',  #3606 ) ;
#21774 = CARTESIAN_POINT ( 'NONE',  ( 10.00000000000000000, 0.000000000000000000, 0.000000000000000000 ) ) ;
#21775 = VECTOR ( 'NONE', #20981, 1000.000000000000000 ) ;
#21776 = CARTESIAN_POINT ( 'NONE',  ( -10.00000000000000000, 0.000000000000000000, 0.000000000000000000 ) ) ;
#21777 = AXIS2_PLACEMENT_3D ( 'NONE', #33458, #7263, #13896 ) ;
#21778 = CARTESIAN_POINT ( 'NONE',  ( 10.00000000000000000, 0.6853352020790449695, 37.58145647212454321 ) ) ;
#21779 = PRODUCT_RELATED_PRODUCT_CATEGORY ( 'part', '', ( #46831 ) ) ;
#21780 = DIRECTION ( 'NONE',  ( 0.000000000000000000, 0.1564344650402312020, -0.9876883405951376593 ) ) ;
#21781 = CARTESIAN_POINT ( 'NONE',  ( 0.000000000000000000, 24.73286445877808148, -73.44644590900034586 ) ) ;
#21782 = ORIENTED_EDGE ( 'NONE', *, *, #33765, .T. ) ;
#21783 = VERTEX_POINT ( 'NONE', #16141 ) ;
#21784 = EDGE_CURVE ( 'NONE', #23562, #44578, #41671, .T. ) ;
#21785 = ORIENTED_EDGE ( 'NONE', *, *, #2808, .T. ) ;
#21786 = PRODUCT_DEFINITION_CONTEXT ( 'detailed design', #17570, 'design' ) ;
#21787 = PLANE ( 'NONE',  #5736 ) ;
#21788 = DIRECTION ( 'NONE',  ( -1.000000000000000000, 0.000000000000000000, 0.000000000000000000 ) ) ;
#21789 = ORIENTED_EDGE ( 'NONE', *, *, #4651, .F. ) ;
#21790 = PRESENTATION_LAYER_ASSIGNMENT (  '', '', ( #39811 ) ) ;
#21791 = FACE_OUTER_BOUND ( 'NONE', #36959, .T. ) ;
#21792 = EDGE_LOOP ( 'NONE', ( #46908, #8276, #42014, #40115 ) ) ;
#21793 = LINE ( 'NONE', #48231, #35450 ) ;
#21794 = ORIENTED_EDGE ( 'NONE', *, *, #11620, .F. ) ;
#21795 = VERTEX_POINT ( 'NONE', #42078 ) ;
#21796 =( LENGTH_UNIT ( ) NAMED_UNIT ( * ) SI_UNIT ( .MILLI., .METRE. ) );
#21797 = CARTESIAN_POINT ( 'NONE',  ( 0.000000000000000000, 5.256550761633969060, -77.32052557432835727 ) ) ;
#21798 = CIRCLE ( 'NONE', #29632, 31.99999999999998934 ) ;
#21799 = CARTESIAN_POINT ( 'NONE',  ( 0.000000000000000000, 10.74501242461333028, -35.92658777277499382 ) ) ;
#21800 = ORIENTED_EDGE ( 'NONE', *, *, #33361, .F. ) ;
#21801 = DIRECTION ( 'NONE',  ( 0.000000000000000000, 0.000000000000000000, 1.000000000000000000 ) ) ;
#21802 = ORIENTED_EDGE ( 'NONE', *, *, #3795, .T. ) ;
#21804 = EDGE_CURVE ( 'NONE', #14555, #34506, #16647, .T. ) ;
#21803 = AXIS2_PLACEMENT_3D ( 'NONE', #31036, #1151, #46186 ) ;
#21805 = DIRECTION ( 'NONE',  ( -1.000000000000000000, -0.000000000000000000, 0.000000000000000000 ) ) ;
#21806 = CIRCLE ( 'NONE', #5410, 77.49900000000002365 ) ;
#21807 = LINE ( 'NONE', #10079, #3247 ) ;
#21808 = EDGE_CURVE ( 'NONE', #28899, #7732, #42566, .T. ) ;
#21809 = VERTEX_POINT ( 'NONE', #39125 ) ;
#21810 = LINE ( 'NONE', #40911, #27622 ) ;
#21811 = LINE ( 'NONE', #31905, #5191 ) ;
#21813 = ORIENTED_EDGE ( 'NONE', *, *, #36015, .T. ) ;
#21812 = DIRECTION ( 'NONE',  ( -1.000000000000000000, -0.000000000000000000, -0.000000000000000000 ) ) ;
#21814 = FACE_OUTER_BOUND ( 'NONE', #7386, .T. ) ;
#21815 = ORIENTED_EDGE ( 'NONE', *, *, #5306, .F. ) ;
#21816 = DIRECTION ( 'NONE',  ( 0.000000000000000000, 0.000000000000000000, -1.000000000000000000 ) ) ;
#21817 = EDGE_LOOP ( 'NONE', ( #31909, #48364, #12153, #14606 ) ) ;
#21818 = ORIENTED_EDGE ( 'NONE', *, *, #46257, .T. ) ;
#21819 = EDGE_CURVE ( 'NONE', #42231, #45900, #26044, .T. ) ;
#21820 = DIRECTION ( 'NONE',  ( 0.000000000000000000, 0.9510565162951544194, -0.3090169943749447867 ) ) ;
#21821 = LINE ( 'NONE', #29423, #31673 ) ;
#21822 = DIRECTION ( 'NONE',  ( -0.000000000000000000, -0.000000000000000000, -1.000000000000000000 ) ) ;
#21823 = FACE_OUTER_BOUND ( 'NONE', #36031, .T. ) ;
#21824 = PLANE ( 'NONE',  #14937 ) ;
#21825 = ORIENTED_EDGE ( 'NONE', *, *, #10779, .F. ) ;
#21826 = CARTESIAN_POINT ( 'NONE',  ( -6.880223345695647197, -142.5202692415819854, 5.500000000000000000 ) ) ;
#21827 = CARTESIAN_POINT ( 'NONE',  ( 11.59999999999999787, 1.420590287010929336E-15, 53.20000000000001705 ) ) ;
#21828 = EDGE_CURVE ( 'NONE', #26808, #10918, #39325, .T. ) ;
#21829 =( GEOMETRIC_REPRESENTATION_CONTEXT ( 3 ) GLOBAL_UNCERTAINTY_ASSIGNED_CONTEXT ( ( #19318 ) ) GLOBAL_UNIT_ASSIGNED_CONTEXT ( ( #29558, #9988, #3112 ) ) REPRESENTATION_CONTEXT ( 'NONE', 'WORKASPACE' ) );
#21830 = LINE ( 'NONE', #36754, #21578 ) ;
#21831 = VERTEX_POINT ( 'NONE', #45995 ) ;
#21832 = CARTESIAN_POINT ( 'NONE',  ( 5.000000000000000000, 38.55633173627010279, 16.65560815589424593 ) ) ;
#21833 = EDGE_CURVE ( 'NONE', #10918, #715, #15886, .T. ) ;
#21834 = CARTESIAN_POINT ( 'NONE',  ( 0.000000000000000000, 0.000000000000000000, 0.000000000000000000 ) ) ;
#21835 = CARTESIAN_POINT ( 'NONE',  ( 19.12409105625795291, -101.5943176906707919, 2.500000000000000000 ) ) ;
#21836 = DIRECTION ( 'NONE',  ( -0.000000000000000000, 0.8660254037844368202, 0.5000000000000031086 ) ) ;
#21837 = DIRECTION ( 'NONE',  ( 0.000000000000000000, -0.9510565162951502005, -0.3090169943749581094 ) ) ;
#21838 = CARTESIAN_POINT ( 'NONE',  ( -0.4301293587032979371, -118.5629931333561871, -2.500000000000000000 ) ) ;
#21839 = CARTESIAN_POINT ( 'NONE',  ( 10.00000000000000000, 81.50828551894225882, 8.966570791700975818 ) ) ;
#21840 = CARTESIAN_POINT ( 'NONE',  ( -10.00000000000000000, 0.000000000000000000, 0.000000000000000000 ) ) ;
#21841 = EDGE_CURVE ( 'NONE', #2889, #29380, #20546, .T. ) ;
#21842 = ORIENTED_EDGE ( 'NONE', *, *, #36070, .T. ) ;
#21843 = AXIS2_PLACEMENT_3D ( 'NONE', #10592, #6432, #25982 ) ;
#21844 = DIRECTION ( 'NONE',  ( 1.000000000000000000, 0.000000000000000000, 0.000000000000000000 ) ) ;
#21845 = VECTOR ( 'NONE', #30724, 1000.000000000000000 ) ;
#21846 = ORIENTED_EDGE ( 'NONE', *, *, #43552, .F. ) ;
#21847 = CARTESIAN_POINT ( 'NONE',  ( 10.00000000000000000, -36.88895765772628010, -6.736453364083947015 ) ) ;
#21848 = AXIS2_PLACEMENT_3D ( 'NONE', #38068, #48108, #25819 ) ;
#21849 = DIRECTION ( 'NONE',  ( 0.000000000000000000, 0.9510565162951539753, -0.3090169943749460635 ) ) ;
#21850 = ORIENTED_EDGE ( 'NONE', *, *, #33255, .F. ) ;
#21851 = AXIS2_PLACEMENT_3D ( 'NONE', #8874, #15506, #33849 ) ;
#21852 = DIRECTION ( 'NONE',  ( 0.000000000000000000, 0.000000000000000000, 1.000000000000000000 ) ) ;
#21853 = ORIENTED_EDGE ( 'NONE', *, *, #8780, .T. ) ;
#21854 = ORIENTED_EDGE ( 'NONE', *, *, #47848, .F. ) ;
#21855 = CARTESIAN_POINT ( 'NONE',  ( 0.000000000000000000, 14.67089635893819377, -73.72996012237423713 ) ) ;
#21856 = VERTEX_POINT ( 'NONE', #4623 ) ;
#21857 = EDGE_CURVE ( 'NONE', #31210, #46446, #17397, .T. ) ;
#21858 = FACE_OUTER_BOUND ( 'NONE', #42337, .T. ) ;
#21859 = LINE ( 'NONE', #11097, #26974 ) ;
#21860 = VERTEX_POINT ( 'NONE', #24909 ) ;
#21861 = ADVANCED_FACE ( 'NONE', ( #43752 ), #10466, .T. ) ;
#21862 = FACE_OUTER_BOUND ( 'NONE', #48189, .T. ) ;
#21863 = VERTEX_POINT ( 'NONE', #39851 ) ;
#21864 = EDGE_CURVE ( 'NONE', #36432, #44023, #40343, .T. ) ;
#21865 = DIRECTION ( 'NONE',  ( -1.000000000000000000, 0.000000000000000000, 0.000000000000000000 ) ) ;
#21866 = CARTESIAN_POINT ( 'NONE',  ( 10.00000000000000000, -30.80686688396994910, -21.53537804866113703 ) ) ;
#21867 = CARTESIAN_POINT ( 'NONE',  ( 0.000000000000000000, -81.34940948281344220, 10.30890764327355846 ) ) ;
#21868 = EDGE_CURVE ( 'NONE', #27438, #14436, #32276, .T. ) ;
#21869 = VECTOR ( 'NONE', #26179, 1000.000000000000114 ) ;
#21870 = DIRECTION ( 'NONE',  ( 0.000000000000000000, -1.000000000000000000, -1.040834085586084257E-14 ) ) ;
#21871 = ORIENTED_EDGE ( 'NONE', *, *, #46743, .F. ) ;
#21872 = ADVANCED_FACE ( 'NONE', ( #32729 ), #40088, .T. ) ;
#21873 = AXIS2_PLACEMENT_3D ( 'NONE', #37582, #4053, #18959 ) ;
#21874 = LINE ( 'NONE', #36566, #2901 ) ;
#21875 = ORIENTED_EDGE ( 'NONE', *, *, #27242, .T. ) ;
#21876 = EDGE_LOOP ( 'NONE', ( #36265, #24889, #2953, #5821 ) ) ;
#21877 = EDGE_CURVE ( 'NONE', #34997, #30063, #18967, .T. ) ;
#21878 = CARTESIAN_POINT ( 'NONE',  ( -3.000000000000000000, -3.948201729842038432, -23.21447184625298021 ) ) ;
#21879 = AXIS2_PLACEMENT_3D ( 'NONE', #20058, #39392, #34987 ) ;
#21880 = CARTESIAN_POINT ( 'NONE',  ( 0.000000000000000000, 0.000000000000000000, 0.000000000000000000 ) ) ;
#21881 = CARTESIAN_POINT ( 'NONE',  ( 11.99999999999999822, -56.15606465355001120, 59.75363087400055662 ) ) ;
#21882 = DIRECTION ( 'NONE',  ( -1.000000000000000000, 0.000000000000000000, 0.000000000000000000 ) ) ;
#21883 = ORIENTED_EDGE ( 'NONE', *, *, #21114, .F. ) ;
#21884 = DIRECTION ( 'NONE',  ( 1.000000000000000000, -0.000000000000000000, 0.000000000000000000 ) ) ;
#21885 = DIRECTION ( 'NONE',  ( -1.000000000000000000, 0.000000000000000000, 0.000000000000000000 ) ) ;
#21886 = CARTESIAN_POINT ( 'NONE',  ( 14.59956846177685996, -138.4757300459248484, -5.500000000000000000 ) ) ;
#21887 = DIRECTION ( 'NONE',  ( -1.000000000000000000, 0.000000000000000000, 0.000000000000000000 ) ) ;
#21888 = CARTESIAN_POINT ( 'NONE',  ( -3.000000000000000000, -0.9646360437375307573, 23.52805723605590060 ) ) ;
#21889 = ORIENTED_EDGE ( 'NONE', *, *, #2472, .F. ) ;
#21890 = CIRCLE ( 'NONE', #7814, 82.00000000000000000 ) ;
#21891 = CARTESIAN_POINT ( 'NONE',  ( 10.00000000000000000, 0.000000000000000000, 0.000000000000000000 ) ) ;
#21892 = DIRECTION ( 'NONE',  ( -1.000000000000000000, 0.000000000000000000, 0.000000000000000000 ) ) ;
#21893 = CARTESIAN_POINT ( 'NONE',  ( 11.59999999999999964, -0.8299999999999999600, -1.199999999999999956 ) ) ;
#21894 = CARTESIAN_POINT ( 'NONE',  ( 0.000000000000000000, -76.41127070299280888, 12.93880638057289012 ) ) ;
#21895 = ADVANCED_FACE ( 'NONE', ( #9494 ), #6087, .T. ) ;
#21896 = LINE ( 'NONE', #10164, #48251 ) ;
#21897 = CARTESIAN_POINT ( 'NONE',  ( 0.000000000000000000, 31.52238457039637609, -27.75498641678709788 ) ) ;
#21898 = VERTEX_POINT ( 'NONE', #43279 ) ;
#21899 = LINE ( 'NONE', #37328, #10541 ) ;
#21900 = EDGE_CURVE ( 'NONE', #31943, #20870, #21482, .T. ) ;
#21901 = DIRECTION ( 'NONE',  ( 0.000000000000000000, 0.000000000000000000, -1.000000000000000000 ) ) ;
#21902 = ORIENTED_EDGE ( 'NONE', *, *, #44357, .T. ) ;
#21903 = ORIENTED_EDGE ( 'NONE', *, *, #3643, .T. ) ;
#21904 = CIRCLE ( 'NONE', #43778, 77.49900000000000944 ) ;
#21905 = EDGE_CURVE ( 'NONE', #39461, #5144, #33831, .T. ) ;
#21906 = AXIS2_PLACEMENT_3D ( 'NONE', #26878, #38133, #23199 ) ;
#21907 = CIRCLE ( 'NONE', #28177, 82.00000000000000000 ) ;
#21908 = DIRECTION ( 'NONE',  ( -1.000000000000000000, 0.000000000000000000, 0.000000000000000000 ) ) ;
#21909 = ORIENTED_EDGE ( 'NONE', *, *, #3603, .T. ) ;
#21910 = VECTOR ( 'NONE', #13502, 1000.000000000000000 ) ;
#21911 = AXIS2_PLACEMENT_3D ( 'NONE', #14980, #4206, #30397 ) ;
#21912 = ORIENTED_EDGE ( 'NONE', *, *, #46447, .T. ) ;
#21913 = CARTESIAN_POINT ( 'NONE',  ( 6.000000000000000000, 15.33399622253601002, -80.55351364060572905 ) ) ;
#21915 = VERTEX_POINT ( 'NONE', #6319 ) ;
#21914 = AXIS2_PLACEMENT_3D ( 'NONE', #31113, #1246, #261 ) ;
#21916 = EDGE_CURVE ( 'NONE', #12855, #23067, #2873, .T. ) ;
#21917 = DIRECTION ( 'NONE',  ( -1.000000000000000000, -0.000000000000000000, 0.000000000000000000 ) ) ;
#21918 = LINE ( 'NONE', #10684, #36317 ) ;
#21919 = ORIENTED_EDGE ( 'NONE', *, *, #28838, .T. ) ;
#21920 = CYLINDRICAL_SURFACE ( 'NONE', #31303, 42.00000000000000000 ) ;
#21921 = ORIENTED_EDGE ( 'NONE', *, *, #43049, .F. ) ;
#21922 = EDGE_CURVE ( 'NONE', #5918, #14629, #1936, .T. ) ;
#21923 = ORIENTED_EDGE ( 'NONE', *, *, #14697, .F. ) ;
#21924 = ORIENTED_EDGE ( 'NONE', *, *, #9077, .F. ) ;
#21925 = ORIENTED_EDGE ( 'NONE', *, *, #4528, .F. ) ;
#21926 = CARTESIAN_POINT ( 'NONE',  ( 10.00000000000000000, 0.000000000000000000, 0.000000000000000000 ) ) ;
#21928 = EDGE_LOOP ( 'NONE', ( #27072, #14834, #25476, #1331 ) ) ;
#21927 = DIRECTION ( 'NONE',  ( 0.000000000000000000, 1.000000000000000000, 0.000000000000000000 ) ) ;
#21929 = DIRECTION ( 'NONE',  ( 1.000000000000000000, -0.000000000000000000, -0.000000000000000000 ) ) ;
#21930 = ORIENTED_EDGE ( 'NONE', *, *, #45885, .F. ) ;
#21931 = ORIENTED_EDGE ( 'NONE', *, *, #27304, .T. ) ;
#21932 = ORIENTED_EDGE ( 'NONE', *, *, #32175, .F. ) ;
#21933 = FACE_OUTER_BOUND ( 'NONE', #14731, .T. ) ;
#21934 = ORIENTED_EDGE ( 'NONE', *, *, #2694, .T. ) ;
#21935 = EDGE_CURVE ( 'NONE', #46202, #26395, #32034, .T. ) ;
#21936 = CARTESIAN_POINT ( 'NONE',  ( 24.95699195200416654, -110.9640411295978595, -5.500000000000000000 ) ) ;
#21937 = CARTESIAN_POINT ( 'NONE',  ( 15.00000000000000000, -22.32062822937469093, 14.36278369418830181 ) ) ;
#21938 = ADVANCED_FACE ( 'NONE', ( #6553 ), #16859, .T. ) ;
#21939 = FACE_BOUND ( 'NONE', #40366, .T. ) ;
#21940 = CARTESIAN_POINT ( 'NONE',  ( 0.000000000000000000, 0.000000000000000000, 0.000000000000000000 ) ) ;
#21941 = DIRECTION ( 'NONE',  ( -0.000000000000000000, -0.000000000000000000, -1.000000000000000000 ) ) ;
#21942 = DIRECTION ( 'NONE',  ( -1.000000000000000000, -0.000000000000000000, -0.000000000000000000 ) ) ;
#21943 = CARTESIAN_POINT ( 'NONE',  ( 3.429551818649054340, -146.3199197248623875, -5.500000000000000000 ) ) ;
#21944 = CIRCLE ( 'NONE', #39920, 31.99999999999999289 ) ;
#21945 = CARTESIAN_POINT ( 'NONE',  ( 18.80329974962065265, -105.8248132807389084, 2.500000000000000000 ) ) ;
#21946 = ORIENTED_EDGE ( 'NONE', *, *, #45424, .T. ) ;
#21947 = VECTOR ( 'NONE', #37404, 1000.000000000000000 ) ;
#21948 = DIRECTION ( 'NONE',  ( -1.000000000000000000, 0.000000000000000000, 0.000000000000000000 ) ) ;
#21949 = AXIS2_PLACEMENT_3D ( 'NONE', #43153, #9599, #38269 ) ;
#21950 = CIRCLE ( 'NONE', #16477, 11.59999999999999787 ) ;
#21951 = CARTESIAN_POINT ( 'NONE',  ( 10.00000000000000000, 72.35160999960844208, -20.41045688087747223 ) ) ;
#21952 = CARTESIAN_POINT ( 'NONE',  ( 5.999999999999999112, 56.15606465355041621, -59.75363087400017292 ) ) ;
#21953 = CARTESIAN_POINT ( 'NONE',  ( 10.00000000000000000, 31.46837873494978055, 68.27212725128286763 ) ) ;
#21954 = AXIS2_PLACEMENT_3D ( 'NONE', #35008, #46273, #27934 ) ;
#21955 = DIRECTION ( 'NONE',  ( 0.000000000000000000, 0.000000000000000000, 1.000000000000000000 ) ) ;
#21956 = AXIS2_PLACEMENT_3D ( 'NONE', #20819, #32557, #25190 ) ;
#21957 = CARTESIAN_POINT ( 'NONE',  ( 0.000000000000000000, -39.78640506895559525, -66.50666863322042843 ) ) ;
#21958 = DIRECTION ( 'NONE',  ( -1.000000000000000000, -0.000000000000000000, 0.000000000000000000 ) ) ;
#21959 = CARTESIAN_POINT ( 'NONE',  ( -18.12185313557660038, -104.9634299478706794, 5.500000000000000000 ) ) ;
#21960 = DIRECTION ( 'NONE',  ( 1.000000000000000000, 0.000000000000000000, 0.000000000000000000 ) ) ;
#21961 = CARTESIAN_POINT ( 'NONE',  ( 10.00000000000000000, 0.000000000000000000, 0.000000000000000000 ) ) ;
#21962 = VERTEX_POINT ( 'NONE', #47650 ) ;
#21963 = ORIENTED_EDGE ( 'NONE', *, *, #8245, .T. ) ;
#21964 = ORIENTED_EDGE ( 'NONE', *, *, #9135, .F. ) ;
#21965 = EDGE_CURVE ( 'NONE', #44445, #26225, #28823, .T. ) ;
#21966 = FACE_OUTER_BOUND ( 'NONE', #6642, .T. ) ;
#21967 = CARTESIAN_POINT ( 'NONE',  ( 0.000000000000000000, 74.65491531819118620, 23.16904090965732621 ) ) ;
#21968 = ORIENTED_EDGE ( 'NONE', *, *, #22761, .F. ) ;
#21969 = VERTEX_POINT ( 'NONE', #39369 ) ;
#21970 = AXIS2_PLACEMENT_3D ( 'NONE', #15697, #4457, #8826 ) ;
#21971 = CIRCLE ( 'NONE', #14969, 15.99999999999999645 ) ;
#21972 = DIRECTION ( 'NONE',  ( 0.000000000000000000, -0.7604059656000227152, -0.6494480483301934282 ) ) ;
#21973 = VECTOR ( 'NONE', #37844, 1000.000000000000000 ) ;
#21974 = AXIS2_PLACEMENT_3D ( 'NONE', #2362, #35672, #32012 ) ;
#21975 = VERTEX_POINT ( 'NONE', #20766 ) ;
#21976 = VERTEX_POINT ( 'NONE', #10218 ) ;
#21977 = EDGE_CURVE ( 'NONE', #33061, #41296, #22893, .T. ) ;
#21978 = CIRCLE ( 'NONE', #9480, 31.99999999999998579 ) ;
#21979 = ADVANCED_FACE ( 'NONE', ( #13664 ), #28597, .F. ) ;
#21980 = ADVANCED_FACE ( 'NONE', ( #13901 ), #11676, .F. ) ;
#21981 = CARTESIAN_POINT ( 'NONE',  ( 0.000000000000000000, -2.663952781846440576, 41.91543099594817789 ) ) ;
#21982 = CYLINDRICAL_SURFACE ( 'NONE', #35661, 77.49899999999999523 ) ;
#21983 = EDGE_LOOP ( 'NONE', ( #18442, #381, #5338, #32879 ) ) ;
#21984 = EDGE_CURVE ( 'NONE', #39718, #13449, #36172, .T. ) ;
#21985 = DIRECTION ( 'NONE',  ( -0.000000000000000000, -0.000000000000000000, 1.000000000000000000 ) ) ;
#21986 = CIRCLE ( 'NONE', #17308, 1.000000000000000000 ) ;
#21987 = EDGE_CURVE ( 'NONE', #1423, #13574, #44967, .T. ) ;
#21988 = CARTESIAN_POINT ( 'NONE',  ( 0.000000000000000000, 0.000000000000000000, 0.000000000000000000 ) ) ;
#21989 = CARTESIAN_POINT ( 'NONE',  ( 0.000000000000000000, 71.21200624218795383, 40.65526001592638039 ) ) ;
#21990 = ORIENTED_EDGE ( 'NONE', *, *, #11593, .F. ) ;
#21991 = ORIENTED_EDGE ( 'NONE', *, *, #40514, .T. ) ;
#21992 = CARTESIAN_POINT ( 'NONE',  ( -22.67106064244953245, -113.6342314410295842, 5.500000000000000000 ) ) ;
#21993 = CARTESIAN_POINT ( 'NONE',  ( 10.00000000000000000, 30.41916302227113178, 71.27951684758036777 ) ) ;
#21994 = ORIENTED_EDGE ( 'NONE', *, *, #23644, .F. ) ;
#21995 = ORIENTED_EDGE ( 'NONE', *, *, #24897, .T. ) ;
#21996 = LINE ( 'NONE', #36920, #27576 ) ;
#21997 = DIRECTION ( 'NONE',  ( 0.000000000000000000, 0.000000000000000000, 1.000000000000000000 ) ) ;
#21998 = ORIENTED_EDGE ( 'NONE', *, *, #38925, .F. ) ;
#21999 = VERTEX_POINT ( 'NONE', #33223 ) ;
#22001 = EDGE_CURVE ( 'NONE', #13122, #46849, #22457, .T. ) ;
#22000 = DIRECTION ( 'NONE',  ( 0.000000000000000000, 0.000000000000000000, 1.000000000000000000 ) ) ;
#22002 = DIRECTION ( 'NONE',  ( 0.000000000000000000, 0.000000000000000000, 1.000000000000000000 ) ) ;
#22003 = DIRECTION ( 'NONE',  ( -1.000000000000000000, 0.000000000000000000, -0.000000000000000000 ) ) ;
#22004 = LINE ( 'NONE', #37670, #37710 ) ;
#22005 = LINE ( 'NONE', #33022, #7029 ) ;
#22006 = EDGE_CURVE ( 'NONE', #42551, #21081, #44004, .T. ) ;
#22008 = AXIS2_PLACEMENT_3D ( 'NONE', #32970, #44242, #29548 ) ;
#22007 = DIRECTION ( 'NONE',  ( 0.000000000000000000, 0.000000000000000000, 1.000000000000000000 ) ) ;
#22009 = CIRCLE ( 'NONE', #40782, 31.99999999999999289 ) ;
#22010 = CARTESIAN_POINT ( 'NONE',  ( 11.99999999999999822, 39.47590169984944453, -71.87247863392373404 ) ) ;
#22011 = DIRECTION ( 'NONE',  ( 1.000000000000000000, -0.000000000000000000, 0.000000000000000000 ) ) ;
#22012 = ORIENTED_EDGE ( 'NONE', *, *, #24530, .F. ) ;
#22013 = CIRCLE ( 'NONE', #29043, 31.99999999999998934 ) ;
#22014 = DIRECTION ( 'NONE',  ( 0.000000000000000000, -0.6494480483301739993, -0.7604059656000390355 ) ) ;
#22015 = LINE ( 'NONE', #44301, #23009 ) ;
#22016 = SURFACE_SIDE_STYLE ('',( #7090 ) ) ;
#22017 = DIRECTION ( 'NONE',  ( 0.000000000000000000, 0.000000000000000000, 1.000000000000000000 ) ) ;
#22018 = VECTOR ( 'NONE', #10457, 1000.000000000000000 ) ;
#22019 = ORIENTED_EDGE ( 'NONE', *, *, #13925, .F. ) ;
#22020 = ORIENTED_EDGE ( 'NONE', *, *, #20273, .T. ) ;
#22021 = EDGE_CURVE ( 'NONE', #15663, #28440, #11452, .T. ) ;
#22022 = CARTESIAN_POINT ( 'NONE',  ( 11.99999999999999822, 0.000000000000000000, 0.000000000000000000 ) ) ;
#22023 = VECTOR ( 'NONE', #27134, 1000.000000000000000 ) ;
#22024 = EDGE_CURVE ( 'NONE', #4021, #14629, #35402, .T. ) ;
#22025 = CARTESIAN_POINT ( 'NONE',  ( -10.00000000000000000, 0.000000000000000000, 0.000000000000000000 ) ) ;
#22026 = EDGE_CURVE ( 'NONE', #7117, #6056, #44031, .T. ) ;
#22027 = VERTEX_POINT ( 'NONE', #37617 ) ;
#22028 = DIRECTION ( 'NONE',  ( -1.000000000000000000, 0.000000000000000000, 0.000000000000000000 ) ) ;
#22029 = ORIENTED_EDGE ( 'NONE', *, *, #7050, .T. ) ;
#22030 = DIRECTION ( 'NONE',  ( -0.000000000000000000, -0.000000000000000000, -1.000000000000000000 ) ) ;
#22031 = ORIENTED_EDGE ( 'NONE', *, *, #47329, .T. ) ;
#22032 = ORIENTED_EDGE ( 'NONE', *, *, #38605, .F. ) ;
#22033 = VERTEX_POINT ( 'NONE', #4093 ) ;
#22034 = ORIENTED_EDGE ( 'NONE', *, *, #16147, .T. ) ;
#22035 = DIRECTION ( 'NONE',  ( 0.6064928550163531940, 0.7950889364178782559, 0.000000000000000000 ) ) ;
#22036 = EDGE_CURVE ( 'NONE', #30527, #2177, #10945, .T. ) ;
#22037 = EDGE_CURVE ( 'NONE', #13625, #14256, #27628, .T. ) ;
#22038 = CARTESIAN_POINT ( 'NONE',  ( 11.99999999999999822, 0.000000000000000000, 0.000000000000000000 ) ) ;
#22039 = EDGE_LOOP ( 'NONE', ( #22604, #33076, #38655, #15910 ) ) ;
#22040 = ORIENTED_EDGE ( 'NONE', *, *, #2174, .F. ) ;
#22041 = DIRECTION ( 'NONE',  ( -1.000000000000000000, 0.000000000000000000, 0.000000000000000000 ) ) ;
#22042 = AXIS2_PLACEMENT_3D ( 'NONE', #20545, #42350, #35490 ) ;
#22043 = ORIENTED_EDGE ( 'NONE', *, *, #20727, .T. ) ;
#22044 = DIRECTION ( 'NONE',  ( 0.000000000000000000, -0.9781476007338043566, 0.2079116908177651712 ) ) ;
#22045 = LINE ( 'NONE', #2727, #5613 ) ;
#22046 = ORIENTED_EDGE ( 'NONE', *, *, #28773, .T. ) ;
#22047 = CARTESIAN_POINT ( 'NONE',  ( 0.000000000000000000, 0.000000000000000000, 0.000000000000000000 ) ) ;
#22048 = DIRECTION ( 'NONE',  ( 0.000000000000000000, 0.000000000000000000, 1.000000000000000000 ) ) ;
#22049 = ORIENTED_EDGE ( 'NONE', *, *, #30080, .T. ) ;
#22050 = EDGE_CURVE ( 'NONE', #12709, #30788, #26367, .T. ) ;
#22051 = DIRECTION ( 'NONE',  ( 0.000000000000000000, 0.8910065241883657894, 0.4539904997395509678 ) ) ;
#22052 = CARTESIAN_POINT ( 'NONE',  ( 10.00000000000000000, -30.00120703465189465, -22.64427369931201639 ) ) ;
#22053 = ORIENTED_EDGE ( 'NONE', *, *, #43226, .F. ) ;
#22054 = DIRECTION ( 'NONE',  ( 1.000000000000000000, 0.000000000000000000, -0.000000000000000000 ) ) ;
#22055 = EDGE_LOOP ( 'NONE', ( #39119, #23194, #22889, #25546 ) ) ;
#22056 = VERTEX_POINT ( 'NONE', #18999 ) ;
#22057 = FACE_OUTER_BOUND ( 'NONE', #17746, .T. ) ;
#22058 = DIRECTION ( 'NONE',  ( -1.000000000000000000, 0.000000000000000000, 0.000000000000000000 ) ) ;
#22059 = ORIENTED_EDGE ( 'NONE', *, *, #8358, .T. ) ;
#22060 = AXIS2_PLACEMENT_3D ( 'NONE', #22935, #38117, #19483 ) ;
#22061 = CARTESIAN_POINT ( 'NONE',  ( -13.05994868825747446, -139.5943292883446532, -2.500000000000000000 ) ) ;
#22062 = FACE_OUTER_BOUND ( 'NONE', #7262, .T. ) ;
#22063 = LINE ( 'NONE', #26239, #8085 ) ;
#22064 = ORIENTED_EDGE ( 'NONE', *, *, #27637, .T. ) ;
#22065 = CIRCLE ( 'NONE', #45507, 16.00000000000000000 ) ;
#22066 = CARTESIAN_POINT ( 'NONE',  ( 0.000000000000000000, -37.16516213103280108, 4.992566952384862589 ) ) ;
#22067 = PLANE ( 'NONE',  #35263 ) ;
#22068 = DIRECTION ( 'NONE',  ( 1.000000000000000000, 0.000000000000000000, 0.000000000000000000 ) ) ;
#22069 = EDGE_LOOP ( 'NONE', ( #39990, #48425, #29774, #30488 ) ) ;
#22070 = DIRECTION ( 'NONE',  ( -1.000000000000000000, 0.000000000000000000, 0.000000000000000000 ) ) ;
#22071 = CARTESIAN_POINT ( 'NONE',  ( 11.99999999999999822, 0.000000000000000000, 0.000000000000000000 ) ) ;
#22072 = DIRECTION ( 'NONE',  ( 1.000000000000000000, 0.000000000000000000, 0.000000000000000000 ) ) ;
#22073 = FACE_OUTER_BOUND ( 'NONE', #21983, .T. ) ;
#22074 = VECTOR ( 'NONE', #23451, 1000.000000000000000 ) ;
#22075 = DIRECTION ( 'NONE',  ( 0.000000000000000000, 0.000000000000000000, 1.000000000000000000 ) ) ;
#22076 = DIRECTION ( 'NONE',  ( 0.000000000000000000, 0.000000000000000000, 1.000000000000000000 ) ) ;
#22077 = DIRECTION ( 'NONE',  ( -1.000000000000000000, 0.000000000000000000, 0.000000000000000000 ) ) ;
#22078 = CARTESIAN_POINT ( 'NONE',  ( 10.00000000000000000, 37.16516213103277977, 4.992566952385115719 ) ) ;
#22079 = EDGE_LOOP ( 'NONE', ( #35743, #17052, #31155, #1432 ) ) ;
#22080 = EDGE_CURVE ( 'NONE', #43252, #36432, #23705, .T. ) ;
#22081 = CIRCLE ( 'NONE', #36191, 19.21700905503013601 ) ;
#22082 = ORIENTED_EDGE ( 'NONE', *, *, #13036, .F. ) ;
#22083 = EDGE_CURVE ( 'NONE', #21044, #12855, #42466, .T. ) ;
#22084 = DIRECTION ( 'NONE',  ( -1.000000000000000000, -0.000000000000000000, -0.000000000000000000 ) ) ;
#22085 = ORIENTED_EDGE ( 'NONE', *, *, #19288, .F. ) ;
#22086 = DIRECTION ( 'NONE',  ( -1.000000000000000000, 0.000000000000000000, 0.000000000000000000 ) ) ;
#22087 = AXIS2_PLACEMENT_3D ( 'NONE', #15152, #41824, #29584 ) ;
#22088 = ADVANCED_FACE ( 'NONE', ( #32971 ), #22207, .T. ) ;
#22089 = DIRECTION ( 'NONE',  ( 0.7533909544171997208, 0.6575728627325956310, 0.000000000000000000 ) ) ;
#22090 = VERTEX_POINT ( 'NONE', #37132 ) ;
#22091 = CIRCLE ( 'NONE', #8042, 16.00000000000000000 ) ;
#22092 = DIRECTION ( 'NONE',  ( 0.000000000000000000, -1.000000000000000000, 0.000000000000000000 ) ) ;
#22093 = EDGE_CURVE ( 'NONE', #7802, #17130, #31557, .T. ) ;
#22094 = VECTOR ( 'NONE', #475, 1000.000000000000000 ) ;
#22095 = VERTEX_POINT ( 'NONE', #40564 ) ;
#22096 = VECTOR ( 'NONE', #11665, 1000.000000000000000 ) ;
#22097 = AXIS2_PLACEMENT_3D ( 'NONE', #33359, #10850, #18429 ) ;
#22098 = CARTESIAN_POINT ( 'NONE',  ( 0.000000000000000000, 26.02418014898407961, -70.52718814184231633 ) ) ;
#22099 = VERTEX_POINT ( 'NONE', #7026 ) ;
#22100 = ORIENTED_EDGE ( 'NONE', *, *, #31084, .F. ) ;
#22101 = EDGE_CURVE ( 'NONE', #34021, #29746, #38559, .T. ) ;
#22102 = EDGE_CURVE ( 'NONE', #21614, #22033, #36878, .T. ) ;
#22103 = CARTESIAN_POINT ( 'NONE',  ( 10.00000000000000000, -41.81611651403864727, 3.925862922256025289 ) ) ;
#22104 = EDGE_CURVE ( 'NONE', #13054, #33911, #10421, .T. ) ;
#22105 = CARTESIAN_POINT ( 'NONE',  ( 12.50000000000000000, -132.5000000000000000, 40.00000000000000000 ) ) ;
#22106 = CARTESIAN_POINT ( 'NONE',  ( 35.50000000000000711, -120.0000000000000000, 2.500000000000000000 ) ) ;
#22107 = ORIENTED_EDGE ( 'NONE', *, *, #35905, .T. ) ;
#22108 = DIRECTION ( 'NONE',  ( 0.000000000000000000, -0.1564344650402381687, 0.9876883405951365491 ) ) ;
#22109 = CIRCLE ( 'NONE', #195, 37.49900000000000233 ) ;
#22110 = ORIENTED_EDGE ( 'NONE', *, *, #32199, .F. ) ;
#22111 = CARTESIAN_POINT ( 'NONE',  ( 0.000000000000000000, -37.48860685352290290, -0.8828120875904512665 ) ) ;
#22112 = CARTESIAN_POINT ( 'NONE',  ( 0.000000000000000000, -17.80606268964563554, 33.00180498840040855 ) ) ;
#22113 = CARTESIAN_POINT ( 'NONE',  ( 5.000000000000000000, 15.48615015657581750, 39.04073710021349797 ) ) ;
#22114 = AXIS2_PLACEMENT_3D ( 'NONE', #8832, #23774, #41915 ) ;
#22115 = EDGE_CURVE ( 'NONE', #43390, #19329, #29958, .T. ) ;
#22116 = CARTESIAN_POINT ( 'NONE',  ( 10.00000000000000000, 16.45098606841173705, -33.79645857604496229 ) ) ;
#22117 = CIRCLE ( 'NONE', #4136, 31.99999999999998934 ) ;
#22118 = EDGE_LOOP ( 'NONE', ( #42477, #30553, #17168, #30578 ) ) ;
#22119 = CARTESIAN_POINT ( 'NONE',  ( 0.000000000000000000, -55.38113227695820484, 54.21277698773656084 ) ) ;
#22120 = ORIENTED_EDGE ( 'NONE', *, *, #3424, .T. ) ;
#22121 = ORIENTED_EDGE ( 'NONE', *, *, #19989, .T. ) ;
#22122 = CYLINDRICAL_SURFACE ( 'NONE', #8270, 16.00000000000000000 ) ;
#22123 = AXIS2_PLACEMENT_3D ( 'NONE', #8394, #45857, #4719 ) ;
#22124 = DIRECTION ( 'NONE',  ( -1.000000000000000000, 0.000000000000000000, 0.000000000000000000 ) ) ;
#22125 = DIRECTION ( 'NONE',  ( 0.000000000000000000, 0.000000000000000000, 1.000000000000000000 ) ) ;
#22126 = DIRECTION ( 'NONE',  ( -0.000000000000000000, -0.000000000000000000, -1.000000000000000000 ) ) ;
#22127 = VERTEX_POINT ( 'NONE', #31254 ) ;
#22128 = CARTESIAN_POINT ( 'NONE',  ( -21.33958957442910886, -129.9559990355020034, 2.500000000000000000 ) ) ;
#22129 = VECTOR ( 'NONE', #17312, 1000.000000000000000 ) ;
#22130 = CARTESIAN_POINT ( 'NONE',  ( 0.000000000000000000, 65.59268652807263322, -36.72794159290169347 ) ) ;
#22131 = CARTESIAN_POINT ( 'NONE',  ( 0.000000000000000000, -76.69515212746036070, 29.01471420065537643 ) ) ;
#22132 = DIRECTION ( 'NONE',  ( -1.000000000000000000, -0.000000000000000000, 0.000000000000000000 ) ) ;
#22133 = DIRECTION ( 'NONE',  ( 0.000000000000000000, 0.000000000000000000, 1.000000000000000000 ) ) ;
#22134 = AXIS2_PLACEMENT_3D ( 'NONE', #14067, #28988, #43925 ) ;
#22135 = CYLINDRICAL_SURFACE ( 'NONE', #2717, 31.99999999999998579 ) ;
#22136 = DIRECTION ( 'NONE',  ( -1.000000000000000000, 0.000000000000000000, 0.000000000000000000 ) ) ;
#22137 = CARTESIAN_POINT ( 'NONE',  ( 11.99999999999999822, -54.21277698773636899, -55.38113227695839669 ) ) ;
#22138 = AXIS2_PLACEMENT_3D ( 'NONE', #3008, #25041, #6449 ) ;
#22139 = CARTESIAN_POINT ( 'NONE',  ( 0.000000000000000000, 0.000000000000000000, 0.000000000000000000 ) ) ;
#22140 = DIRECTION ( 'NONE',  ( 0.000000000000000000, 0.000000000000000000, 1.000000000000000000 ) ) ;
#22141 = AXIS2_PLACEMENT_3D ( 'NONE', #36319, #36553, #21132 ) ;
#22142 = LINE ( 'NONE', #14079, #14546 ) ;
#22143 = CARTESIAN_POINT ( 'NONE',  ( 0.000000000000000000, -65.58780272294100655, 36.73666225445870737 ) ) ;
#22144 = LINE ( 'NONE', #2821, #33129 ) ;
#22145 = DIRECTION ( 'NONE',  ( -0.6516173805718079581, 0.7585478161175704948, 0.000000000000000000 ) ) ;
#22146 = CARTESIAN_POINT ( 'NONE',  ( -6.880223345695647197, -142.5202692415819854, 5.500000000000000000 ) ) ;
#22147 = EDGE_CURVE ( 'NONE', #23778, #47607, #11917, .T. ) ;
#22148 = CIRCLE ( 'NONE', #8064, 31.99999999999998934 ) ;
#22149 = EDGE_CURVE ( 'NONE', #9352, #7024, #23174, .T. ) ;
#22150 = CARTESIAN_POINT ( 'NONE',  ( 11.99999999999999822, -62.50329211542465657, 41.76937507738766442 ) ) ;
#22151 = EDGE_CURVE ( 'NONE', #20259, #28619, #31494, .T. ) ;
#22152 = VERTEX_POINT ( 'NONE', #20216 ) ;
#22153 = EDGE_CURVE ( 'NONE', #46727, #22767, #15828, .T. ) ;
#22154 = EDGE_CURVE ( 'NONE', #46674, #1488, #241, .T. ) ;
#22155 = ORIENTED_EDGE ( 'NONE', *, *, #29727, .F. ) ;
#22156 = AXIS2_PLACEMENT_3D ( 'NONE', #38576, #34892, #43205 ) ;
#22157 = AXIS2_PLACEMENT_3D ( 'NONE', #5833, #34948, #16355 ) ;
#22158 = CIRCLE ( 'NONE', #26071, 77.49900000000000944 ) ;
#22159 = CARTESIAN_POINT ( 'NONE',  ( 10.00000000000000000, 27.05870788708267582, -26.08949754952995903 ) ) ;
#22160 = ORIENTED_EDGE ( 'NONE', *, *, #23546, .T. ) ;
#22161 = AXIS2_PLACEMENT_3D ( 'NONE', #15109, #11192, #44717 ) ;
#22162 = EDGE_CURVE ( 'NONE', #46621, #7146, #21360, .T. ) ;
#22163 = CIRCLE ( 'NONE', #47938, 12.49999999999999645 ) ;
#22164 = AXIS2_PLACEMENT_3D ( 'NONE', #45621, #38785, #11857 ) ;
#22165 = DIRECTION ( 'NONE',  ( 0.000000000000000000, 0.5877852522924742473, -0.8090169943749465631 ) ) ;
#22166 = EDGE_CURVE ( 'NONE', #5585, #24462, #8477, .T. ) ;
#22167 = CIRCLE ( 'NONE', #44853, 20.69999999999999929 ) ;
#22168 = CARTESIAN_POINT ( 'NONE',  ( 11.99999999999999822, 0.000000000000000000, 0.000000000000000000 ) ) ;
#22169 = CIRCLE ( 'NONE', #39409, 16.00000000000000000 ) ;
#22171 = ORIENTED_EDGE ( 'NONE', *, *, #32053, .T. ) ;
#22170 = FACE_OUTER_BOUND ( 'NONE', #19969, .T. ) ;
#22172 = VERTEX_POINT ( 'NONE', #42250 ) ;
#22173 = CARTESIAN_POINT ( 'NONE',  ( 12.00000000000000000, 9.615535125379096826, 24.73947219025905042 ) ) ;
#22174 = VERTEX_POINT ( 'NONE', #27332 ) ;
#22175 = ORIENTED_EDGE ( 'NONE', *, *, #27187, .F. ) ;
#22176 = ORIENTED_EDGE ( 'NONE', *, *, #39810, .T. ) ;
#22177 = FACE_OUTER_BOUND ( 'NONE', #22238, .T. ) ;
#22178 = CARTESIAN_POINT ( 'NONE',  ( 0.000000000000000000, -77.32052557432837148, -5.256550761633681290 ) ) ;
#22179 = EDGE_CURVE ( 'NONE', #19681, #42002, #12177, .T. ) ;
#22180 = DIRECTION ( 'NONE',  ( -1.000000000000000000, -0.000000000000000000, -0.000000000000000000 ) ) ;
#22181 = ORIENTED_EDGE ( 'NONE', *, *, #41842, .T. ) ;
#22182 = ORIENTED_EDGE ( 'NONE', *, *, #5203, .T. ) ;
#22183 = LINE ( 'NONE', #3579, #31033 ) ;
#22184 = VERTEX_POINT ( 'NONE', #27826 ) ;
#22185 = DIRECTION ( 'NONE',  ( 0.000000000000000000, 1.224646799147347784E-16, 1.000000000000000000 ) ) ;
#22186 = CARTESIAN_POINT ( 'NONE',  ( 0.000000000000000000, 59.03342792756263435, 46.54456581323825048 ) ) ;
#22187 = DIRECTION ( 'NONE',  ( 1.000000000000000000, 0.000000000000000000, 0.000000000000000000 ) ) ;
#22188 = DIRECTION ( 'NONE',  ( 0.000000000000000000, 0.8090169943749445647, 0.5877852522924770229 ) ) ;
#22189 = DIRECTION ( 'NONE',  ( 0.000000000000000000, 0.5877852522924684742, 0.8090169943749506709 ) ) ;
#22190 = CARTESIAN_POINT ( 'NONE',  ( -22.67106064244953245, -113.6342314410295842, 2.500000000000000000 ) ) ;
#22191 = AXIS2_PLACEMENT_3D ( 'NONE', #32631, #3006, #17702 ) ;
#22192 = CYLINDRICAL_SURFACE ( 'NONE', #3114, 31.99999999999998579 ) ;
#22193 = LINE ( 'NONE', #41767, #30048 ) ;
#22194 = ORIENTED_EDGE ( 'NONE', *, *, #11964, .F. ) ;
#22195 = EDGE_CURVE ( 'NONE', #28331, #15680, #37859, .T. ) ;
#22196 = CARTESIAN_POINT ( 'NONE',  ( 23.41451323550360186, -132.5004227906269989, -5.500000000000000000 ) ) ;
#22197 = AXIS2_PLACEMENT_3D ( 'NONE', #29425, #44349, #19581 ) ;
#22198 = ORIENTED_EDGE ( 'NONE', *, *, #31929, .F. ) ;
#22199 = DIRECTION ( 'NONE',  ( -1.000000000000000000, -0.000000000000000000, -0.000000000000000000 ) ) ;
#22200 = ORIENTED_EDGE ( 'NONE', *, *, #25621, .T. ) ;
#22201 = AXIS2_PLACEMENT_3D ( 'NONE', #41960, #27756, #26769 ) ;
#22202 = AXIS2_PLACEMENT_3D ( 'NONE', #29048, #29536, #25611 ) ;
#22203 = AXIS2_PLACEMENT_3D ( 'NONE', #46416, #28775, #1627 ) ;
#22204 = CARTESIAN_POINT ( 'NONE',  ( 0.000000000000000000, -5.256550761633393520, 77.32052557432838569 ) ) ;
#22205 = VERTEX_POINT ( 'NONE', #26840 ) ;
#22206 = CARTESIAN_POINT ( 'NONE',  ( 0.000000000000000000, -30.00120703465189465, -22.64427369931201639 ) ) ;
#22207 = CYLINDRICAL_SURFACE ( 'NONE', #36203, 82.00000000000000000 ) ;
#22208 = CARTESIAN_POINT ( 'NONE',  ( 0.000000000000000000, -27.13269053701114331, 25.88420570971391754 ) ) ;
#22209 = CARTESIAN_POINT ( 'NONE',  ( 0.000000000000000000, 0.000000000000000000, 0.000000000000000000 ) ) ;
#22210 = EDGE_CURVE ( 'NONE', #59, #33522, #42749, .T. ) ;
#22211 = ORIENTED_EDGE ( 'NONE', *, *, #34056, .F. ) ;
#22212 = VECTOR ( 'NONE', #44975, 999.9999999999998863 ) ;
#22213 = AXIS2_PLACEMENT_3D ( 'NONE', #18882, #41916, #8369 ) ;
#22214 = CARTESIAN_POINT ( 'NONE',  ( -10.00000000000000000, 0.000000000000000000, 0.000000000000000000 ) ) ;
#22215 = CARTESIAN_POINT ( 'NONE',  ( 0.000000000000000000, 0.000000000000000000, 0.000000000000000000 ) ) ;
#22216 = CIRCLE ( 'NONE', #32393, 12.50000000000000000 ) ;
#22217 = EDGE_CURVE ( 'NONE', #18104, #43027, #22934, .T. ) ;
#22218 = CARTESIAN_POINT ( 'NONE',  ( 6.377742925735834234, -145.7647898336708181, 5.500000000000000000 ) ) ;
#22219 = CARTESIAN_POINT ( 'NONE',  ( -2.977765906491215642, 1.885622467823562354E-15, 15.39727592589476579 ) ) ;
#22220 = AXIS2_PLACEMENT_3D ( 'NONE', #2027, #1769, #20601 ) ;
#22221 = EDGE_CURVE ( 'NONE', #39014, #23379, #8078, .T. ) ;
#22222 = VERTEX_POINT ( 'NONE', #22922 ) ;
#22223 = VERTEX_POINT ( 'NONE', #16079 ) ;
#22224 = EDGE_CURVE ( 'NONE', #7935, #45678, #27568, .T. ) ;
#22225 = ORIENTED_EDGE ( 'NONE', *, *, #10847, .T. ) ;
#22226 = VERTEX_POINT ( 'NONE', #19974 ) ;
#22227 = AXIS2_PLACEMENT_3D ( 'NONE', #25988, #33577, #23707 ) ;
#22228 = DIRECTION ( 'NONE',  ( 1.000000000000000000, 0.000000000000000000, 0.000000000000000000 ) ) ;
#22229 = DIRECTION ( 'NONE',  ( -1.000000000000000000, -0.000000000000000000, 0.000000000000000000 ) ) ;
#22230 = VERTEX_POINT ( 'NONE', #31018 ) ;
#22231 = ORIENTED_EDGE ( 'NONE', *, *, #35301, .F. ) ;
#22232 = EDGE_LOOP ( 'NONE', ( #16497, #7112, #41702, #35619 ) ) ;
#22233 = AXIS2_PLACEMENT_3D ( 'NONE', #34227, #19522, #8295 ) ;
#22234 = CARTESIAN_POINT ( 'NONE',  ( 10.00000000000000000, 37.16516213103277977, 4.992566952385115719 ) ) ;
#22235 = AXIS2_PLACEMENT_3D ( 'NONE', #29996, #30249, #4306 ) ;
#22236 = VECTOR ( 'NONE', #41662, 1000.000000000000000 ) ;
#22237 = ORIENTED_EDGE ( 'NONE', *, *, #17456, .F. ) ;
#22238 = EDGE_LOOP ( 'NONE', ( #24924, #1976, #24817, #24751 ) ) ;
#22239 = CIRCLE ( 'NONE', #19874, 77.49900000000000944 ) ;
#22240 = PRODUCT_DEFINITION_SHAPE ( 'NONE', 'NONE',  #48455 ) ;
#22241 = DIRECTION ( 'NONE',  ( 0.000000000000000000, 0.3826834323650905589, -0.9238795325112864054 ) ) ;
#22242 = CIRCLE ( 'NONE', #10577, 82.00000000000000000 ) ;
#22243 = AXIS2_PLACEMENT_3D ( 'NONE', #1509, #35515, #46294 ) ;
#22244 = ORIENTED_EDGE ( 'NONE', *, *, #43381, .F. ) ;
#22245 = CARTESIAN_POINT ( 'NONE',  ( 11.99999999999999822, 21.60688246758696351, -79.10210256391344785 ) ) ;
#22246 = VERTEX_POINT ( 'NONE', #19253 ) ;
#22247 = CIRCLE ( 'NONE', #48027, 31.99999999999998224 ) ;
#22248 = FACE_OUTER_BOUND ( 'NONE', #27650, .T. ) ;
#22249 = AXIS2_PLACEMENT_3D ( 'NONE', #40479, #14038, #3503 ) ;
#22250 = DIRECTION ( 'NONE',  ( 0.000000000000000000, 0.000000000000000000, 1.000000000000000000 ) ) ;
#22251 = CARTESIAN_POINT ( 'NONE',  ( 0.000000000000000000, -51.02545421589285723, -55.20638768913812555 ) ) ;
#22252 = VERTEX_POINT ( 'NONE', #34651 ) ;
#22253 = VERTEX_POINT ( 'NONE', #45439 ) ;
#22254 = DIRECTION ( 'NONE',  ( -1.000000000000000000, -0.000000000000000000, 0.000000000000000000 ) ) ;
#22255 = FACE_OUTER_BOUND ( 'NONE', #24596, .T. ) ;
#22256 = VERTEX_POINT ( 'NONE', #41781 ) ;
#22257 = ORIENTED_EDGE ( 'NONE', *, *, #24323, .F. ) ;
#22258 = CARTESIAN_POINT ( 'NONE',  ( 10.00000000000000000, 0.000000000000000000, 0.000000000000000000 ) ) ;
#22259 = DIRECTION ( 'NONE',  ( -1.000000000000000000, 0.000000000000000000, -0.000000000000000000 ) ) ;
#22260 = ORIENTED_EDGE ( 'NONE', *, *, #9765, .T. ) ;
#22261 = FACE_OUTER_BOUND ( 'NONE', #24878, .T. ) ;
#22262 = DIRECTION ( 'NONE',  ( -0.08130631524010117905, 0.9966891607226784355, 0.000000000000000000 ) ) ;
#22263 = CARTESIAN_POINT ( 'NONE',  ( 11.99999999999999822, 41.76937507738788469, 62.50329211542452157 ) ) ;
#22264 = CARTESIAN_POINT ( 'NONE',  ( 5.999999999999999112, 33.71516098798849015, -74.74816331893393340 ) ) ;
#22265 = CARTESIAN_POINT ( 'NONE',  ( 0.000000000000000000, 0.000000000000000000, -40.00000000000000000 ) ) ;
#22266 = DIRECTION ( 'NONE',  ( 0.000000000000000000, 0.000000000000000000, 1.000000000000000000 ) ) ;
#22267 = DIRECTION ( 'NONE',  ( 0.000000000000000000, 0.5877852522924743583, -0.8090169943749466741 ) ) ;
#22268 = ADVANCED_FACE ( 'NONE', ( #8240 ), #38108, .F. ) ;
#22269 = CIRCLE ( 'NONE', #8985, 31.99999999999998579 ) ;
#22270 = CARTESIAN_POINT ( 'NONE',  ( 0.000000000000000000, -77.49459641780886443, -0.8261519478439277586 ) ) ;
#22271 = CARTESIAN_POINT ( 'NONE',  ( -10.00000000000000000, 0.000000000000000000, 0.000000000000000000 ) ) ;
#22272 = ADVANCED_FACE ( 'NONE', ( #19475 ), #1134, .T. ) ;
#22273 = VECTOR ( 'NONE', #29477, 1000.000000000000000 ) ;
#22274 = CARTESIAN_POINT ( 'NONE',  ( 0.000000000000000000, 5.202137450156907761, -37.22597642581151689 ) ) ;
#22275 = LINE ( 'NONE', #47488, #39448 ) ;
#22276 = ADVANCED_FACE ( 'NONE', ( #39565 ), #21171, .T. ) ;
#22277 = DIRECTION ( 'NONE',  ( 0.000000000000000000, -0.9238795325112821866, -0.3826834323651008285 ) ) ;
#22278 = ORIENTED_EDGE ( 'NONE', *, *, #36246, .F. ) ;
#22279 = ORIENTED_EDGE ( 'NONE', *, *, #21124, .T. ) ;
#22280 = VECTOR ( 'NONE', #29461, 1000.000000000000000 ) ;
#22281 = AXIS2_PLACEMENT_3D ( 'NONE', #484, #23238, #19535 ) ;
#22282 = DIRECTION ( 'NONE',  ( 0.000000000000000000, 0.000000000000000000, 1.000000000000000000 ) ) ;
#22283 = ADVANCED_FACE ( 'NONE', ( #31981 ), #46895, .T. ) ;
#22284 = AXIS2_PLACEMENT_3D ( 'NONE', #12749, #32313, #24239 ) ;
#22285 = EDGE_CURVE ( 'NONE', #9186, #36861, #20946, .T. ) ;
#22286 = DIRECTION ( 'NONE',  ( 1.000000000000000000, -0.000000000000000000, -0.000000000000000000 ) ) ;
#22287 = CIRCLE ( 'NONE', #40258, 82.00000000000000000 ) ;
#22288 = EDGE_LOOP ( 'NONE', ( #40497, #45639, #3092, #20407 ) ) ;
#22289 = VECTOR ( 'NONE', #19101, 1000.000000000000000 ) ;
#22290 = VERTEX_POINT ( 'NONE', #14078 ) ;
#22291 = DIRECTION ( 'NONE',  ( -1.000000000000000000, -0.000000000000000000, 0.000000000000000000 ) ) ;
#22292 = ORIENTED_EDGE ( 'NONE', *, *, #10784, .F. ) ;
#22293 = CYLINDRICAL_SURFACE ( 'NONE', #12820, 42.00000000000000000 ) ;
#22294 = ORIENTED_EDGE ( 'NONE', *, *, #18947, .T. ) ;
#22295 = EDGE_CURVE ( 'NONE', #12545, #48002, #30772, .T. ) ;
#22296 = VERTEX_POINT ( 'NONE', #39798 ) ;
#22297 = ORIENTED_EDGE ( 'NONE', *, *, #6036, .F. ) ;
#22298 = AXIS2_PLACEMENT_3D ( 'NONE', #37675, #25928, #40868 ) ;
#22299 = ORIENTED_EDGE ( 'NONE', *, *, #48228, .F. ) ;
#22300 = DIRECTION ( 'NONE',  ( -1.000000000000000000, -0.000000000000000000, -0.000000000000000000 ) ) ;
#22301 = VECTOR ( 'NONE', #12579, 1000.000000000000000 ) ;
#22302 = DIRECTION ( 'NONE',  ( 1.000000000000000000, -0.000000000000000000, -0.000000000000000000 ) ) ;
#22303 = EDGE_LOOP ( 'NONE', ( #32046, #14049, #41442, #13446 ) ) ;
#22304 = VERTEX_POINT ( 'NONE', #17500 ) ;
#22305 = VECTOR ( 'NONE', #30626, 1000.000000000000000 ) ;
#22306 = DIRECTION ( 'NONE',  ( 0.000000000000000000, 0.000000000000000000, -1.000000000000000000 ) ) ;
#22307 = ORIENTED_EDGE ( 'NONE', *, *, #9230, .F. ) ;
#22308 = DIRECTION ( 'NONE',  ( -1.000000000000000000, 0.000000000000000000, -0.000000000000000000 ) ) ;
#22309 = LINE ( 'NONE', #3697, #26743 ) ;
#22310 = ORIENTED_EDGE ( 'NONE', *, *, #10041, .F. ) ;
#22311 = CARTESIAN_POINT ( 'NONE',  ( 0.000000000000000000, 0.000000000000000000, 52.00000000000002132 ) ) ;
#22312 = CARTESIAN_POINT ( 'NONE',  ( -18.24502636017238899, -100.7225776329765665, 5.500000000000000000 ) ) ;
#22314 = ORIENTED_EDGE ( 'NONE', *, *, #18313, .F. ) ;
#22313 = CARTESIAN_POINT ( 'NONE',  ( 10.00000000000000000, 0.000000000000000000, 0.000000000000000000 ) ) ;
#22315 = ADVANCED_FACE ( 'NONE', ( #24852 ), #17252, .F. ) ;
#22316 = DIRECTION ( 'NONE',  ( 0.000000000000000000, 0.000000000000000000, 1.000000000000000000 ) ) ;
#22317 = AXIS2_PLACEMENT_3D ( 'NONE', #44392, #29220, #7182 ) ;
#22318 = ORIENTED_EDGE ( 'NONE', *, *, #41297, .T. ) ;
#22319 = DIRECTION ( 'NONE',  ( 0.8225049752423776450, 0.5687579148473764779, 0.000000000000000000 ) ) ;
#22320 = ORIENTED_EDGE ( 'NONE', *, *, #46546, .T. ) ;
#22321 = VERTEX_POINT ( 'NONE', #35382 ) ;
#22322 = CARTESIAN_POINT ( 'NONE',  ( 16.30584220631899228, -140.9432449716519784, 5.500000000000000000 ) ) ;
#22323 = CARTESIAN_POINT ( 'NONE',  ( 10.00000000000000000, 37.48860685352291000, -0.8828120875901940279 ) ) ;
#22324 = ORIENTED_EDGE ( 'NONE', *, *, #18901, .T. ) ;
#22325 = EDGE_CURVE ( 'NONE', #14880, #40287, #39304, .T. ) ;
#22326 = DIRECTION ( 'NONE',  ( -1.000000000000000000, -0.000000000000000000, -0.000000000000000000 ) ) ;
#22327 = VECTOR ( 'NONE', #7458, 1000.000000000000000 ) ;
#22328 = DIRECTION ( 'NONE',  ( 1.000000000000000000, 0.000000000000000000, 0.000000000000000000 ) ) ;
#22329 = FACE_OUTER_BOUND ( 'NONE', #10470, .T. ) ;
#22330 = EDGE_CURVE ( 'NONE', #35415, #28305, #38608, .T. ) ;
#22331 = CIRCLE ( 'NONE', #2748, 31.99999999999999289 ) ;
#22332 = CARTESIAN_POINT ( 'NONE',  ( 0.000000000000000000, -37.16516213103280108, 4.992566952384862589 ) ) ;
#22333 = CARTESIAN_POINT ( 'NONE',  ( 0.000000000000000000, 67.80270845531956070, -46.11716303203112943 ) ) ;
#22334 = FACE_OUTER_BOUND ( 'NONE', #16679, .T. ) ;
#22335 = ORIENTED_EDGE ( 'NONE', *, *, #36543, .T. ) ;
#22336 = LINE ( 'NONE', #21832, #13710 ) ;
#22337 = CARTESIAN_POINT ( 'NONE',  ( -0.9515373497862389396, -96.47140937769621871, 5.500000000000000000 ) ) ;
#22338 = DIRECTION ( 'NONE',  ( -1.000000000000000000, 0.000000000000000000, -0.000000000000000000 ) ) ;
#22339 = LINE ( 'NONE', #8365, #30201 ) ;
#22340 = LINE ( 'NONE', #26491, #15112 ) ;
#22341 = DIRECTION ( 'NONE',  ( 0.000000000000000000, 0.000000000000000000, 1.000000000000000000 ) ) ;
#22342 = FACE_OUTER_BOUND ( 'NONE', #71, .T. ) ;
#22343 = EDGE_CURVE ( 'NONE', #40483, #33807, #13852, .T. ) ;
#22344 = DIRECTION ( 'NONE',  ( 0.000000000000000000, 0.000000000000000000, 1.000000000000000000 ) ) ;
#22345 = EDGE_CURVE ( 'NONE', #34798, #46920, #28426, .T. ) ;
#22346 = EDGE_CURVE ( 'NONE', #46699, #42002, #8855, .T. ) ;
#22347 = VECTOR ( 'NONE', #4461, 1000.000000000000000 ) ;
#22348 = CARTESIAN_POINT ( 'NONE',  ( -10.00000000000000000, 0.000000000000000000, 0.000000000000000000 ) ) ;
#22349 = ORIENTED_EDGE ( 'NONE', *, *, #46120, .T. ) ;
#22350 = CARTESIAN_POINT ( 'NONE',  ( 12.00000000000000000, -10.45096189432344502, -21.10159698893425073 ) ) ;
#22351 = CARTESIAN_POINT ( 'NONE',  ( 0.000000000000000000, 0.000000000000000000, 0.000000000000000000 ) ) ;
#22352 = DIRECTION ( 'NONE',  ( 0.000000000000000000, 0.000000000000000000, 1.000000000000000000 ) ) ;
#22353 = EDGE_LOOP ( 'NONE', ( #8380, #9641, #20523, #39384 ) ) ;
#22354 = PRODUCT_DEFINITION ( 'UNKNOWN', '', #35818, #3673 ) ;
#22355 = VECTOR ( 'NONE', #23264, 1000.000000000000000 ) ;
#22356 = DIRECTION ( 'NONE',  ( -1.000000000000000000, 0.000000000000000000, 0.000000000000000000 ) ) ;
#22357 = VECTOR ( 'NONE', #18411, 1000.000000000000000 ) ;
#22358 = ORIENTED_EDGE ( 'NONE', *, *, #25861, .F. ) ;
#22359 = DIRECTION ( 'NONE',  ( 0.000000000000000000, 0.000000000000000000, -1.000000000000000000 ) ) ;
#22360 = CLOSED_SHELL ( 'NONE', ( #23645, #11596, #37738, #31454, #10670, #26991, #18441, #2465, #44591, #21506, #43995, #20779, #40353, #42202, #12714, #27341, #14211, #30461, #16039, #39766, #25685, #3059, #47370, #27888, #42984, #33833, #4227, #15118, #15313, #32286, #14041, #2595, #44028, #9911, #44986, #46206, #38766, #15790, #42615, #2000, #12717, #28891 ) ) ;
#22361 = FACE_OUTER_BOUND ( 'NONE', #45756, .T. ) ;
#22363 = ORIENTED_EDGE ( 'NONE', *, *, #618, .F. ) ;
#22362 = DIRECTION ( 'NONE',  ( -1.000000000000000000, -0.000000000000000000, -0.000000000000000000 ) ) ;
#22364 = ORIENTED_EDGE ( 'NONE', *, *, #42206, .F. ) ;
#22365 = CARTESIAN_POINT ( 'NONE',  ( 10.00000000000000000, -0.8828120875903202602, 37.48860685352291000 ) ) ;
#22366 = CIRCLE ( 'NONE', #45011, 82.00000000000000000 ) ;
#22367 = ORIENTED_EDGE ( 'NONE', *, *, #31969, .F. ) ;
#22368 = CARTESIAN_POINT ( 'NONE',  ( 0.000000000000000000, -51.03279382321048985, -55.19960302592120627 ) ) ;
#22369 = DIRECTION ( 'NONE',  ( -0.000000000000000000, -0.000000000000000000, -1.000000000000000000 ) ) ;
#22370 = CARTESIAN_POINT ( 'NONE',  ( 15.00000000000000000, -0.9646360437372099028, 23.52805723605590771 ) ) ;
#22371 = VECTOR ( 'NONE', #10276, 1000.000000000000000 ) ;
#22372 = PLANE ( 'NONE',  #16382 ) ;
#22373 = EDGE_CURVE ( 'NONE', #25110, #21860, #2333, .T. ) ;
#22374 = VERTEX_POINT ( 'NONE', #32211 ) ;
#22375 = LINE ( 'NONE', #3032, #10718 ) ;
#22376 = ORIENTED_EDGE ( 'NONE', *, *, #23415, .T. ) ;
#22377 = ORIENTED_EDGE ( 'NONE', *, *, #1150, .F. ) ;
#22378 = CARTESIAN_POINT ( 'NONE',  ( -235.0000123116479926, -123.0000000000000284, 2.500000000000000000 ) ) ;
#22379 = ADVANCED_FACE ( 'NONE', ( #32673 ), #20701, .T. ) ;
#22380 = DIRECTION ( 'NONE',  ( 1.000000000000000000, 0.000000000000000000, 0.000000000000000000 ) ) ;
#22381 = DIRECTION ( 'NONE',  ( -1.000000000000000000, -0.000000000000000000, 0.000000000000000000 ) ) ;
#22382 = CARTESIAN_POINT ( 'NONE',  ( 23.41451323550360186, -132.5004227906269989, 5.500000000000000000 ) ) ;
#22383 = ORIENTED_EDGE ( 'NONE', *, *, #15439, .T. ) ;
#22384 = CARTESIAN_POINT ( 'NONE',  ( 10.00000000000000000, 69.42325613327489009, -34.44570377933524696 ) ) ;
#22385 = EDGE_CURVE ( 'NONE', #13149, #9644, #27633, .T. ) ;
#22386 = DIRECTION ( 'NONE',  ( 0.000000000000000000, -0.000000000000000000, -1.000000000000000000 ) ) ;
#22387 = DIRECTION ( 'NONE',  ( -1.000000000000000000, 0.000000000000000000, 0.000000000000000000 ) ) ;
#22388 = DIRECTION ( 'NONE',  ( -1.000000000000000000, -0.000000000000000000, -0.000000000000000000 ) ) ;
#22389 = CYLINDRICAL_SURFACE ( 'NONE', #26237, 77.49899999999999523 ) ;
#22390 = AXIS2_PLACEMENT_3D ( 'NONE', #6535, #9714, #17059 ) ;
#22391 = CARTESIAN_POINT ( 'NONE',  ( 10.00000000000000000, 29.81001611431009479, 22.74946021919143391 ) ) ;
#22392 = FACE_OUTER_BOUND ( 'NONE', #40388, .T. ) ;
#22393 = FACE_OUTER_BOUND ( 'NONE', #16854, .T. ) ;
#22394 = VECTOR ( 'NONE', #34527, 1000.000000000000000 ) ;
#22395 = FACE_OUTER_BOUND ( 'NONE', #20056, .T. ) ;
#22396 = DIRECTION ( 'NONE',  ( -1.000000000000000000, -0.000000000000000000, -0.000000000000000000 ) ) ;
#22397 = EDGE_CURVE ( 'NONE', #27937, #13040, #2109, .T. ) ;
#22398 = EDGE_CURVE ( 'NONE', #33047, #188, #4988, .T. ) ;
#22399 = DIRECTION ( 'NONE',  ( -1.000000000000000000, 0.000000000000000000, 0.000000000000000000 ) ) ;
#22400 = CARTESIAN_POINT ( 'NONE',  ( 5.000000000000000000, 21.60688246758696707, -79.10210256391346206 ) ) ;
#22401 = DIRECTION ( 'NONE',  ( -1.000000000000000000, -0.000000000000000000, 0.000000000000000000 ) ) ;
#22402 = CIRCLE ( 'NONE', #1296, 82.00000000000000000 ) ;
#22403 = CARTESIAN_POINT ( 'NONE',  ( 15.00000000000000000, -10.45096189432314127, 21.10159698893440350 ) ) ;
#22404 = CARTESIAN_POINT ( 'NONE',  ( 5.000000000000000000, -32.34446384429951138, -26.79245525562750530 ) ) ;
#22405 = CIRCLE ( 'NONE', #25503, 31.99999999999998934 ) ;
#22406 = FACE_OUTER_BOUND ( 'NONE', #15281, .T. ) ;
#22407 = VERTEX_POINT ( 'NONE', #16799 ) ;
#22408 = ORIENTED_EDGE ( 'NONE', *, *, #15133, .F. ) ;
#22409 = EDGE_CURVE ( 'NONE', #28111, #39825, #31748, .T. ) ;
#22410 = CIRCLE ( 'NONE', #27102, 16.00000000000000000 ) ;
#22411 = ORIENTED_EDGE ( 'NONE', *, *, #41897, .F. ) ;
#22412 = ORIENTED_EDGE ( 'NONE', *, *, #17990, .F. ) ;
#22413 = CYLINDRICAL_SURFACE ( 'NONE', #23420, 14.09999999999999964 ) ;
#22414 = ORIENTED_EDGE ( 'NONE', *, *, #7551, .F. ) ;
#22415 = AXIS2_PLACEMENT_3D ( 'NONE', #18471, #11853, #40998 ) ;
#22416 = AXIS2_PLACEMENT_3D ( 'NONE', #25839, #10928, #21701 ) ;
#22417 = FACE_OUTER_BOUND ( 'NONE', #6158, .T. ) ;
#22418 = DIRECTION ( 'NONE',  ( -1.000000000000000000, -0.000000000000000000, 0.000000000000000000 ) ) ;
#22420 = ORIENTED_EDGE ( 'NONE', *, *, #35910, .F. ) ;
#22419 = CARTESIAN_POINT ( 'NONE',  ( 0.000000000000000000, 49.70050353004977239, -59.46389618801908483 ) ) ;
#22421 = EDGE_LOOP ( 'NONE', ( #43110, #46915, #137, #33779 ) ) ;
#22422 = AXIS2_PLACEMENT_3D ( 'NONE', #12956, #20513, #28601 ) ;
#22423 = DIRECTION ( 'NONE',  ( 1.000000000000000000, -0.000000000000000000, 0.000000000000000000 ) ) ;
#22424 = EDGE_LOOP ( 'NONE', ( #28906, #7506, #34385, #7223 ) ) ;
#22425 = ORIENTED_EDGE ( 'NONE', *, *, #10501, .T. ) ;
#22426 = ORIENTED_EDGE ( 'NONE', *, *, #12225, .T. ) ;
#22427 = CARTESIAN_POINT ( 'NONE',  ( 0.000000000000000000, 0.000000000000000000, 0.000000000000000000 ) ) ;
#22428 = CARTESIAN_POINT ( 'NONE',  ( 12.50000000000000000, -132.5000000000000000, 40.00000000000000000 ) ) ;
#22429 = DIRECTION ( 'NONE',  ( -1.000000000000000000, -0.000000000000000000, -0.000000000000000000 ) ) ;
#22430 = ORIENTED_EDGE ( 'NONE', *, *, #37873, .F. ) ;
#22431 = ORIENTED_EDGE ( 'NONE', *, *, #9593, .T. ) ;
#22432 = ORIENTED_EDGE ( 'NONE', *, *, #13327, .T. ) ;
#22433 = DIRECTION ( 'NONE',  ( -1.000000000000000000, 0.000000000000000000, 0.000000000000000000 ) ) ;
#22434 = ORIENTED_EDGE ( 'NONE', *, *, #35541, .T. ) ;
#22435 = DIRECTION ( 'NONE',  ( 0.000000000000000000, 1.000000000000000000, 3.491481338843133355E-15 ) ) ;
#22436 = EDGE_CURVE ( 'NONE', #37649, #44937, #44660, .T. ) ;
#22437 = DIRECTION ( 'NONE',  ( -1.000000000000000000, -0.000000000000000000, -0.000000000000000000 ) ) ;
#22438 = CARTESIAN_POINT ( 'NONE',  ( -10.00000000000000000, 0.000000000000000000, 0.000000000000000000 ) ) ;
#22439 = DIRECTION ( 'NONE',  ( 0.000000000000000000, 0.3090169943749410675, 0.9510565162951556406 ) ) ;
#22440 = CARTESIAN_POINT ( 'NONE',  ( 10.00000000000000000, 0.000000000000000000, 0.000000000000000000 ) ) ;
#22441 = LINE ( 'NONE', #44463, #25256 ) ;
#22442 = CIRCLE ( 'NONE', #32590, 31.99999999999999289 ) ;
#22443 = ADVANCED_FACE ( 'NONE', ( #36821 ), #349, .T. ) ;
#22444 = LINE ( 'NONE', #42239, #24444 ) ;
#22445 = ORIENTED_EDGE ( 'NONE', *, *, #26378, .F. ) ;
#22446 = DIRECTION ( 'NONE',  ( -1.000000000000000000, -0.000000000000000000, 0.000000000000000000 ) ) ;
#22447 = LINE ( 'NONE', #33682, #47231 ) ;
#22448 = ORIENTED_EDGE ( 'NONE', *, *, #1148, .F. ) ;
#22449 = AXIS2_PLACEMENT_3D ( 'NONE', #43699, #28287, #9934 ) ;
#22450 = CARTESIAN_POINT ( 'NONE',  ( 0.000000000000000000, 0.000000000000000000, -125.0000000000000000 ) ) ;
#22451 = ORIENTED_EDGE ( 'NONE', *, *, #12173, .F. ) ;
#22452 = ADVANCED_FACE ( 'NONE', ( #33877 ), #15301, .T. ) ;
#22453 = LINE ( 'NONE', #22917, #31204 ) ;
#22454 = EDGE_LOOP ( 'NONE', ( #22363, #39418, #48363, #41167 ) ) ;
#22455 = DIRECTION ( 'NONE',  ( 0.000000000000000000, -0.5877852522924624790, -0.8090169943749553338 ) ) ;
#22456 = PLANE ( 'NONE',  #29843 ) ;
#22457 = LINE ( 'NONE', #33935, #25215 ) ;
#22458 = AXIS2_PLACEMENT_3D ( 'NONE', #37067, #2812, #43931 ) ;
#22459 = EDGE_CURVE ( 'NONE', #21525, #23147, #26077, .T. ) ;
#22460 = DIRECTION ( 'NONE',  ( -1.000000000000000000, -0.000000000000000000, 0.000000000000000000 ) ) ;
#22461 = CARTESIAN_POINT ( 'NONE',  ( 11.99999999999999822, 69.42325613327489009, -34.44570377933524696 ) ) ;
#22462 = AXIS2_PLACEMENT_3D ( 'NONE', #7190, #32653, #48308 ) ;
#22463 = CARTESIAN_POINT ( 'NONE',  ( 4.999999999999999112, 10.41901085202078292, 40.68715046381932865 ) ) ;
#22464 = DIRECTION ( 'NONE',  ( 0.000000000000000000, 0.000000000000000000, 1.000000000000000000 ) ) ;
#22465 = EDGE_CURVE ( 'NONE', #22704, #43358, #41244, .T. ) ;
#22466 = AXIS2_PLACEMENT_3D ( 'NONE', #37864, #11680, #26606 ) ;
#22467 = FACE_OUTER_BOUND ( 'NONE', #35875, .T. ) ;
#22468 = FILL_AREA_STYLE ('',( #41793 ) ) ;
#22469 = LINE ( 'NONE', #22219, #18234 ) ;
#22470 = EDGE_LOOP ( 'NONE', ( #8280, #46879, #25936, #8084 ) ) ;
#22471 = EDGE_CURVE ( 'NONE', #11742, #26881, #29492, .T. ) ;
#22472 = CIRCLE ( 'NONE', #47471, 15.99999999999999822 ) ;
#22473 = ORIENTED_EDGE ( 'NONE', *, *, #34184, .F. ) ;
#22474 = ORIENTED_EDGE ( 'NONE', *, *, #18157, .F. ) ;
#22475 = DIRECTION ( 'NONE',  ( -1.000000000000000000, 0.000000000000000000, 0.000000000000000000 ) ) ;
#22476 = DIRECTION ( 'NONE',  ( -1.000000000000000000, -0.000000000000000000, -0.000000000000000000 ) ) ;
#22477 = CIRCLE ( 'NONE', #40478, 77.49899999999998101 ) ;
#22478 = EDGE_CURVE ( 'NONE', #31583, #45656, #17477, .T. ) ;
#22479 = CYLINDRICAL_SURFACE ( 'NONE', #31999, 37.49900000000000233 ) ;
#22480 = VERTEX_POINT ( 'NONE', #33407 ) ;
#22481 = DIRECTION ( 'NONE',  ( 0.000000000000000000, 0.000000000000000000, 1.000000000000000000 ) ) ;
#22482 = AXIS2_PLACEMENT_3D ( 'NONE', #41635, #45538, #37968 ) ;
#22483 = CARTESIAN_POINT ( 'NONE',  ( 10.00000000000000000, -37.58145647212455032, 0.6853352020789044152 ) ) ;
#22484 = ORIENTED_EDGE ( 'NONE', *, *, #37903, .F. ) ;
#22485 = CARTESIAN_POINT ( 'NONE',  ( 11.99999999999999822, -29.01471420065506379, -76.69515212746047439 ) ) ;
#22486 = VERTEX_POINT ( 'NONE', #15050 ) ;
#22487 = ADVANCED_FACE ( 'NONE', ( #44423 ), #29251, .T. ) ;
#22488 = ORIENTED_EDGE ( 'NONE', *, *, #43384, .T. ) ;
#22489 = PLANE ( 'NONE',  #47842 ) ;
#22490 = EDGE_CURVE ( 'NONE', #16462, #46727, #21666, .T. ) ;
#22491 = CARTESIAN_POINT ( 'NONE',  ( 0.000000000000000000, 0.000000000000000000, 0.000000000000000000 ) ) ;
#22492 = DIRECTION ( 'NONE',  ( -1.000000000000000000, -0.000000000000000000, 0.000000000000000000 ) ) ;
#22493 = VERTEX_POINT ( 'NONE', #14809 ) ;
#22494 = ADVANCED_FACE ( 'NONE', ( #3782 ), #26057, .T. ) ;
#22495 = ORIENTED_EDGE ( 'NONE', *, *, #18986, .T. ) ;
#22496 = CARTESIAN_POINT ( 'NONE',  ( 0.000000000000000000, 30.00120703465205452, 22.64427369931179967 ) ) ;
#22497 = DIRECTION ( 'NONE',  ( 0.000000000000000000, 0.000000000000000000, 1.000000000000000000 ) ) ;
#22498 = VERTEX_POINT ( 'NONE', #14319 ) ;
#22499 = ORIENTED_EDGE ( 'NONE', *, *, #48139, .F. ) ;
#22500 = EDGE_CURVE ( 'NONE', #37649, #35793, #40744, .T. ) ;
#22501 = CARTESIAN_POINT ( 'NONE',  ( 10.00000000000000000, 0.000000000000000000, 0.000000000000000000 ) ) ;
#22502 = ORIENTED_EDGE ( 'NONE', *, *, #41607, .F. ) ;
#22503 = DIRECTION ( 'NONE',  ( -1.000000000000000000, -0.000000000000000000, -0.000000000000000000 ) ) ;
#22504 = CARTESIAN_POINT ( 'NONE',  ( 5.000000000000000000, 21.40280677340421889, -36.13751322684397138 ) ) ;
#22505 = DIRECTION ( 'NONE',  ( 0.000000000000000000, 0.000000000000000000, 1.000000000000000000 ) ) ;
#22506 = FACE_OUTER_BOUND ( 'NONE', #2142, .T. ) ;
#22507 = DIRECTION ( 'NONE',  ( 1.000000000000000000, 0.000000000000000000, 0.000000000000000000 ) ) ;
#22508 = LINE ( 'NONE', #14920, #46905 ) ;
#22509 = AXIS2_PLACEMENT_3D ( 'NONE', #19238, #34387, #41518 ) ;
#22510 = LINE ( 'NONE', #25924, #45063 ) ;
#22511 = CARTESIAN_POINT ( 'NONE',  ( 0.000000000000000000, 35.91791733033476675, 68.67312586195008350 ) ) ;
#22512 = CARTESIAN_POINT ( 'NONE',  ( 0.000000000000000000, 0.000000000000000000, 0.000000000000000000 ) ) ;
#22513 = ORIENTED_EDGE ( 'NONE', *, *, #27721, .F. ) ;
#22514 = LINE ( 'NONE', #33516, #10379 ) ;
#22515 = DIRECTION ( 'NONE',  ( 0.000000000000000000, -0.1564344650402380854, 0.9876883405951365491 ) ) ;
#22516 = SURFACE_STYLE_FILL_AREA ( #485 ) ;
#22517 = LINE ( 'NONE', #23240, #38939 ) ;
#22518 = EDGE_LOOP ( 'NONE', ( #31830, #34090, #20556, #37231 ) ) ;
#22519 = AXIS2_PLACEMENT_3D ( 'NONE', #37363, #48137, #33678 ) ;
#22520 = EDGE_CURVE ( 'NONE', #17154, #24143, #7696, .T. ) ;
#22521 = LINE ( 'NONE', #491, #228 ) ;
#22522 = AXIS2_PLACEMENT_3D ( 'NONE', #32850, #5533, #20455 ) ;
#22523 = DIRECTION ( 'NONE',  ( 0.000000000000000000, -0.8090169943749422332, -0.5877852522924803536 ) ) ;
#22524 = EDGE_CURVE ( 'NONE', #13690, #35068, #6740, .T. ) ;
#22525 = DIRECTION ( 'NONE',  ( 1.000000000000000000, 0.000000000000000000, -0.000000000000000000 ) ) ;
#22526 = AXIS2_PLACEMENT_3D ( 'NONE', #10194, #21453, #36386 ) ;
#22527 = VERTEX_POINT ( 'NONE', #44904 ) ;
#22528 = CARTESIAN_POINT ( 'NONE',  ( 6.000000000000000000, -81.96053171279901051, -2.543863470249253300 ) ) ;
#22529 = ORIENTED_EDGE ( 'NONE', *, *, #15432, .T. ) ;
#22530 = ORIENTED_EDGE ( 'NONE', *, *, #7422, .F. ) ;
#22531 = ORIENTED_EDGE ( 'NONE', *, *, #44995, .F. ) ;
#22532 = ORIENTED_EDGE ( 'NONE', *, *, #14104, .F. ) ;
#22533 = CARTESIAN_POINT ( 'NONE',  ( 10.00000000000000000, -5.202137450156655518, 37.22597642581156663 ) ) ;
#22534 = AXIS2_PLACEMENT_3D ( 'NONE', #25759, #33593, #3498 ) ;
#22535 = VECTOR ( 'NONE', #33350, 1000.000000000000000 ) ;
#22536 = DIRECTION ( 'NONE',  ( -1.000000000000000000, 0.000000000000000000, 0.000000000000000000 ) ) ;
#22537 = ORIENTED_EDGE ( 'NONE', *, *, #39068, .T. ) ;
#22538 = ORIENTED_EDGE ( 'NONE', *, *, #45948, .F. ) ;
#22539 = EDGE_CURVE ( 'NONE', #41161, #8489, #47939, .T. ) ;
#22540 = DIRECTION ( 'NONE',  ( -1.000000000000000000, 0.000000000000000000, 0.000000000000000000 ) ) ;
#22541 = ORIENTED_EDGE ( 'NONE', *, *, #46582, .F. ) ;
#22542 = CARTESIAN_POINT ( 'NONE',  ( 11.99999999999999822, 0.000000000000000000, 0.000000000000000000 ) ) ;
#22543 = EDGE_CURVE ( 'NONE', #41271, #7167, #26309, .T. ) ;
#22544 = CARTESIAN_POINT ( 'NONE',  ( -3.000000000000000000, -0.9646360437372163421, -23.52805723605591126 ) ) ;
#22545 = VERTEX_POINT ( 'NONE', #36588 ) ;
#22546 = CARTESIAN_POINT ( 'NONE',  ( 0.000000000000000000, 66.50666863322055633, -39.78640506895536078 ) ) ;
#22547 = FACE_OUTER_BOUND ( 'NONE', #1866, .T. ) ;
#22548 = VERTEX_POINT ( 'NONE', #17975 ) ;
#22549 = DIRECTION ( 'NONE',  ( 1.000000000000000000, 0.000000000000000000, -0.000000000000000000 ) ) ;
#22550 = CARTESIAN_POINT ( 'NONE',  ( 0.000000000000000000, 2.946379043146343246, 75.11764819372150725 ) ) ;
#22551 = VERTEX_POINT ( 'NONE', #6976 ) ;
#22552 = CARTESIAN_POINT ( 'NONE',  ( 10.00000000000000000, -16.23288003029521320, 33.80338159004277543 ) ) ;
#22553 = ORIENTED_EDGE ( 'NONE', *, *, #38666, .F. ) ;
#22554 = VERTEX_POINT ( 'NONE', #44181 ) ;
#22555 = EDGE_CURVE ( 'NONE', #6051, #43074, #10659, .T. ) ;
#22556 = DIRECTION ( 'NONE',  ( -1.000000000000000000, -0.000000000000000000, -0.000000000000000000 ) ) ;
#22557 = DIRECTION ( 'NONE',  ( 0.000000000000000000, 0.7071067811865486830, -0.7071067811865463515 ) ) ;
#22558 = ORIENTED_EDGE ( 'NONE', *, *, #9995, .F. ) ;
#22559 = CIRCLE ( 'NONE', #48336, 77.49900000000002365 ) ;
#22560 = FACE_OUTER_BOUND ( 'NONE', #9908, .T. ) ;
#22561 = ADVANCED_FACE ( 'NONE', ( #41973 ), #597, .T. ) ;
#22562 = CARTESIAN_POINT ( 'NONE',  ( 12.00000000000000000, 18.84667830672605859, 18.68964196561243085 ) ) ;
#22563 = LINE ( 'NONE', #10824, #35455 ) ;
#22564 = AXIS2_PLACEMENT_3D ( 'NONE', #3817, #7243, #3573 ) ;
#22565 = CYLINDRICAL_SURFACE ( 'NONE', #46874, 31.99999999999998579 ) ;
#22566 = CARTESIAN_POINT ( 'NONE',  ( 0.000000000000000000, -120.0000000000000000, 40.00000000000000711 ) ) ;
#22567 = DIRECTION ( 'NONE',  ( -1.000000000000000000, -0.000000000000000000, -0.000000000000000000 ) ) ;
#22568 = DIRECTION ( 'NONE',  ( -0.5687579148473765889, 0.8225049752423776450, 0.000000000000000000 ) ) ;
#22569 = DIRECTION ( 'NONE',  ( 0.000000000000000000, -0.8910065241883626808, -0.4539904997395570740 ) ) ;
#22570 = CARTESIAN_POINT ( 'NONE',  ( 10.00000000000000000, 37.16516213103285082, -4.992566952384588141 ) ) ;
#22571 = CYLINDRICAL_SURFACE ( 'NONE', #30976, 0.9999999999999991118 ) ;
#22572 = LINE ( 'NONE', #18420, #4106 ) ;
#22573 = LINE ( 'NONE', #21838, #296 ) ;
#22574 = DIRECTION ( 'NONE',  ( 0.000000000000000000, 0.000000000000000000, 1.000000000000000000 ) ) ;
#22575 = CARTESIAN_POINT ( 'NONE',  ( -23.30023580412278505, -123.4057321492263384, 5.500000000000000000 ) ) ;
#22576 = ORIENTED_EDGE ( 'NONE', *, *, #43344, .T. ) ;
#22577 = DIRECTION ( 'NONE',  ( -1.000000000000000000, 0.000000000000000000, 0.000000000000000000 ) ) ;
#22578 = ORIENTED_EDGE ( 'NONE', *, *, #36080, .F. ) ;
#22579 = APPLICATION_CONTEXT ( 'automotive_design' ) ;
#22580 = LINE ( 'NONE', #3987, #11959 ) ;
#22581 = DIRECTION ( 'NONE',  ( 0.000000000000000000, 0.000000000000000000, 1.000000000000000000 ) ) ;
#22582 = ORIENTED_EDGE ( 'NONE', *, *, #18602, .F. ) ;
#22583 = AXIS2_PLACEMENT_3D ( 'NONE', #14887, #11214, #180 ) ;
#22584 = ADVANCED_FACE ( 'NONE', ( #7929 ), #1071, .F. ) ;
#22585 = CARTESIAN_POINT ( 'NONE',  ( 15.00000000000000000, -25.60904388321925040, -6.976881207771165272 ) ) ;
#22586 = AXIS2_PLACEMENT_3D ( 'NONE', #48166, #29330, #40359 ) ;
#22587 = ORIENTED_EDGE ( 'NONE', *, *, #31126, .T. ) ;
#22588 = VERTEX_POINT ( 'NONE', #30958 ) ;
#22589 = ADVANCED_FACE ( 'NONE', ( #4751 ), #4995, .F. ) ;
#22590 = DIRECTION ( 'NONE',  ( 8.090853898039833646E-17, -9.269810975720164453E-17, 1.000000000000000000 ) ) ;
#22591 = EDGE_LOOP ( 'NONE', ( #3622, #8215, #25912, #25332 ) ) ;
#22592 = DIRECTION ( 'NONE',  ( -0.000000000000000000, -0.000000000000000000, -1.000000000000000000 ) ) ;
#22594 = ORIENTED_EDGE ( 'NONE', *, *, #4983, .F. ) ;
#22593 = DIRECTION ( 'NONE',  ( 0.000000000000000000, -0.4539904997395351471, -0.8910065241883738940 ) ) ;
#22595 = VERTEX_POINT ( 'NONE', #8422 ) ;
#22596 = EDGE_CURVE ( 'NONE', #29992, #409, #21363, .T. ) ;
#22597 = EDGE_CURVE ( 'NONE', #10969, #23846, #8648, .T. ) ;
#22598 = ADVANCED_FACE ( 'NONE', ( #5248 ), #16016, .T. ) ;
#22599 = DIRECTION ( 'NONE',  ( -1.000000000000000000, -0.000000000000000000, 0.000000000000000000 ) ) ;
#22600 = CARTESIAN_POINT ( 'NONE',  ( -23.54415474984308432, -120.4156646670583086, -2.500000000000000000 ) ) ;
#22601 = DIRECTION ( 'NONE',  ( -1.000000000000000000, -0.000000000000000000, 0.000000000000000000 ) ) ;
#22602 = MECHANICAL_DESIGN_GEOMETRIC_PRESENTATION_REPRESENTATION (  '', ( #16359 ), #26452 ) ;
#22603 = DIRECTION ( 'NONE',  ( -1.000000000000000000, 0.000000000000000000, -0.000000000000000000 ) ) ;
#22604 = ORIENTED_EDGE ( 'NONE', *, *, #25412, .F. ) ;
#22605 = DIRECTION ( 'NONE',  ( 0.000000000000000000, 0.000000000000000000, 1.000000000000000000 ) ) ;
#22606 = ORIENTED_EDGE ( 'NONE', *, *, #1513, .T. ) ;
#22607 = ORIENTED_EDGE ( 'NONE', *, *, #15798, .F. ) ;
#22608 = CARTESIAN_POINT ( 'NONE',  ( -10.00000000000000000, 0.000000000000000000, 0.000000000000000000 ) ) ;
#22609 = DIRECTION ( 'NONE',  ( 0.000000000000000000, 0.000000000000000000, -1.000000000000000000 ) ) ;
#22610 = EDGE_CURVE ( 'NONE', #3259, #37588, #25267, .T. ) ;
#22611 = DIRECTION ( 'NONE',  ( -0.6862798483830544471, -0.7273375899149802093, 0.000000000000000000 ) ) ;
#22612 = CARTESIAN_POINT ( 'NONE',  ( -10.00000000000000000, 0.000000000000000000, 0.000000000000000000 ) ) ;
#22613 = ORIENTED_EDGE ( 'NONE', *, *, #31929, .T. ) ;
#22614 = FACE_OUTER_BOUND ( 'NONE', #31289, .T. ) ;
#22615 = FACE_OUTER_BOUND ( 'NONE', #42795, .T. ) ;
#22616 = CARTESIAN_POINT ( 'NONE',  ( 0.000000000000000000, 0.000000000000000000, 0.000000000000000000 ) ) ;
#22617 = DIRECTION ( 'NONE',  ( 0.000000000000000000, 0.000000000000000000, 1.000000000000000000 ) ) ;
#22619 = AXIS2_PLACEMENT_3D ( 'NONE', #9545, #42861, #31862 ) ;
#22618 = FACE_OUTER_BOUND ( 'NONE', #23796, .T. ) ;
#22620 = LINE ( 'NONE', #37552, #44981 ) ;
#22621 = CARTESIAN_POINT ( 'NONE',  ( 10.00000000000000000, -28.89263327155693517, -71.91182617369219088 ) ) ;
#22622 = CARTESIAN_POINT ( 'NONE',  ( 0.000000000000000000, 0.000000000000000000, 0.000000000000000000 ) ) ;
#22623 = DIRECTION ( 'NONE',  ( -1.000000000000000000, 0.000000000000000000, -0.000000000000000000 ) ) ;
#22624 = DIRECTION ( 'NONE',  ( -1.000000000000000000, 0.000000000000000000, 0.000000000000000000 ) ) ;
#22625 = CARTESIAN_POINT ( 'NONE',  ( 0.000000000000000000, 0.000000000000000000, 0.000000000000000000 ) ) ;
#22626 = DIRECTION ( 'NONE',  ( 0.000000000000000000, 0.000000000000000000, 1.000000000000000000 ) ) ;
#22627 = LINE ( 'NONE', #38535, #21465 ) ;
#22628 = CIRCLE ( 'NONE', #37484, 82.00000000000000000 ) ;
#22629 = DIRECTION ( 'NONE',  ( -1.000000000000000000, 0.000000000000000000, 0.000000000000000000 ) ) ;
#22630 = DIRECTION ( 'NONE',  ( -1.000000000000000000, 0.000000000000000000, 0.000000000000000000 ) ) ;
#22631 = DIRECTION ( 'NONE',  ( 0.000000000000000000, 0.5877852522924684742, 0.8090169943749507819 ) ) ;
#22632 = ORIENTED_EDGE ( 'NONE', *, *, #4429, .T. ) ;
#22633 = ORIENTED_EDGE ( 'NONE', *, *, #44281, .F. ) ;
#22634 = EDGE_CURVE ( 'NONE', #14425, #14988, #22864, .T. ) ;
#22635 = EDGE_CURVE ( 'NONE', #1236, #16242, #30697, .T. ) ;
#22636 = VERTEX_POINT ( 'NONE', #4286 ) ;
#22637 = EDGE_CURVE ( 'NONE', #1846, #39388, #5757, .T. ) ;
#22638 = ORIENTED_EDGE ( 'NONE', *, *, #23652, .T. ) ;
#22639 = DIRECTION ( 'NONE',  ( 1.000000000000000000, 0.000000000000000000, -0.000000000000000000 ) ) ;
#22640 = ORIENTED_EDGE ( 'NONE', *, *, #28411, .F. ) ;
#22641 = ADVANCED_FACE ( 'NONE', ( #23584, #38530 ), #19911, .F. ) ;
#22642 = CARTESIAN_POINT ( 'NONE',  ( 6.000000000000000000, -71.87247863392443037, 39.47590169984818687 ) ) ;
#22643 = VECTOR ( 'NONE', #33840, 1000.000000000000000 ) ;
#22644 = CYLINDRICAL_SURFACE ( 'NONE', #21873, 77.49899999999999523 ) ;
#22645 = DIRECTION ( 'NONE',  ( -1.000000000000000000, 0.000000000000000000, 0.000000000000000000 ) ) ;
#22646 = AXIS2_PLACEMENT_3D ( 'NONE', #11150, #37817, #4304 ) ;
#22647 = ORIENTED_EDGE ( 'NONE', *, *, #33498, .F. ) ;
#22648 = CYLINDRICAL_SURFACE ( 'NONE', #10974, 16.00000000000000000 ) ;
#22649 = ORIENTED_EDGE ( 'NONE', *, *, #43885, .F. ) ;
#22650 = EDGE_LOOP ( 'NONE', ( #35559, #4816, #17110, #36300 ) ) ;
#22651 = VERTEX_POINT ( 'NONE', #30228 ) ;
#22652 =( GEOMETRIC_REPRESENTATION_CONTEXT ( 3 ) GLOBAL_UNCERTAINTY_ASSIGNED_CONTEXT ( ( #8060 ) ) GLOBAL_UNIT_ASSIGNED_CONTEXT ( ( #31007, #9423, #45926 ) ) REPRESENTATION_CONTEXT ( 'NONE', 'WORKASPACE' ) );
#22653 = EDGE_CURVE ( 'NONE', #4179, #41802, #19195, .T. ) ;
#22654 = ADVANCED_FACE ( 'NONE', ( #16264 ), #31197, .T. ) ;
#22655 = DIRECTION ( 'NONE',  ( 0.000000000000000000, 0.000000000000000000, -1.000000000000000000 ) ) ;
#22656 = CARTESIAN_POINT ( 'NONE',  ( 6.000000000000000000, 29.01471420065563933, 76.69515212746026123 ) ) ;
#22657 = DIRECTION ( 'NONE',  ( -1.000000000000000000, -0.000000000000000000, 0.000000000000000000 ) ) ;
#22658 = ORIENTED_EDGE ( 'NONE', *, *, #21612, .T. ) ;
#22659 = ORIENTED_EDGE ( 'NONE', *, *, #41130, .T. ) ;
#22660 = ORIENTED_EDGE ( 'NONE', *, *, #34204, .F. ) ;
#22661 = VECTOR ( 'NONE', #18389, 1000.000000000000000 ) ;
#22662 = CARTESIAN_POINT ( 'NONE',  ( 10.00000000000000000, -41.91543099594819921, 2.663952781846001816 ) ) ;
#22663 = VERTEX_POINT ( 'NONE', #46117 ) ;
#22664 = DIRECTION ( 'NONE',  ( 0.000000000000000000, -0.3826834323650970537, 0.9238795325112838519 ) ) ;
#22665 = CARTESIAN_POINT ( 'NONE',  ( 0.000000000000000000, 64.81221759200343513, 50.23322058963371006 ) ) ;
#22666 = DIRECTION ( 'NONE',  ( -1.000000000000000000, -0.000000000000000000, 0.000000000000000000 ) ) ;
#22667 = DIRECTION ( 'NONE',  ( -1.000000000000000000, 0.000000000000000000, -0.000000000000000000 ) ) ;
#22668 = DIRECTION ( 'NONE',  ( -1.000000000000000000, 0.000000000000000000, 0.000000000000000000 ) ) ;
#22669 = CARTESIAN_POINT ( 'NONE',  ( 0.000000000000000000, 55.38113227695858143, -54.21277698773617715 ) ) ;
#22670 = CARTESIAN_POINT ( 'NONE',  ( 10.00000000000000000, 51.03279382321088065, 55.19960302592086521 ) ) ;
#22671 = VERTEX_POINT ( 'NONE', #12584 ) ;
#22672 = DIRECTION ( 'NONE',  ( 1.000000000000000000, -0.000000000000000000, 0.000000000000000000 ) ) ;
#22674 = EDGE_CURVE ( 'NONE', #461, #37099, #44038, .T. ) ;
#22673 = LINE ( 'NONE', #11907, #339 ) ;
#22675 = FACE_OUTER_BOUND ( 'NONE', #35145, .T. ) ;
#22676 = ORIENTED_EDGE ( 'NONE', *, *, #13128, .T. ) ;
#22677 = CARTESIAN_POINT ( 'NONE',  ( 11.99999999999999822, 3.894527615419054456, -81.90746397400384637 ) ) ;
#22678 = DIRECTION ( 'NONE',  ( 0.000000000000000000, 0.000000000000000000, -1.000000000000000000 ) ) ;
#22679 = LINE ( 'NONE', #33461, #29034 ) ;
#22680 = CARTESIAN_POINT ( 'NONE',  ( 11.99999999999999822, 0.000000000000000000, 0.000000000000000000 ) ) ;
#22681 = DIRECTION ( 'NONE',  ( -1.000000000000000000, 0.000000000000000000, 0.000000000000000000 ) ) ;
#22682 = CIRCLE ( 'NONE', #1585, 82.00000000000000000 ) ;
#22683 = EDGE_LOOP ( 'NONE', ( #25177, #40324, #39414, #5557 ) ) ;
#22684 = DIRECTION ( 'NONE',  ( -1.000000000000000000, 0.000000000000000000, 0.000000000000000000 ) ) ;
#22685 = DIRECTION ( 'NONE',  ( 0.000000000000000000, 0.8090169943749445647, 0.5877852522924770229 ) ) ;
#22686 = AXIS2_PLACEMENT_3D ( 'NONE', #34088, #26278, #15497 ) ;
#22687 = CIRCLE ( 'NONE', #1590, 82.00000000000000000 ) ;
#22688 = AXIS2_PLACEMENT_3D ( 'NONE', #20295, #31586, #23992 ) ;
#22689 = CARTESIAN_POINT ( 'NONE',  ( -10.00000000000000000, 0.000000000000000000, 0.000000000000000000 ) ) ;
#22690 = CARTESIAN_POINT ( 'NONE',  ( 0.000000000000000000, 0.000000000000000000, 0.000000000000000000 ) ) ;
#22691 = AXIS2_PLACEMENT_3D ( 'NONE', #4951, #20599, #46565 ) ;
#22692 = ORIENTED_EDGE ( 'NONE', *, *, #29201, .T. ) ;
#22693 = VERTEX_POINT ( 'NONE', #23348 ) ;
#22694 = CIRCLE ( 'NONE', #42224, 31.99999999999999289 ) ;
#22695 = EDGE_CURVE ( 'NONE', #32278, #10070, #39375, .T. ) ;
#22696 = AXIS2_PLACEMENT_3D ( 'NONE', #33788, #22784, #34761 ) ;
#22697 = EDGE_CURVE ( 'NONE', #9926, #42385, #39984, .T. ) ;
#22698 = VERTEX_POINT ( 'NONE', #13797 ) ;
#22699 = DIRECTION ( 'NONE',  ( -1.000000000000000000, 0.000000000000000000, 0.000000000000000000 ) ) ;
#22700 = CARTESIAN_POINT ( 'NONE',  ( 0.000000000000000000, 0.000000000000000000, 0.000000000000000000 ) ) ;
#22701 = ORIENTED_EDGE ( 'NONE', *, *, #23060, .T. ) ;
#22702 = ADVANCED_FACE ( 'NONE', ( #13074 ), #28004, .F. ) ;
#22703 = CARTESIAN_POINT ( 'NONE',  ( 0.000000000000000000, 22.90783923731629912, 78.73519480814962890 ) ) ;
#22704 = VERTEX_POINT ( 'NONE', #28230 ) ;
#22705 = VERTEX_POINT ( 'NONE', #28722 ) ;
#22706 = EDGE_CURVE ( 'NONE', #44730, #21962, #12829, .T. ) ;
#22707 = EDGE_CURVE ( 'NONE', #11522, #11877, #1889, .T. ) ;
#22708 = FACE_OUTER_BOUND ( 'NONE', #3940, .T. ) ;
#22709 = LINE ( 'NONE', #33964, #31376 ) ;
#22710 = CIRCLE ( 'NONE', #32870, 82.00000000000000000 ) ;
#22711 = CARTESIAN_POINT ( 'NONE',  ( -23.54415474984308787, -120.4156646670583086, 5.500000000000000000 ) ) ;
#22712 = VECTOR ( 'NONE', #36387, 1000.000000000000000 ) ;
#22713 = DIRECTION ( 'NONE',  ( -1.000000000000000000, 0.000000000000000000, 0.000000000000000000 ) ) ;
#22714 = EDGE_CURVE ( 'NONE', #11938, #3320, #36291, .T. ) ;
#22715 = VERTEX_POINT ( 'NONE', #39506 ) ;
#22716 = ORIENTED_EDGE ( 'NONE', *, *, #40173, .T. ) ;
#22717 = CARTESIAN_POINT ( 'NONE',  ( 10.00000000000000000, 0.000000000000000000, 0.000000000000000000 ) ) ;
#22718 = CIRCLE ( 'NONE', #45389, 16.00000000000000000 ) ;
#22719 = CIRCLE ( 'NONE', #4768, 31.99999999999998579 ) ;
#22720 = PLANE ( 'NONE',  #41668 ) ;
#22721 = CARTESIAN_POINT ( 'NONE',  ( 0.000000000000000000, 22.48208911017500355, 35.47612816024530957 ) ) ;
#22722 = VERTEX_POINT ( 'NONE', #27767 ) ;
#22723 = AXIS2_PLACEMENT_3D ( 'NONE', #24989, #40178, #21314 ) ;
#22724 = EDGE_LOOP ( 'NONE', ( #22692, #28006, #20714, #27904 ) ) ;
#22725 = AXIS2_PLACEMENT_3D ( 'NONE', #7144, #34051, #44585 ) ;
#22726 = CARTESIAN_POINT ( 'NONE',  ( -3.000000000000000000, -20.55727247249726020, -16.78983467731313084 ) ) ;
#22727 = EDGE_CURVE ( 'NONE', #34943, #39901, #27661, .T. ) ;
#22728 = CARTESIAN_POINT ( 'NONE',  ( 11.99999999999999822, 63.18004540533092239, -44.88180994100307686 ) ) ;
#22729 = ORIENTED_EDGE ( 'NONE', *, *, #31372, .F. ) ;
#22730 = VECTOR ( 'NONE', #44467, 1000.000000000000000 ) ;
#22731 = EDGE_LOOP ( 'NONE', ( #149, #21995, #47353, #41332 ) ) ;
#22732 = FACE_OUTER_BOUND ( 'NONE', #37373, .T. ) ;
#22733 = ORIENTED_EDGE ( 'NONE', *, *, #40596, .T. ) ;
#22734 = CARTESIAN_POINT ( 'NONE',  ( 10.00000000000000000, -5.202137450156129717, -37.22597642581163768 ) ) ;
#22735 = FACE_OUTER_BOUND ( 'NONE', #37963, .T. ) ;
#22736 = CYLINDRICAL_SURFACE ( 'NONE', #11832, 42.00000000000000000 ) ;
#22737 = LINE ( 'NONE', #15412, #44073 ) ;
#22738 = CARTESIAN_POINT ( 'NONE',  ( 11.99999999999999822, -8.830959090341869100, -74.65491531819127147 ) ) ;
#22739 = DIRECTION ( 'NONE',  ( -1.000000000000000000, 0.000000000000000000, 0.000000000000000000 ) ) ;
#22740 = CARTESIAN_POINT ( 'NONE',  ( 0.000000000000000000, 14.66109333815564852, -73.73191006444555740 ) ) ;
#22741 = DIRECTION ( 'NONE',  ( -1.000000000000000000, -0.000000000000000000, -0.000000000000000000 ) ) ;
#22742 = DIRECTION ( 'NONE',  ( 0.7585478161175723821, 0.6516173805718057377, 0.000000000000000000 ) ) ;
#22743 = VERTEX_POINT ( 'NONE', #20897 ) ;
#22744 = CARTESIAN_POINT ( 'NONE',  ( 11.99999999999999822, 26.02418014898310261, 70.52718814184268581 ) ) ;
#22745 = CARTESIAN_POINT ( 'NONE',  ( -17.26469406256017791, -140.1601175325492648, 2.500000000000000000 ) ) ;
#22746 = CARTESIAN_POINT ( 'NONE',  ( 18.80329974962065265, -105.8248132807389084, -2.500000000000000000 ) ) ;
#22747 = EDGE_LOOP ( 'NONE', ( #7038, #39397, #33545, #35492 ) ) ;
#22748 = CIRCLE ( 'NONE', #14160, 31.99999999999999289 ) ;
#22749 = UNCERTAINTY_MEASURE_WITH_UNIT (LENGTH_MEASURE( 1.000000000000000082E-05 ), #5662, 'distance_accuracy_value', 'NONE');
#22750 = FACE_OUTER_BOUND ( 'NONE', #12611, .T. ) ;
#22751 = AXIS2_PLACEMENT_3D ( 'NONE', #6121, #35966, #17123 ) ;
#22752 = AXIS2_PLACEMENT_3D ( 'NONE', #9468, #40066, #36389 ) ;
#22753 = EDGE_CURVE ( 'NONE', #42000, #9517, #31589, .T. ) ;
#22754 = FACE_OUTER_BOUND ( 'NONE', #34830, .T. ) ;
#22755 = CARTESIAN_POINT ( 'NONE',  ( 4.999999999999999112, -3.925862922256468046, 41.81611651403860463 ) ) ;
#22756 = EDGE_CURVE ( 'NONE', #15029, #20027, #20643, .T. ) ;
#22757 = ORIENTED_EDGE ( 'NONE', *, *, #47137, .T. ) ;
#22758 = EDGE_CURVE ( 'NONE', #2924, #7777, #16974, .T. ) ;
#22759 = AXIS2_PLACEMENT_3D ( 'NONE', #16361, #31547, #19516 ) ;
#22760 = CIRCLE ( 'NONE', #43871, 11.59999999999999787 ) ;
#22761 = EDGE_CURVE ( 'NONE', #30860, #30648, #30041, .T. ) ;
#22762 = AXIS2_PLACEMENT_3D ( 'NONE', #5046, #42975, #39292 ) ;
#22763 = EDGE_CURVE ( 'NONE', #23501, #46809, #19855, .T. ) ;
#22764 = CYLINDRICAL_SURFACE ( 'NONE', #14874, 42.00000000000000000 ) ;
#22765 = ORIENTED_EDGE ( 'NONE', *, *, #6359, .T. ) ;
#22766 = ORIENTED_EDGE ( 'NONE', *, *, #46913, .F. ) ;
#22767 = VERTEX_POINT ( 'NONE', #46350 ) ;
#22768 = EDGE_LOOP ( 'NONE', ( #513, #14229, #43455, #21732 ) ) ;
#22769 = ORIENTED_EDGE ( 'NONE', *, *, #40301, .F. ) ;
#22770 = DIRECTION ( 'NONE',  ( 0.000000000000000000, -0.4539904997395352027, -0.8910065241883737830 ) ) ;
#22771 = ORIENTED_EDGE ( 'NONE', *, *, #14392, .T. ) ;
#22772 = EDGE_CURVE ( 'NONE', #12014, #31321, #24558, .T. ) ;
#22773 = ORIENTED_EDGE ( 'NONE', *, *, #22596, .F. ) ;
#22774 = FACE_OUTER_BOUND ( 'NONE', #7331, .T. ) ;
#22775 = EDGE_LOOP ( 'NONE', ( #859, #1752, #47674, #2643 ) ) ;
#22776 = FACE_OUTER_BOUND ( 'NONE', #8615, .T. ) ;
#22777 = DIRECTION ( 'NONE',  ( -1.000000000000000000, 0.000000000000000000, 0.000000000000000000 ) ) ;
#22778 = EDGE_LOOP ( 'NONE', ( #41386, #15252, #11275, #32014 ) ) ;
#22779 = ORIENTED_EDGE ( 'NONE', *, *, #40122, .F. ) ;
#22780 = DIRECTION ( 'NONE',  ( -1.000000000000000000, -0.000000000000000000, -0.000000000000000000 ) ) ;
#22781 = DIRECTION ( 'NONE',  ( -1.000000000000000000, 0.000000000000000000, -0.000000000000000000 ) ) ;
#22782 = ORIENTED_EDGE ( 'NONE', *, *, #31918, .T. ) ;
#22783 = AXIS2_PLACEMENT_3D ( 'NONE', #42025, #24366, #19713 ) ;
#22784 = DIRECTION ( 'NONE',  ( 1.000000000000000000, 0.000000000000000000, -0.000000000000000000 ) ) ;
#22785 = ADVANCED_FACE ( 'NONE', ( #28480 ), #9379, .T. ) ;
#22786 = DIRECTION ( 'NONE',  ( 0.000000000000000000, 0.000000000000000000, -1.000000000000000000 ) ) ;
#22787 = VERTEX_POINT ( 'NONE', #36052 ) ;
#22788 = VECTOR ( 'NONE', #37832, 1000.000000000000000 ) ;
#22789 = DIRECTION ( 'NONE',  ( 0.000000000000000000, -0.3826834323650772363, -0.9238795325112919565 ) ) ;
#22790 = VERTEX_POINT ( 'NONE', #2511 ) ;
#22791 = ORIENTED_EDGE ( 'NONE', *, *, #32807, .F. ) ;
#22792 = CARTESIAN_POINT ( 'NONE',  ( 0.000000000000000000, -36.88895765772637247, 6.736453364083436313 ) ) ;
#22793 = CARTESIAN_POINT ( 'NONE',  ( 0.000000000000000000, 0.000000000000000000, 0.000000000000000000 ) ) ;
#22794 = ORIENTED_EDGE ( 'NONE', *, *, #28735, .F. ) ;
#22795 = VECTOR ( 'NONE', #28568, 1000.000000000000114 ) ;
#22796 = DIRECTION ( 'NONE',  ( -1.000000000000000000, -0.000000000000000000, 0.000000000000000000 ) ) ;
#22797 = DIRECTION ( 'NONE',  ( 0.000000000000000000, 0.000000000000000000, 1.000000000000000000 ) ) ;
#22798 = DIRECTION ( 'NONE',  ( -1.000000000000000000, 0.000000000000000000, 0.000000000000000000 ) ) ;
#22799 = CARTESIAN_POINT ( 'NONE',  ( 10.00000000000000000, 26.02418014898310261, 70.52718814184268581 ) ) ;
#22800 = AXIS2_PLACEMENT_3D ( 'NONE', #22450, #37368, #33924 ) ;
#22801 = DIRECTION ( 'NONE',  ( 0.000000000000000000, 0.000000000000000000, 1.000000000000000000 ) ) ;
#22802 = DIRECTION ( 'NONE',  ( 1.000000000000000000, 0.000000000000000000, 0.000000000000000000 ) ) ;
#22803 = EDGE_CURVE ( 'NONE', #37711, #15663, #39249, .T. ) ;
#22804 = ORIENTED_EDGE ( 'NONE', *, *, #38189, .T. ) ;
#22805 = PLANE ( 'NONE',  #26261 ) ;
#22806 = DIRECTION ( 'NONE',  ( 1.000000000000000000, 0.000000000000000000, 0.000000000000000000 ) ) ;
#22807 = CARTESIAN_POINT ( 'NONE',  ( 11.99999999999999822, -26.02418014898359289, 70.52718814184250107 ) ) ;
#22808 = CARTESIAN_POINT ( 'NONE',  ( -235.0000123116479926, -117.0000000000000142, 2.500000000000000000 ) ) ;
#22809 = SHAPE_REPRESENTATION ( 'taper roller bearing_iso_ISO 355-2 - 2BD25 - 22,SI,NC,22', ( #11636 ), #2952 ) ;
#22810 = AXIS2_PLACEMENT_3D ( 'NONE', #26949, #26457, #26698 ) ;
#22811 = LINE ( 'NONE', #7156, #2542 ) ;
#22812 = LINE ( 'NONE', #4466, #30847 ) ;
#22813 = CARTESIAN_POINT ( 'NONE',  ( 11.99999999999999822, -54.21277698773713638, 55.38113227695764351 ) ) ;
#22814 = DIRECTION ( 'NONE',  ( 0.000000000000000000, 0.000000000000000000, 1.000000000000000000 ) ) ;
#22815 = VERTEX_POINT ( 'NONE', #20392 ) ;
#22816 = EDGE_CURVE ( 'NONE', #41422, #5993, #12062, .T. ) ;
#22817 = VERTEX_POINT ( 'NONE', #46607 ) ;
#22818 = DIRECTION ( 'NONE',  ( 0.000000000000000000, 0.8910065241883656784, 0.4539904997395511899 ) ) ;
#22819 = ORIENTED_EDGE ( 'NONE', *, *, #9889, .F. ) ;
#22820 = EDGE_CURVE ( 'NONE', #15589, #46205, #34706, .T. ) ;
#22821 = CARTESIAN_POINT ( 'NONE',  ( 0.000000000000000000, -10.74501242461258244, -35.92658777277521409 ) ) ;
#22822 = APPLICATION_PROTOCOL_DEFINITION ( 'draft international standard', 'automotive_design', 1998, #25696 ) ;
#22823 = EDGE_CURVE ( 'NONE', #13181, #27382, #10344, .T. ) ;
#22824 = CARTESIAN_POINT ( 'NONE',  ( 0.000000000000000000, 0.000000000000000000, 0.000000000000000000 ) ) ;
#22825 = VERTEX_POINT ( 'NONE', #40464 ) ;
#22826 = ADVANCED_FACE ( 'NONE', ( #41192 ), #7646, .T. ) ;
#22827 = AXIS2_PLACEMENT_3D ( 'NONE', #34349, #14576, #29491 ) ;
#22828 = EDGE_CURVE ( 'NONE', #18661, #29809, #22573, .T. ) ;
#22829 = AXIS2_PLACEMENT_3D ( 'NONE', #7960, #48362, #14612 ) ;
#22830 = LINE ( 'NONE', #4479, #20589 ) ;
#22831 = EDGE_LOOP ( 'NONE', ( #27425, #14098, #5572, #34374 ) ) ;
#22832 = AXIS2_PLACEMENT_3D ( 'NONE', #23164, #4562, #34394 ) ;
#22833 = DIRECTION ( 'NONE',  ( -0.000000000000000000, -0.000000000000000000, -1.000000000000000000 ) ) ;
#22834 = CARTESIAN_POINT ( 'NONE',  ( 5.000000000000002665, 40.65526001592612459, 71.21200624218811015 ) ) ;
#22836 = VERTEX_POINT ( 'NONE', #44126 ) ;
#22835 = FACE_OUTER_BOUND ( 'NONE', #27850, .T. ) ;
#22837 = CIRCLE ( 'NONE', #14246, 31.99999999999998934 ) ;
#22838 = ORIENTED_EDGE ( 'NONE', *, *, #26167, .T. ) ;
#22839 = DIRECTION ( 'NONE',  ( 0.000000000000000000, 0.000000000000000000, 1.000000000000000000 ) ) ;
#22840 = DIRECTION ( 'NONE',  ( -1.000000000000000000, 0.000000000000000000, 0.000000000000000000 ) ) ;
#22841 = DIRECTION ( 'NONE',  ( -1.000000000000000000, 0.000000000000000000, -0.000000000000000000 ) ) ;
#22842 = DIRECTION ( 'NONE',  ( 0.000000000000000000, -0.9876883405951393247, 0.1564344650402204329 ) ) ;
#22843 = VERTEX_POINT ( 'NONE', #32624 ) ;
#22844 = DIRECTION ( 'NONE',  ( -1.000000000000000000, -0.000000000000000000, 0.000000000000000000 ) ) ;
#22845 = EDGE_LOOP ( 'NONE', ( #23722, #2650, #2232, #25093 ) ) ;
#22846 = ORIENTED_EDGE ( 'NONE', *, *, #21804, .F. ) ;
#22847 = CARTESIAN_POINT ( 'NONE',  ( 11.99999999999999822, -55.19960302592029677, -51.03279382321147750 ) ) ;
#22848 = AXIS2_PLACEMENT_3D ( 'NONE', #29360, #11968, #45484 ) ;
#22849 = DIRECTION ( 'NONE',  ( 0.000000000000000000, -0.9238795325112821866, -0.3826834323651006065 ) ) ;
#22850 = CARTESIAN_POINT ( 'NONE',  ( 0.000000000000000000, 59.75363087400076267, 56.15606465354979804 ) ) ;
#22851 = FACE_OUTER_BOUND ( 'NONE', #30602, .T. ) ;
#22852 = ORIENTED_EDGE ( 'NONE', *, *, #18329, .F. ) ;
#22853 = DIRECTION ( 'NONE',  ( 0.000000000000000000, 0.000000000000000000, 1.000000000000000000 ) ) ;
#22854 = FACE_OUTER_BOUND ( 'NONE', #21449, .T. ) ;
#22855 = DIRECTION ( 'NONE',  ( -1.000000000000000000, -0.000000000000000000, -0.000000000000000000 ) ) ;
#22856 = CYLINDRICAL_SURFACE ( 'NONE', #24441, 37.49900000000000233 ) ;
#22857 = CYLINDRICAL_SURFACE ( 'NONE', #21548, 31.99999999999998579 ) ;
#22858 = VECTOR ( 'NONE', #9189, 1000.000000000000000 ) ;
#22859 = CARTESIAN_POINT ( 'NONE',  ( 10.00000000000000000, -50.23322058963299241, -64.81221759200398935 ) ) ;
#22860 = DIRECTION ( 'NONE',  ( 0.000000000000000000, -0.5877852522924797984, -0.8090169943749426773 ) ) ;
#22861 = CYLINDRICAL_SURFACE ( 'NONE', #24770, 16.00000000000000000 ) ;
#22862 = VECTOR ( 'NONE', #30867, 1000.000000000000000 ) ;
#22863 = CARTESIAN_POINT ( 'NONE',  ( 0.000000000000000000, -25.88420570971381807, -27.13269053701123212 ) ) ;
#22864 = LINE ( 'NONE', #824, #4184 ) ;
#22865 = AXIS2_PLACEMENT_3D ( 'NONE', #22738, #11004, #48205 ) ;
#22866 = CYLINDRICAL_SURFACE ( 'NONE', #12214, 77.49899999999999523 ) ;
#22867 = CARTESIAN_POINT ( 'NONE',  ( 10.00000000000000000, 80.28980883073757013, 16.65972982744963460 ) ) ;
#22868 = CARTESIAN_POINT ( 'NONE',  ( 0.000000000000000000, 33.80338159004283938, 16.23288003029508886 ) ) ;
#22869 = AXIS2_PLACEMENT_3D ( 'NONE', #14371, #29302, #25848 ) ;
#22870 = CARTESIAN_POINT ( 'NONE',  ( 4.999999999999999112, -3.925862922255855647, -41.81611651403866858 ) ) ;
#22871 = ORIENTED_EDGE ( 'NONE', *, *, #40052, .T. ) ;
#22872 = EDGE_CURVE ( 'NONE', #2440, #46432, #9694, .T. ) ;
#22873 = EDGE_CURVE ( 'NONE', #12321, #1420, #28470, .T. ) ;
#22874 = FACE_OUTER_BOUND ( 'NONE', #46978, .T. ) ;
#22875 = ORIENTED_EDGE ( 'NONE', *, *, #36782, .F. ) ;
#22876 = ADVANCED_FACE ( 'NONE', ( #6687 ), #48032, .T. ) ;
#22877 = EDGE_CURVE ( 'NONE', #9486, #1645, #7352, .T. ) ;
#22878 = ORIENTED_EDGE ( 'NONE', *, *, #39947, .F. ) ;
#22879 = AXIS2_PLACEMENT_3D ( 'NONE', #25914, #40142, #43800 ) ;
#22880 = EDGE_CURVE ( 'NONE', #45199, #42057, #15193, .T. ) ;
#22881 = CYLINDRICAL_SURFACE ( 'NONE', #18726, 16.00000000000000000 ) ;
#22882 = AXIS2_PLACEMENT_3D ( 'NONE', #41665, #4234, #26000 ) ;
#22883 = ORIENTED_EDGE ( 'NONE', *, *, #28892, .F. ) ;
#22884 = AXIS2_PLACEMENT_3D ( 'NONE', #34516, #41894, #38448 ) ;
#22885 = DIRECTION ( 'NONE',  ( -1.000000000000000000, -0.000000000000000000, -0.000000000000000000 ) ) ;
#22886 = CYLINDRICAL_SURFACE ( 'NONE', #10116, 77.49899999999999523 ) ;
#22887 = AXIS2_PLACEMENT_3D ( 'NONE', #45010, #458, #37906 ) ;
#22888 = CARTESIAN_POINT ( 'NONE',  ( 23.11608002360578240, -124.4885236261218182, -2.500000000000000000 ) ) ;
#22889 = ORIENTED_EDGE ( 'NONE', *, *, #35202, .F. ) ;
#22890 = DIRECTION ( 'NONE',  ( 0.000000000000000000, 0.000000000000000000, 1.000000000000000000 ) ) ;
#22891 = AXIS2_PLACEMENT_3D ( 'NONE', #688, #30551, #45475 ) ;
#22892 = ORIENTED_EDGE ( 'NONE', *, *, #41620, .F. ) ;
#22893 = CIRCLE ( 'NONE', #26811, 16.00000000000000000 ) ;
#22894 = ORIENTED_EDGE ( 'NONE', *, *, #5152, .F. ) ;
#22895 = CYLINDRICAL_SURFACE ( 'NONE', #6873, 82.00000000000000000 ) ;
#22896 = CARTESIAN_POINT ( 'NONE',  ( 15.00000000000000000, -10.45096189432314127, 21.10159698893440350 ) ) ;
#22897 = FACE_OUTER_BOUND ( 'NONE', #26699, .T. ) ;
#22898 = ORIENTED_EDGE ( 'NONE', *, *, #33025, .T. ) ;
#22899 = AXIS2_PLACEMENT_3D ( 'NONE', #29482, #44412, #10880 ) ;
#22900 = ORIENTED_EDGE ( 'NONE', *, *, #14034, .F. ) ;
#22901 = ORIENTED_EDGE ( 'NONE', *, *, #21379, .F. ) ;
#22902 = CARTESIAN_POINT ( 'NONE',  ( 10.00000000000000000, -75.11764819372145041, -2.946379043147127064 ) ) ;
#22903 = ORIENTED_EDGE ( 'NONE', *, *, #14929, .T. ) ;
#22904 = LINE ( 'NONE', #37839, #34747 ) ;
#22905 = DIRECTION ( 'NONE',  ( 0.000000000000000000, 0.5224985647159440250, 0.8526401643540951758 ) ) ;
#22906 = DIRECTION ( 'NONE',  ( 1.000000000000000000, -0.000000000000000000, -0.000000000000000000 ) ) ;
#22907 = DIRECTION ( 'NONE',  ( 0.000000000000000000, 0.000000000000000000, -1.000000000000000000 ) ) ;
#22908 = CARTESIAN_POINT ( 'NONE',  ( 11.99999999999999822, 63.97538442413427617, 51.29473840253247374 ) ) ;
#22909 = LINE ( 'NONE', #33209, #14335 ) ;
#22910 = DIRECTION ( 'NONE',  ( 0.000000000000000000, 0.000000000000000000, 1.000000000000000000 ) ) ;
#22911 = FACE_OUTER_BOUND ( 'NONE', #22055, .T. ) ;
#22912 = VERTEX_POINT ( 'NONE', #36535 ) ;
#22913 = DIRECTION ( 'NONE',  ( 0.000000000000000000, 0.4539904997395413644, 0.8910065241883706744 ) ) ;
#22914 = EDGE_CURVE ( 'NONE', #38308, #3813, #28943, .T. ) ;
#22915 = ORIENTED_EDGE ( 'NONE', *, *, #6457, .T. ) ;
#22916 = VERTEX_POINT ( 'NONE', #7407 ) ;
#22917 = CARTESIAN_POINT ( 'NONE',  ( 5.000000000000002665, 22.90783923731741112, -78.73519480814930205 ) ) ;
#22918 = ADVANCED_FACE ( 'NONE', ( #33581 ), #3728, .T. ) ;
#22919 = CYLINDRICAL_SURFACE ( 'NONE', #23053, 31.99999999999998579 ) ;
#22920 = DIRECTION ( 'NONE',  ( -1.000000000000000000, 0.000000000000000000, 0.000000000000000000 ) ) ;
#22921 = VECTOR ( 'NONE', #47970, 1000.000000000000114 ) ;
#22922 = CARTESIAN_POINT ( 'NONE',  ( 10.00000000000000000, 24.73286445877703699, 73.44644590900070114 ) ) ;
#22923 = EDGE_CURVE ( 'NONE', #10549, #8725, #17921, .T. ) ;
#22924 = DIRECTION ( 'NONE',  ( 0.000000000000000000, 0.000000000000000000, 1.000000000000000000 ) ) ;
#22926 = VECTOR ( 'NONE', #43535, 1000.000000000000000 ) ;
#22925 = DIRECTION ( 'NONE',  ( -1.000000000000000000, 0.000000000000000000, -0.000000000000000000 ) ) ;
#22927 = CARTESIAN_POINT ( 'NONE',  ( 0.000000000000000000, 49.70050353004889132, 59.46389618801982380 ) ) ;
#22928 = CARTESIAN_POINT ( 'NONE',  ( 10.00000000000000000, 54.21277698773675979, 55.38113227695801299 ) ) ;
#22929 = AXIS2_PLACEMENT_3D ( 'NONE', #19701, #16301, #16537 ) ;
#22930 = AXIS2_PLACEMENT_3D ( 'NONE', #13993, #10312, #11538 ) ;
#22931 = AXIS2_PLACEMENT_3D ( 'NONE', #21961, #36885, #48161 ) ;
#22932 = EDGE_CURVE ( 'NONE', #42951, #19820, #14389, .T. ) ;
#22933 =( LENGTH_UNIT ( ) NAMED_UNIT ( * ) SI_UNIT ( .MILLI., .METRE. ) );
#22934 = CIRCLE ( 'NONE', #24509, 37.49900000000000233 ) ;
#22935 = CARTESIAN_POINT ( 'NONE',  ( 0.000000000000000000, -120.0000000000000000, 125.0000000000000000 ) ) ;
#22936 = ADVANCED_FACE ( 'NONE', ( #29440 ), #33348, .T. ) ;
#22937 = EDGE_CURVE ( 'NONE', #36554, #7777, #3428, .T. ) ;
#22938 = VERTEX_POINT ( 'NONE', #37262 ) ;
#22939 = AXIS2_PLACEMENT_3D ( 'NONE', #9824, #39707, #27720 ) ;
#22940 = AXIS2_PLACEMENT_3D ( 'NONE', #38283, #27038, #45377 ) ;
#22941 = AXIS2_PLACEMENT_3D ( 'NONE', #21343, #36280, #2745 ) ;
#22942 = VECTOR ( 'NONE', #18893, 1000.000000000000000 ) ;
#22943 = CARTESIAN_POINT ( 'NONE',  ( 11.99999999999999822, -75.54627589209955829, 17.28742895386058009 ) ) ;
#22944 = CARTESIAN_POINT ( 'NONE',  ( 12.00000000000000000, 23.49999999999999645, -1.500000000000003997 ) ) ;
#22945 = ORIENTED_EDGE ( 'NONE', *, *, #43826, .T. ) ;
#22946 = AXIS2_PLACEMENT_3D ( 'NONE', #26196, #15900, #11272 ) ;
#22947 = ADVANCED_FACE ( 'NONE', ( #10604 ), #11077, .T. ) ;
#22948 = ORIENTED_EDGE ( 'NONE', *, *, #2641, .T. ) ;
#22949 = CARTESIAN_POINT ( 'NONE',  ( 10.00000000000000000, -26.02418014898359289, 70.52718814184250107 ) ) ;
#22950 = ORIENTED_EDGE ( 'NONE', *, *, #45166, .F. ) ;
#22951 = VERTEX_POINT ( 'NONE', #29912 ) ;
#22952 = AXIS2_PLACEMENT_3D ( 'NONE', #12836, #20648, #35586 ) ;
#22953 = CYLINDRICAL_SURFACE ( 'NONE', #46848, 77.49899999999999523 ) ;
#22954 = DIRECTION ( 'NONE',  ( -1.000000000000000000, 0.000000000000000000, 0.000000000000000000 ) ) ;
#22955 = CARTESIAN_POINT ( 'NONE',  ( 9.984461079971730157, -95.40710393340120277, 2.500000000000000000 ) ) ;
#22956 = ORIENTED_EDGE ( 'NONE', *, *, #27770, .F. ) ;
#22957 = CARTESIAN_POINT ( 'NONE',  ( 10.00000000000000000, 0.000000000000000000, 0.000000000000000000 ) ) ;
#22958 = ORIENTED_EDGE ( 'NONE', *, *, #27583, .T. ) ;
#22959 = ORIENTED_EDGE ( 'NONE', *, *, #42830, .F. ) ;
#22960 = LINE ( 'NONE', #12208, #4850 ) ;
#22961 = AXIS2_PLACEMENT_3D ( 'NONE', #32438, #2802, #17737 ) ;
#22962 = VECTOR ( 'NONE', #19699, 1000.000000000000000 ) ;
#22963 = AXIS2_PLACEMENT_3D ( 'NONE', #33412, #37326, #33638 ) ;
#22964 = DIRECTION ( 'NONE',  ( 0.000000000000000000, 0.000000000000000000, 1.000000000000000000 ) ) ;
#22965 = CARTESIAN_POINT ( 'NONE',  ( 0.000000000000000000, 0.000000000000000000, 0.000000000000000000 ) ) ;
#22966 = ORIENTED_EDGE ( 'NONE', *, *, #9750, .T. ) ;
#22967 = ORIENTED_EDGE ( 'NONE', *, *, #18669, .F. ) ;
#22968 = DIRECTION ( 'NONE',  ( 0.000000000000000000, 0.000000000000000000, 1.000000000000000000 ) ) ;
#22969 = EDGE_CURVE ( 'NONE', #6182, #40126, #26897, .T. ) ;
#22970 = CIRCLE ( 'NONE', #45646, 77.49899999999999523 ) ;
#22971 = AXIS2_PLACEMENT_3D ( 'NONE', #2763, #17696, #47546 ) ;
#22972 = ORIENTED_EDGE ( 'NONE', *, *, #46816, .T. ) ;
#22973 = EDGE_LOOP ( 'NONE', ( #5109, #24348, #34028, #13201 ) ) ;
#22974 = AXIS2_PLACEMENT_3D ( 'NONE', #30338, #11499, #3898 ) ;
#22975 = LINE ( 'NONE', #4140, #4863 ) ;
#22976 = ORIENTED_EDGE ( 'NONE', *, *, #14915, .T. ) ;
#22977 = AXIS2_PLACEMENT_3D ( 'NONE', #48221, #14701, #10058 ) ;
#22978 = DIRECTION ( 'NONE',  ( -1.000000000000000000, 0.000000000000000000, 0.000000000000000000 ) ) ;
#22979 = EDGE_CURVE ( 'NONE', #20870, #47247, #33139, .T. ) ;
#22980 = CARTESIAN_POINT ( 'NONE',  ( 0.000000000000000000, -8.840884882374576037, -74.65374052328658649 ) ) ;
#22981 = CARTESIAN_POINT ( 'NONE',  ( 10.00000000000000000, -10.96151621346461447, -35.95386929396268272 ) ) ;
#22982 = CYLINDRICAL_SURFACE ( 'NONE', #23784, 31.99999999999998579 ) ;
#22983 = CYLINDRICAL_SURFACE ( 'NONE', #22865, 31.99999999999998579 ) ;
#22984 = CARTESIAN_POINT ( 'NONE',  ( 11.99999999999999822, -75.11764819372145041, -2.946379043147127064 ) ) ;
#22985 = EDGE_CURVE ( 'NONE', #21783, #43334, #21393, .T. ) ;
#22986 = CIRCLE ( 'NONE', #23744, 17.37152077436032371 ) ;
#22987 = DIRECTION ( 'NONE',  ( 0.000000000000000000, 0.000000000000000000, 1.000000000000000000 ) ) ;
#22988 = CYLINDRICAL_SURFACE ( 'NONE', #45832, 31.99999999999998579 ) ;
#22989 = CYLINDRICAL_SURFACE ( 'NONE', #19180, 42.00000000000000000 ) ;
#22990 = ORIENTED_EDGE ( 'NONE', *, *, #27129, .T. ) ;
#22991 = DIRECTION ( 'NONE',  ( 1.000000000000000000, 0.000000000000000000, 0.000000000000000000 ) ) ;
#22992 = LINE ( 'NONE', #35388, #30891 ) ;
#22993 =( LENGTH_UNIT ( ) NAMED_UNIT ( * ) SI_UNIT ( .MILLI., .METRE. ) );
#22994 = DIRECTION ( 'NONE',  ( 0.000000000000000000, -0.3826834323650774583, -0.9238795325112919565 ) ) ;
#22995 = EDGE_CURVE ( 'NONE', #36805, #21677, #43317, .T. ) ;
#22996 = EDGE_CURVE ( 'NONE', #6721, #43680, #8921, .T. ) ;
#22997 = ORIENTED_EDGE ( 'NONE', *, *, #5938, .T. ) ;
#22998 = VECTOR ( 'NONE', #48201, 1000.000000000000000 ) ;
#22999 = DIRECTION ( 'NONE',  ( -1.000000000000000000, 0.000000000000000000, 0.000000000000000000 ) ) ;
#23000 = AXIS2_PLACEMENT_3D ( 'NONE', #28460, #13784, #32144 ) ;
#23001 = AXIS2_PLACEMENT_3D ( 'NONE', #33881, #26785, #34596 ) ;
#23002 = AXIS2_PLACEMENT_3D ( 'NONE', #46089, #4961, #31415 ) ;
#23003 = CARTESIAN_POINT ( 'NONE',  ( 0.000000000000000000, -2.543863470247813119, -81.96053171279905314 ) ) ;
#23004 = CARTESIAN_POINT ( 'NONE',  ( -10.00000000000000000, 0.000000000000000000, 0.000000000000000000 ) ) ;
#23005 = ORIENTED_EDGE ( 'NONE', *, *, #35938, .T. ) ;
#23006 = ADVANCED_FACE ( 'NONE', ( #8833 ), #37500, .T. ) ;
#23007 = EDGE_LOOP ( 'NONE', ( #10174, #30224, #1782, #125 ) ) ;
#23008 = AXIS2_PLACEMENT_3D ( 'NONE', #240, #27353, #29869 ) ;
#23009 = VECTOR ( 'NONE', #36940, 1000.000000000000000 ) ;
#23010 = AXIS2_PLACEMENT_3D ( 'NONE', #11449, #7754, #26365 ) ;
#23011 = DIRECTION ( 'NONE',  ( 0.000000000000000000, 0.000000000000000000, 1.000000000000000000 ) ) ;
#23012 = VECTOR ( 'NONE', #17580, 1000.000000000000000 ) ;
#23013 = ORIENTED_EDGE ( 'NONE', *, *, #27422, .F. ) ;
#23014 = ORIENTED_EDGE ( 'NONE', *, *, #12001, .F. ) ;
#23015 = ORIENTED_EDGE ( 'NONE', *, *, #20353, .T. ) ;
#23016 = AXIS2_PLACEMENT_3D ( 'NONE', #26356, #33213, #37848 ) ;
#23017 = CARTESIAN_POINT ( 'NONE',  ( 0.000000000000000000, 71.91182617369230456, -28.89263327155667938 ) ) ;
#23018 = EDGE_LOOP ( 'NONE', ( #35098, #4079, #30244, #1229 ) ) ;
#23019 = ORIENTED_EDGE ( 'NONE', *, *, #38911, .F. ) ;
#23020 = VERTEX_POINT ( 'NONE', #27458 ) ;
#23021 = CARTESIAN_POINT ( 'NONE',  ( 0.000000000000000000, 0.000000000000000000, 0.000000000000000000 ) ) ;
#23022 = ORIENTED_EDGE ( 'NONE', *, *, #24868, .T. ) ;
#23023 = DIRECTION ( 'NONE',  ( -1.000000000000000000, -0.000000000000000000, -0.000000000000000000 ) ) ;
#23024 = CARTESIAN_POINT ( 'NONE',  ( 10.00000000000000000, -29.01471420065617224, 76.69515212746006227 ) ) ;
#23025 = ORIENTED_EDGE ( 'NONE', *, *, #10172, .T. ) ;
#23026 = CARTESIAN_POINT ( 'NONE',  ( 10.00000000000000000, -35.53030884539077050, -12.26510123303296851 ) ) ;
#23027 = VERTEX_POINT ( 'NONE', #15959 ) ;
#23029 = ORIENTED_EDGE ( 'NONE', *, *, #8493, .T. ) ;
#23028 = DIRECTION ( 'NONE',  ( -1.000000000000000000, 0.000000000000000000, 0.000000000000000000 ) ) ;
#23030 = DIRECTION ( 'NONE',  ( 0.000000000000000000, -0.3090169943749471737, 0.9510565162951537532 ) ) ;
#23031 = EDGE_LOOP ( 'NONE', ( #2470, #18949, #35349, #24737 ) ) ;
#23032 = CYLINDRICAL_SURFACE ( 'NONE', #16240, 77.49899999999999523 ) ;
#23033 = EDGE_LOOP ( 'NONE', ( #18531, #41483, #46018, #36961 ) ) ;
#23034 = VERTEX_POINT ( 'NONE', #8121 ) ;
#23035 = DIRECTION ( 'NONE',  ( -1.000000000000000000, 0.000000000000000000, 0.000000000000000000 ) ) ;
#23036 = AXIS2_PLACEMENT_3D ( 'NONE', #37580, #44930, #617 ) ;
#23037 = DIRECTION ( 'NONE',  ( 0.000000000000000000, 0.000000000000000000, 1.000000000000000000 ) ) ;
#23038 = EDGE_CURVE ( 'NONE', #14224, #5001, #23298, .T. ) ;
#23039 = LINE ( 'NONE', #996, #40962 ) ;
#23040 = CARTESIAN_POINT ( 'NONE',  ( 21.85433023846371370, -135.0628101570779620, -5.500000000000000000 ) ) ;
#23041 = DIRECTION ( 'NONE',  ( -1.000000000000000000, 0.000000000000000000, 0.000000000000000000 ) ) ;
#23042 = EDGE_CURVE ( 'NONE', #6278, #45279, #22812, .T. ) ;
#23043 = CARTESIAN_POINT ( 'NONE',  ( 5.000000000000002665, -2.543863470248944214, 81.96053171279901051 ) ) ;
#23044 = ADVANCED_FACE ( 'NONE', ( #543 ), #12527, .F. ) ;
#23045 = DIRECTION ( 'NONE',  ( -1.000000000000000000, -0.000000000000000000, -0.000000000000000000 ) ) ;
#23046 = CYLINDRICAL_SURFACE ( 'NONE', #38049, 31.99999999999999289 ) ;
#23047 = ORIENTED_EDGE ( 'NONE', *, *, #31299, .F. ) ;
#23048 = AXIS2_PLACEMENT_3D ( 'NONE', #4159, #27836, #44780 ) ;
#23049 = CYLINDRICAL_SURFACE ( 'NONE', #24683, 37.49900000000000233 ) ;
#23050 = ADVANCED_FACE ( 'NONE', ( #27220 ), #11568, .T. ) ;
#23051 = LINE ( 'NONE', #30404, #592 ) ;
#23053 = AXIS2_PLACEMENT_3D ( 'NONE', #1131, #13305, #42248 ) ;
#23052 = FACE_OUTER_BOUND ( 'NONE', #29675, .T. ) ;
#23054 = CIRCLE ( 'NONE', #4303, 42.00000000000000000 ) ;
#23055 = CARTESIAN_POINT ( 'NONE',  ( 0.000000000000000000, -51.29473840253177030, -63.97538442413482329 ) ) ;
#23056 = CARTESIAN_POINT ( 'NONE',  ( -2.500000000000000000, 16.00000000000000000, -19.01812422950394676 ) ) ;
#23057 = CARTESIAN_POINT ( 'NONE',  ( 11.99999999999999822, 17.28742895386084655, 75.54627589209950145 ) ) ;
#23058 = DIRECTION ( 'NONE',  ( -1.000000000000000000, -0.000000000000000000, -0.000000000000000000 ) ) ;
#23059 = CIRCLE ( 'NONE', #12139, 82.00000000000000000 ) ;
#23060 = EDGE_CURVE ( 'NONE', #23124, #10502, #41019, .T. ) ;
#23061 = FACE_BOUND ( 'NONE', #25820, .T. ) ;
#23062 = VERTEX_POINT ( 'NONE', #41419 ) ;
#23063 = EDGE_CURVE ( 'NONE', #36193, #22222, #37867, .T. ) ;
#23064 = CARTESIAN_POINT ( 'NONE',  ( 10.00000000000000000, 14.66109333815460225, 73.73191006444577056 ) ) ;
#23065 = APPLICATION_PROTOCOL_DEFINITION ( 'draft international standard', 'automotive_design', 1998, #29133 ) ;
#23066 = LINE ( 'NONE', #7654, #22942 ) ;
#23067 = VERTEX_POINT ( 'NONE', #26730 ) ;
#23068 = EDGE_CURVE ( 'NONE', #46997, #908, #37991, .T. ) ;
#23069 = AXIS2_PLACEMENT_3D ( 'NONE', #32031, #29965, #24675 ) ;
#23070 = AXIS2_PLACEMENT_3D ( 'NONE', #28983, #47817, #47582 ) ;
#23071 = VERTEX_POINT ( 'NONE', #4223 ) ;
#23072 = DIRECTION ( 'NONE',  ( 0.000000000000000000, 0.8660254037844432595, -0.4999999999999919509 ) ) ;
#23073 = ORIENTED_EDGE ( 'NONE', *, *, #20827, .F. ) ;
#23074 = EDGE_CURVE ( 'NONE', #26344, #24460, #766, .T. ) ;
#23075 = VECTOR ( 'NONE', #4540, 999.9999999999998863 ) ;
#23076 = CIRCLE ( 'NONE', #12925, 42.00000000000000000 ) ;
#23077 = DIRECTION ( 'NONE',  ( -1.000000000000000000, 0.000000000000000000, 0.000000000000000000 ) ) ;
#23078 = DIRECTION ( 'NONE',  ( 0.000000000000000000, 0.000000000000000000, 1.000000000000000000 ) ) ;
#23079 = CARTESIAN_POINT ( 'NONE',  ( 0.000000000000000000, 46.21855187248719687, -62.20884554313968806 ) ) ;
#23080 = ORIENTED_EDGE ( 'NONE', *, *, #27000, .T. ) ;
#23081 = VECTOR ( 'NONE', #28390, 1000.000000000000000 ) ;
#23082 = ORIENTED_EDGE ( 'NONE', *, *, #17025, .F. ) ;
#23083 = CIRCLE ( 'NONE', #19932, 31.99999999999998934 ) ;
#23084 = AXIS2_PLACEMENT_3D ( 'NONE', #15928, #31107, #30866 ) ;
#23085 = CYLINDRICAL_SURFACE ( 'NONE', #23128, 42.00000000000000000 ) ;
#23086 = DIRECTION ( 'NONE',  ( 0.000000000000000000, 0.000000000000000000, 1.000000000000000000 ) ) ;
#23087 = CARTESIAN_POINT ( 'NONE',  ( 0.000000000000000000, -59.03342792756231461, -46.54456581323868392 ) ) ;
#23089 = VERTEX_POINT ( 'NONE', #42141 ) ;
#23088 = DIRECTION ( 'NONE',  ( 0.000000000000000000, 0.6691306063588661202, 0.7431448254773871387 ) ) ;
#23090 = AXIS2_PLACEMENT_3D ( 'NONE', #39979, #21609, #24561 ) ;
#23091 = ORIENTED_EDGE ( 'NONE', *, *, #19000, .T. ) ;
#23092 = DIRECTION ( 'NONE',  ( -1.000000000000000000, 0.000000000000000000, -0.000000000000000000 ) ) ;
#23093 = EDGE_LOOP ( 'NONE', ( #25310, #12968, #35418, #8757 ) ) ;
#23094 = EDGE_LOOP ( 'NONE', ( #38566, #25976, #35215, #36153 ) ) ;
#23095 = ADVANCED_FACE ( 'NONE', ( #34297 ), #12054, .T. ) ;
#23096 = FACE_OUTER_BOUND ( 'NONE', #1536, .T. ) ;
#23097 = EDGE_CURVE ( 'NONE', #22705, #33441, #26984, .T. ) ;
#23098 = DIRECTION ( 'NONE',  ( -1.000000000000000000, 0.000000000000000000, 0.000000000000000000 ) ) ;
#23099 = CIRCLE ( 'NONE', #4354, 31.99999999999999289 ) ;
#23100 = FACE_OUTER_BOUND ( 'NONE', #12940, .T. ) ;
#23101 = CARTESIAN_POINT ( 'NONE',  ( 11.99999999999999822, 68.27212725128275395, 31.46837873495001503 ) ) ;
#23102 = ORIENTED_EDGE ( 'NONE', *, *, #30777, .T. ) ;
#23103 = PLANE ( 'NONE',  #29987 ) ;
#23104 = DIRECTION ( 'NONE',  ( -1.000000000000000000, 0.000000000000000000, -0.000000000000000000 ) ) ;
#23105 = EDGE_CURVE ( 'NONE', #48222, #29618, #3478, .T. ) ;
#23106 = CYLINDRICAL_SURFACE ( 'NONE', #36019, 31.99999999999998579 ) ;
#23107 = DIRECTION ( 'NONE',  ( -1.000000000000000000, 0.000000000000000000, 0.000000000000000000 ) ) ;
#23108 = AXIS2_PLACEMENT_3D ( 'NONE', #9145, #5243, #36045 ) ;
#23109 = FACE_BOUND ( 'NONE', #26708, .T. ) ;
#23110 = FACE_OUTER_BOUND ( 'NONE', #28343, .T. ) ;
#23112 = ADVANCED_FACE ( 'NONE', ( #9553 ), #28404, .T. ) ;
#23111 = DIRECTION ( 'NONE',  ( -0.000000000000000000, 0.8090169943749491166, 0.5877852522924709167 ) ) ;
#23113 = DIRECTION ( 'NONE',  ( 0.000000000000000000, 0.000000000000000000, 1.000000000000000000 ) ) ;
#23114 = FACE_OUTER_BOUND ( 'NONE', #35696, .T. ) ;
#23115 = DIRECTION ( 'NONE',  ( -1.000000000000000000, -0.000000000000000000, -0.000000000000000000 ) ) ;
#23116 = FACE_OUTER_BOUND ( 'NONE', #9583, .T. ) ;
#23117 = VECTOR ( 'NONE', #3133, 1000.000000000000000 ) ;
#23118 = CARTESIAN_POINT ( 'NONE',  ( -25.50183398199384754, -112.6408924756582053, 5.500000000000000000 ) ) ;
#23119 = LINE ( 'NONE', #45157, #47972 ) ;
#23120 = FACE_OUTER_BOUND ( 'NONE', #11428, .T. ) ;
#23121 = AXIS2_PLACEMENT_3D ( 'NONE', #32668, #6733, #21659 ) ;
#23122 = FACE_OUTER_BOUND ( 'NONE', #46102, .T. ) ;
#23123 = AXIS2_PLACEMENT_3D ( 'NONE', #8881, #23821, #35070 ) ;
#23124 = VERTEX_POINT ( 'NONE', #13020 ) ;
#23125 = CLOSED_SHELL ( 'NONE', ( #21429, #23006, #6466, #45957, #41020, #21979 ) ) ;
#23126 = ORIENTED_EDGE ( 'NONE', *, *, #10123, .T. ) ;
#23127 = ORIENTED_EDGE ( 'NONE', *, *, #24369, .F. ) ;
#23128 = AXIS2_PLACEMENT_3D ( 'NONE', #37526, #15503, #11830 ) ;
#23129 = ORIENTED_EDGE ( 'NONE', *, *, #25291, .F. ) ;
#23130 = CARTESIAN_POINT ( 'NONE',  ( 0.000000000000000000, 16.45098606841126454, 33.79645857604518966 ) ) ;
#23131 = AXIS2_PLACEMENT_3D ( 'NONE', #4962, #46090, #4720 ) ;
#23132 = ORIENTED_EDGE ( 'NONE', *, *, #140, .T. ) ;
#23133 = VECTOR ( 'NONE', #45550, 1000.000000000000000 ) ;
#23134 = CARTESIAN_POINT ( 'NONE',  ( 0.000000000000000000, 33.17418723428333749, -17.67226234102790272 ) ) ;
#23135 = ORIENTED_EDGE ( 'NONE', *, *, #33706, .F. ) ;
#23136 = CARTESIAN_POINT ( 'NONE',  ( -23.54415474984308787, -120.4156646670583086, 5.500000000000000000 ) ) ;
#23137 = FACE_OUTER_BOUND ( 'NONE', #17060, .T. ) ;
#23138 = VERTEX_POINT ( 'NONE', #13731 ) ;
#23139 = LINE ( 'NONE', #15329, #3129 ) ;
#23140 = VERTEX_POINT ( 'NONE', #2224 ) ;
#23141 = CIRCLE ( 'NONE', #36421, 31.99999999999998579 ) ;
#23142 = ORIENTED_EDGE ( 'NONE', *, *, #18913, .F. ) ;
#23143 = CARTESIAN_POINT ( 'NONE',  ( 0.000000000000000000, -74.65374052328644439, -8.840884882375878107 ) ) ;
#23144 = CYLINDRICAL_SURFACE ( 'NONE', #1697, 31.99999999999998579 ) ;
#23145 = CIRCLE ( 'NONE', #40382, 82.00000000000000000 ) ;
#23146 = ORIENTED_EDGE ( 'NONE', *, *, #26399, .T. ) ;
#23147 = VERTEX_POINT ( 'NONE', #31384 ) ;
#23148 = DIRECTION ( 'NONE',  ( 1.000000000000000000, 0.000000000000000000, 0.000000000000000000 ) ) ;
#23149 = ORIENTED_EDGE ( 'NONE', *, *, #14151, .F. ) ;
#23150 = EDGE_CURVE ( 'NONE', #40126, #32923, #6584, .T. ) ;
#23151 = DIRECTION ( 'NONE',  ( 0.000000000000000000, 0.000000000000000000, 1.000000000000000000 ) ) ;
#23152 = AXIS2_PLACEMENT_3D ( 'NONE', #28930, #40214, #39976 ) ;
#23153 = DIRECTION ( 'NONE',  ( 0.000000000000000000, 0.8526401643540935105, -0.5224985647159466895 ) ) ;
#23154 = DIRECTION ( 'NONE',  ( 0.000000000000000000, -0.4539904997395350361, -0.8910065241883738940 ) ) ;
#23155 = CARTESIAN_POINT ( 'NONE',  ( 4.999999999999999112, 40.98264845739763018, -9.188173127306860977 ) ) ;
#23156 = DIRECTION ( 'NONE',  ( -1.000000000000000000, 0.000000000000000000, 0.000000000000000000 ) ) ;
#23157 = EDGE_CURVE ( 'NONE', #47105, #6091, #37087, .T. ) ;
#23158 = LINE ( 'NONE', #12873, #37778 ) ;
#23159 = CARTESIAN_POINT ( 'NONE',  ( -10.00000000000000000, 0.000000000000000000, 0.000000000000000000 ) ) ;
#23160 = VERTEX_POINT ( 'NONE', #9095 ) ;
#23161 = DIRECTION ( 'NONE',  ( 0.000000000000000000, 0.000000000000000000, 1.000000000000000000 ) ) ;
#23162 = DIRECTION ( 'NONE',  ( 0.000000000000000000, -0.7431448254773878048, 0.6691306063588654540 ) ) ;
#23163 = EDGE_LOOP ( 'NONE', ( #12138, #20678, #24604, #24055 ) ) ;
#23164 = CARTESIAN_POINT ( 'NONE',  ( 0.000000000000000000, -65.58780272294100655, 36.73666225445870737 ) ) ;
#23165 = DIRECTION ( 'NONE',  ( 0.000000000000000000, 0.000000000000000000, 1.000000000000000000 ) ) ;
#23166 = VERTEX_POINT ( 'NONE', #46786 ) ;
#23167 = VERTEX_POINT ( 'NONE', #20830 ) ;
#23169 = ADVANCED_FACE ( 'NONE', ( #5661 ), #34737, .T. ) ;
#23168 = DIRECTION ( 'NONE',  ( 0.000000000000000000, -0.9945218953682742891, -0.1045284632676436315 ) ) ;
#23170 = CARTESIAN_POINT ( 'NONE',  ( -7.670864526094549163, -97.73662565058241114, 5.500000000000000000 ) ) ;
#23171 = VECTOR ( 'NONE', #18416, 1000.000000000000114 ) ;
#23172 = EDGE_CURVE ( 'NONE', #26733, #19547, #20329, .T. ) ;
#23173 = CARTESIAN_POINT ( 'NONE',  ( 10.00000000000000000, 0.000000000000000000, 0.000000000000000000 ) ) ;
#23174 = LINE ( 'NONE', #30761, #3383 ) ;
#23175 = AXIS2_PLACEMENT_3D ( 'NONE', #34269, #38438, #12991 ) ;
#23176 = SURFACE_SIDE_STYLE ('',( #12179 ) ) ;
#23177 = DIRECTION ( 'NONE',  ( 0.000000000000000000, 0.9723699203976773342, -0.2334453638559024491 ) ) ;
#23178 = AXIS2_PLACEMENT_3D ( 'NONE', #42081, #38403, #44776 ) ;
#23179 = CARTESIAN_POINT ( 'NONE',  ( 11.99999999999999822, 0.000000000000000000, 0.000000000000000000 ) ) ;
#23180 = LINE ( 'NONE', #12648, #2919 ) ;
#23181 = FACE_OUTER_BOUND ( 'NONE', #21575, .T. ) ;
#23182 = ORIENTED_EDGE ( 'NONE', *, *, #42134, .T. ) ;
#23183 = CIRCLE ( 'NONE', #45877, 16.00000000000000000 ) ;
#23184 = ORIENTED_EDGE ( 'NONE', *, *, #26386, .F. ) ;
#23185 = ORIENTED_EDGE ( 'NONE', *, *, #47665, .T. ) ;
#23186 = CIRCLE ( 'NONE', #45882, 77.49899999999999523 ) ;
#23187 = CYLINDRICAL_SURFACE ( 'NONE', #3049, 42.00000000000000000 ) ;
#23188 = DIRECTION ( 'NONE',  ( -0.4279312458752990711, -0.9038112904824846527, 0.000000000000000000 ) ) ;
#23189 = ORIENTED_EDGE ( 'NONE', *, *, #19450, .T. ) ;
#23190 = EDGE_CURVE ( 'NONE', #3822, #38262, #20574, .T. ) ;
#23191 = VECTOR ( 'NONE', #16139, 1000.000000000000000 ) ;
#23192 = DIRECTION ( 'NONE',  ( 1.000000000000000000, 0.000000000000000000, 0.000000000000000000 ) ) ;
#23193 = EDGE_CURVE ( 'NONE', #46188, #47238, #38962, .T. ) ;
#23194 = ORIENTED_EDGE ( 'NONE', *, *, #4046, .F. ) ;
#23195 = VERTEX_POINT ( 'NONE', #46544 ) ;
#23196 = CIRCLE ( 'NONE', #36473, 42.00000000000000000 ) ;
#23197 = EDGE_CURVE ( 'NONE', #25587, #1295, #19885, .T. ) ;
#23198 = DIRECTION ( 'NONE',  ( -1.000000000000000000, 0.000000000000000000, -0.000000000000000000 ) ) ;
#23200 = EDGE_LOOP ( 'NONE', ( #21583, #30542, #11893, #43718, #21306, #1199, #6825, #21903, #44371, #24806, #32483, #986, #21203, #60, #27418, #1578, #34861, #31707, #19268, #10121, #35373, #46253, #2715, #33037, #760, #28118, #24174, #16706, #41277, #21813, #10861, #13877, #5022, #41165, #9457, #17754, #37534, #40537, #1771, #25569, #6111, #13745, #34432, #27440, #48379, #6184, #11708, #11152, #44694, #29674, #7998, #41258, #32642, #15256, #40666, #44155, #42674, #12938, #12612, #17778, #34265, #7044, #9992, #67, #11486, #18573, #35164, #42205, #19677, #14454, #24933, #47265, #25645, #11551, #11765, #36176, #13345, #20862, #18197, #34304, #37749, #16626, #18271, #40531, #28795, #15577, #6296, #2431, #5815, #36811, #8520, #35296, #4193, #8548, #4658, #11653, #48038, #6039, #12832, #40378, #45482, #27930, #42770, #17471, #34030, #22182, #23690, #15933, #36728, #1228, #13024, #46993, #25693, #1814, #35833, #24205, #33242, #23565, #15841, #36922, #35066, #21070, #10213, #41036, #10796, #33769, #1555, #31382, #1475, #26662, #10244, #40384, #10085, #41982, #42362, #45932, #29868, #25349, #27620, #46696, #12201, #14282, #45485, #5101, #21278, #11815, #34600, #43913, #6353, #19027, #28231, #35502, #41818, #24046, #33055, #3361, #48307, #12294, #47577, #383, #15838, #18633, #42766, #40450, #28067 ) ) ;
#23199 = DIRECTION ( 'NONE',  ( 0.000000000000000000, 0.000000000000000000, 1.000000000000000000 ) ) ;
#23201 = AXIS2_PLACEMENT_3D ( 'NONE', #23905, #45943, #31987 ) ;
#23202 = CARTESIAN_POINT ( 'NONE',  ( 0.000000000000000000, 8.966570791701871102, -81.50828551894218776 ) ) ;
#23203 = EDGE_LOOP ( 'NONE', ( #38907, #12867, #44394, #21038 ) ) ;
#23204 = DIRECTION ( 'NONE',  ( -1.000000000000000000, 0.000000000000000000, 0.000000000000000000 ) ) ;
#23205 = ORIENTED_EDGE ( 'NONE', *, *, #2107, .T. ) ;
#23206 = VERTEX_POINT ( 'NONE', #35271 ) ;
#23207 = CARTESIAN_POINT ( 'NONE',  ( 11.99999999999999822, 58.39081064771822582, -50.95692526931267707 ) ) ;
#23208 = DIRECTION ( 'NONE',  ( 0.000000000000000000, 1.000000000000000000, 0.000000000000000000 ) ) ;
#23209 = CARTESIAN_POINT ( 'NONE',  ( 0.000000000000000000, -81.34940948281344220, 10.30890764327356557 ) ) ;
#23210 = EDGE_CURVE ( 'NONE', #31534, #14555, #21473, .T. ) ;
#23211 = DIRECTION ( 'NONE',  ( 1.000000000000000000, 0.000000000000000000, 0.000000000000000000 ) ) ;
#23212 = ORIENTED_EDGE ( 'NONE', *, *, #11460, .T. ) ;
#23213 = EDGE_CURVE ( 'NONE', #29530, #43468, #29266, .T. ) ;
#23214 = EDGE_CURVE ( 'NONE', #43260, #5351, #364, .T. ) ;
#23215 = ORIENTED_EDGE ( 'NONE', *, *, #29244, .T. ) ;
#23216 = AXIS2_PLACEMENT_3D ( 'NONE', #26544, #37317, #19417 ) ;
#23217 = DIRECTION ( 'NONE',  ( 0.000000000000000000, 1.000000000000000000, 1.445602896647339410E-16 ) ) ;
#23218 = VECTOR ( 'NONE', #10382, 1000.000000000000000 ) ;
#23219 = VERTEX_POINT ( 'NONE', #31625 ) ;
#23220 = APPLICATION_CONTEXT ( 'automotive_design' ) ;
#23221 = DIRECTION ( 'NONE',  ( -0.000000000000000000, -0.000000000000000000, -1.000000000000000000 ) ) ;
#23222 = VERTEX_POINT ( 'NONE', #31871 ) ;
#23223 = CARTESIAN_POINT ( 'NONE',  ( -2.977765906491215642, 0.000000000000000000, 0.000000000000000000 ) ) ;
#23224 = DIRECTION ( 'NONE',  ( -1.000000000000000000, -0.000000000000000000, 0.000000000000000000 ) ) ;
#23225 = AXIS2_PLACEMENT_3D ( 'NONE', #8528, #16143, #11979 ) ;
#23226 = CARTESIAN_POINT ( 'NONE',  ( 6.000000000000000000, 79.10210256391398786, -21.60688246758503794 ) ) ;
#23227 = DIRECTION ( 'NONE',  ( 1.000000000000000000, -0.000000000000000000, 0.000000000000000000 ) ) ;
#23228 = EDGE_CURVE ( 'NONE', #13266, #13632, #5064, .T. ) ;
#23229 = DIRECTION ( 'NONE',  ( -1.000000000000000000, 0.000000000000000000, -0.000000000000000000 ) ) ;
#23230 = DIRECTION ( 'NONE',  ( 0.000000000000000000, 0.9945218953682742891, 0.1045284632676436315 ) ) ;
#23231 = CARTESIAN_POINT ( 'NONE',  ( 0.000000000000000000, -59.75363087400035056, -56.15606465355021015 ) ) ;
#23232 = VECTOR ( 'NONE', #26545, 1000.000000000000000 ) ;
#23233 = CARTESIAN_POINT ( 'NONE',  ( 11.99999999999999822, -24.73286445877655382, -73.44644590900085745 ) ) ;
#23234 = CARTESIAN_POINT ( 'NONE',  ( 10.00000000000000000, 0.000000000000000000, 0.000000000000000000 ) ) ;
#23235 = VERTEX_POINT ( 'NONE', #38727 ) ;
#23236 = ADVANCED_FACE ( 'NONE', ( #24252 ), #39192, .F. ) ;
#23237 = DIRECTION ( 'NONE',  ( -0.000000000000000000, -0.000000000000000000, -1.000000000000000000 ) ) ;
#23238 = DIRECTION ( 'NONE',  ( -1.000000000000000000, 0.000000000000000000, -0.000000000000000000 ) ) ;
#23239 = APPLICATION_PROTOCOL_DEFINITION ( 'draft international standard', 'automotive_design', 1998, #25068 ) ;
#23240 = CARTESIAN_POINT ( 'NONE',  ( -3.961125083139900749, -143.2122702051246677, 5.500000000000000000 ) ) ;
#23241 = ORIENTED_EDGE ( 'NONE', *, *, #30792, .T. ) ;
#23242 = ORIENTED_EDGE ( 'NONE', *, *, #46467, .F. ) ;
#23243 = VERTEX_POINT ( 'NONE', #35029 ) ;
#23244 = UNCERTAINTY_MEASURE_WITH_UNIT (LENGTH_MEASURE( 1.000000000000000082E-05 ), #33518, 'distance_accuracy_value', 'NONE');
#23245 = DIRECTION ( 'NONE',  ( -1.000000000000000000, 0.000000000000000000, -0.000000000000000000 ) ) ;
#23246 = EDGE_LOOP ( 'NONE', ( #37161, #38295, #43067 ) ) ;
#23247 = FACE_OUTER_BOUND ( 'NONE', #10140, .T. ) ;
#23248 = DIRECTION ( 'NONE',  ( -1.000000000000000000, -0.000000000000000000, 0.000000000000000000 ) ) ;
#23249 = ORIENTED_EDGE ( 'NONE', *, *, #12401, .F. ) ;
#23250 = EDGE_CURVE ( 'NONE', #23509, #13181, #32417, .T. ) ;
#23251 = AXIS2_PLACEMENT_3D ( 'NONE', #24538, #20873, #46330 ) ;
#23252 = EDGE_CURVE ( 'NONE', #45060, #526, #43361, .T. ) ;
#23253 = CARTESIAN_POINT ( 'NONE',  ( 0.000000000000000000, -77.16300072079641836, -27.74655509720752278 ) ) ;
#23254 = EDGE_LOOP ( 'NONE', ( #3000, #449, #44288, #24151 ) ) ;
#23255 = ADVANCED_FACE ( 'NONE', ( #29376 ), #40158, .T. ) ;
#23256 = VECTOR ( 'NONE', #28826, 1000.000000000000114 ) ;
#23257 = ORIENTED_EDGE ( 'NONE', *, *, #26413, .F. ) ;
#23258 = EDGE_LOOP ( 'NONE', ( #10788, #45326, #1667, #31109 ) ) ;
#23259 = ORIENTED_EDGE ( 'NONE', *, *, #2769, .T. ) ;
#23260 = EDGE_CURVE ( 'NONE', #34421, #13155, #3165, .T. ) ;
#23261 = CARTESIAN_POINT ( 'NONE',  ( 0.000000000000000000, -8.966570791700167575, -81.50828551894237251 ) ) ;
#23262 = CIRCLE ( 'NONE', #37315, 12.49999999999999645 ) ;
#23263 = ORIENTED_EDGE ( 'NONE', *, *, #40249, .T. ) ;
#23264 = DIRECTION ( 'NONE',  ( 1.000000000000000000, -0.000000000000000000, 0.000000000000000000 ) ) ;
#23265 = ORIENTED_EDGE ( 'NONE', *, *, #30710, .T. ) ;
#23266 = DIRECTION ( 'NONE',  ( 0.000000000000000000, 0.7071067811865437980, 0.7071067811865512365 ) ) ;
#23267 = ORIENTED_EDGE ( 'NONE', *, *, #33378, .F. ) ;
#23268 = CARTESIAN_POINT ( 'NONE',  ( 8.700667342345820288, -98.11853780484867116, 5.500000000000000000 ) ) ;
#23269 = CARTESIAN_POINT ( 'NONE',  ( 0.000000000000000000, -27.13269053701078448, -25.88420570971428702 ) ) ;
#23270 = EDGE_CURVE ( 'NONE', #2149, #24044, #10776, .T. ) ;
#23271 = DIRECTION ( 'NONE',  ( -1.000000000000000000, 0.000000000000000000, -0.000000000000000000 ) ) ;
#23272 = EDGE_CURVE ( 'NONE', #43433, #11777, #41787, .T. ) ;
#23273 = EDGE_LOOP ( 'NONE', ( #1173, #47740, #11446, #33140 ) ) ;
#23274 = VECTOR ( 'NONE', #22017, 1000.000000000000000 ) ;
#23275 = CARTESIAN_POINT ( 'NONE',  ( 0.000000000000000000, -8.840884882374576037, -74.65374052328658649 ) ) ;
#23276 = CYLINDRICAL_SURFACE ( 'NONE', #33653, 77.49899999999999523 ) ;
#23277 = VERTEX_POINT ( 'NONE', #40400 ) ;
#23278 = DIRECTION ( 'NONE',  ( -1.000000000000000000, 0.000000000000000000, -0.000000000000000000 ) ) ;
#23279 = EDGE_LOOP ( 'NONE', ( #24593, #24759, #30800, #45690 ) ) ;
#23280 = DIRECTION ( 'NONE',  ( 0.000000000000000000, 0.000000000000000000, 1.000000000000000000 ) ) ;
#23281 = CARTESIAN_POINT ( 'NONE',  ( 10.00000000000000000, 35.53030884539102630, -12.26510123303222599 ) ) ;
#23282 = ORIENTED_EDGE ( 'NONE', *, *, #22295, .F. ) ;
#23283 = DIRECTION ( 'NONE',  ( -0.000000000000000000, -0.000000000000000000, 1.000000000000000000 ) ) ;
#23284 = DIRECTION ( 'NONE',  ( 0.000000000000000000, -0.07845909572785234043, 0.9969173337331274087 ) ) ;
#23285 = DIRECTION ( 'NONE',  ( -1.000000000000000000, 0.000000000000000000, 0.000000000000000000 ) ) ;
#23286 = CARTESIAN_POINT ( 'NONE',  ( 10.00000000000000000, 0.000000000000000000, 0.000000000000000000 ) ) ;
#23287 = DIRECTION ( 'NONE',  ( -0.000000000000000000, -0.000000000000000000, -1.000000000000000000 ) ) ;
#23288 = EDGE_CURVE ( 'NONE', #37280, #25536, #18352, .T. ) ;
#23289 = DIRECTION ( 'NONE',  ( 0.000000000000000000, 0.000000000000000000, 1.000000000000000000 ) ) ;
#23290 = AXIS2_PLACEMENT_3D ( 'NONE', #31116, #43984, #10452 ) ;
#23291 = ORIENTED_EDGE ( 'NONE', *, *, #3087, .F. ) ;
#23292 = PLANE ( 'NONE',  #43452 ) ;
#23293 = CARTESIAN_POINT ( 'NONE',  ( -3.360000000000002096, 2.571758278209441661E-15, 21.00000000000000000 ) ) ;
#23294 = DIRECTION ( 'NONE',  ( 0.000000000000000000, 0.000000000000000000, 1.000000000000000000 ) ) ;
#23295 = ORIENTED_EDGE ( 'NONE', *, *, #25354, .F. ) ;
#23296 = CIRCLE ( 'NONE', #9211, 37.49900000000000233 ) ;
#23297 = LINE ( 'NONE', #12296, #26028 ) ;
#23298 = LINE ( 'NONE', #30173, #4230 ) ;
#23300 = CIRCLE ( 'NONE', #38148, 77.49900000000000944 ) ;
#23299 = DIRECTION ( 'NONE',  ( -1.000000000000000000, -0.000000000000000000, 0.000000000000000000 ) ) ;
#23301 = ORIENTED_EDGE ( 'NONE', *, *, #4630, .T. ) ;
#23302 = FACE_BOUND ( 'NONE', #39641, .T. ) ;
#23303 = VERTEX_POINT ( 'NONE', #40625 ) ;
#23304 = CARTESIAN_POINT ( 'NONE',  ( 10.00000000000000000, -71.27951684758046724, 30.41916302227088309 ) ) ;
#23305 = PRODUCT_DEFINITION_FORMATION_WITH_SPECIFIED_SOURCE ( 'ANY', '', #1883, .NOT_KNOWN. ) ;
#23306 = CARTESIAN_POINT ( 'NONE',  ( 10.00000000000000000, 59.03342792756328095, -46.54456581323744757 ) ) ;
#23307 = ORIENTED_EDGE ( 'NONE', *, *, #42609, .F. ) ;
#23308 = CONICAL_SURFACE ( 'NONE', #8453, 13.71319123027096865, 1.361356816555593596 ) ;
#23309 = CARTESIAN_POINT ( 'NONE',  ( 10.00000000000000000, -9.188173127307003085, -40.98264845739760176 ) ) ;
#23310 = ADVANCED_FACE ( 'NONE', ( #25447 ), #10045, .T. ) ;
#23311 = ORIENTED_EDGE ( 'NONE', *, *, #45758, .F. ) ;
#23312 = EDGE_CURVE ( 'NONE', #39764, #34627, #18097, .T. ) ;
#23313 = EDGE_LOOP ( 'NONE', ( #10073, #37101, #32433, #39894 ) ) ;
#23314 = DIRECTION ( 'NONE',  ( 1.000000000000000000, 0.000000000000000000, 0.000000000000000000 ) ) ;
#23315 = VERTEX_POINT ( 'NONE', #24967 ) ;
#23316 = CARTESIAN_POINT ( 'NONE',  ( 0.000000000000000000, 56.15606465355042332, -59.75363087400017292 ) ) ;
#23318 = ORIENTED_EDGE ( 'NONE', *, *, #21613, .F. ) ;
#23317 = LINE ( 'NONE', #4487, #27820 ) ;
#23319 = EDGE_LOOP ( 'NONE', ( #31876, #34812, #12207, #4643 ) ) ;
#23320 = AXIS2_PLACEMENT_3D ( 'NONE', #8591, #13021, #41656 ) ;
#23321 = AXIS2_PLACEMENT_3D ( 'NONE', #47100, #17947, #10376 ) ;
#23322 = CARTESIAN_POINT ( 'NONE',  ( 10.00000000000000000, 81.50828551894240093, -8.966570791699799869 ) ) ;
#23323 = CARTESIAN_POINT ( 'NONE',  ( 0.000000000000000000, -27.75498641678720446, -31.52238457039628727 ) ) ;
#23324 = EDGE_CURVE ( 'NONE', #18975, #11732, #39914, .T. ) ;
#23325 = DIRECTION ( 'NONE',  ( 0.000000000000000000, 0.000000000000000000, 1.000000000000000000 ) ) ;
#23326 = DIRECTION ( 'NONE',  ( 0.000000000000000000, 1.000000000000000000, 0.000000000000000000 ) ) ;
#23327 = VERTEX_POINT ( 'NONE', #7089 ) ;
#23328 = DIRECTION ( 'NONE',  ( 0.000000000000000000, 0.9945218953682742891, -0.1045284632676436315 ) ) ;
#23329 = ORIENTED_EDGE ( 'NONE', *, *, #9252, .T. ) ;
#23330 = EDGE_LOOP ( 'NONE', ( #43393, #12617, #42226, #392 ) ) ;
#23331 = EDGE_CURVE ( 'NONE', #16986, #26232, #29120, .T. ) ;
#23332 = FACE_OUTER_BOUND ( 'NONE', #5737, .T. ) ;
#23333 = DIRECTION ( 'NONE',  ( -1.000000000000000000, 0.000000000000000000, 0.000000000000000000 ) ) ;
#23334 = LINE ( 'NONE', #16479, #6322 ) ;
#23335 = CYLINDRICAL_SURFACE ( 'NONE', #36789, 42.00000000000000000 ) ;
#23336 = ORIENTED_EDGE ( 'NONE', *, *, #31011, .F. ) ;
#23337 = DIRECTION ( 'NONE',  ( -0.000000000000000000, -0.000000000000000000, -1.000000000000000000 ) ) ;
#23338 = DIRECTION ( 'NONE',  ( 0.000000000000000000, 0.4067366430757908824, -0.9135454576426050854 ) ) ;
#23339 = DIRECTION ( 'NONE',  ( -1.000000000000000000, -0.000000000000000000, -0.000000000000000000 ) ) ;
#23340 = AXIS2_PLACEMENT_3D ( 'NONE', #11334, #7409, #22344 ) ;
#23341 = CARTESIAN_POINT ( 'NONE',  ( 10.00000000000000000, 62.20884554314086046, -46.21855187248561236 ) ) ;
#23342 = EDGE_CURVE ( 'NONE', #25836, #919, #22015, .T. ) ;
#23343 = CARTESIAN_POINT ( 'NONE',  ( 0.000000000000000000, 0.8828120875900632436, 37.48860685352291000 ) ) ;
#23344 = CARTESIAN_POINT ( 'NONE',  ( 0.000000000000000000, -30.84782396557233142, 21.32104025579104345 ) ) ;
#23345 = CYLINDRICAL_SURFACE ( 'NONE', #9509, 10.00000000000000178 ) ;
#23346 = LINE ( 'NONE', #11854, #11471 ) ;
#23347 = CARTESIAN_POINT ( 'NONE',  ( -10.00000000000000000, 0.000000000000000000, 0.000000000000000000 ) ) ;
#23348 = CARTESIAN_POINT ( 'NONE',  ( 10.00000000000000000, 76.69515212746057387, -29.01471420065480089 ) ) ;
#23349 = EDGE_LOOP ( 'NONE', ( #41896, #43662, #20012, #26527 ) ) ;
#23350 = EDGE_LOOP ( 'NONE', ( #31163, #21178, #27972, #26497 ) ) ;
#23351 = FACE_OUTER_BOUND ( 'NONE', #9812, .T. ) ;
#23352 = DIRECTION ( 'NONE',  ( 0.000000000000000000, 0.7071067811865487940, -0.7071067811865462405 ) ) ;
#23353 = AXIS2_PLACEMENT_3D ( 'NONE', #35222, #39650, #6109 ) ;
#23354 = VERTEX_POINT ( 'NONE', #14692 ) ;
#23355 = ORIENTED_EDGE ( 'NONE', *, *, #37401, .F. ) ;
#23356 = CIRCLE ( 'NONE', #42898, 42.00000000000000000 ) ;
#23357 = AXIS2_PLACEMENT_3D ( 'NONE', #48410, #37403, #33963 ) ;
#23358 = CYLINDRICAL_SURFACE ( 'NONE', #44010, 31.99999999999999289 ) ;
#23359 = ORIENTED_EDGE ( 'NONE', *, *, #7193, .T. ) ;
#23360 = EDGE_CURVE ( 'NONE', #45107, #34199, #10283, .T. ) ;
#23361 = VERTEX_POINT ( 'NONE', #11012 ) ;
#23362 = EDGE_CURVE ( 'NONE', #12471, #34159, #1927, .T. ) ;
#23363 = ORIENTED_EDGE ( 'NONE', *, *, #9839, .T. ) ;
#23364 = VERTEX_POINT ( 'NONE', #17626 ) ;
#23365 = EDGE_CURVE ( 'NONE', #11714, #17149, #22275, .T. ) ;
#23366 =( GEOMETRIC_REPRESENTATION_CONTEXT ( 3 ) GLOBAL_UNCERTAINTY_ASSIGNED_CONTEXT ( ( #718 ) ) GLOBAL_UNIT_ASSIGNED_CONTEXT ( ( #46005, #1208, #8056 ) ) REPRESENTATION_CONTEXT ( 'NONE', 'WORKASPACE' ) );
#23367 = FACE_OUTER_BOUND ( 'NONE', #37214, .T. ) ;
#23368 = ADVANCED_FACE ( 'NONE', ( #18597 ), #33517, .T. ) ;
#23369 = EDGE_CURVE ( 'NONE', #21200, #48285, #32567, .T. ) ;
#23370 = CARTESIAN_POINT ( 'NONE',  ( 0.000000000000000000, -74.74816331893404708, -33.71516098798818462 ) ) ;
#23371 = DIRECTION ( 'NONE',  ( 0.000000000000000000, 0.000000000000000000, 1.000000000000000000 ) ) ;
#23372 = ORIENTED_EDGE ( 'NONE', *, *, #34056, .T. ) ;
#23373 = DIRECTION ( 'NONE',  ( 0.000000000000000000, 0.000000000000000000, 1.000000000000000000 ) ) ;
#23374 = ORIENTED_EDGE ( 'NONE', *, *, #18417, .T. ) ;
#23375 = VERTEX_POINT ( 'NONE', #43813 ) ;
#23376 = LINE ( 'NONE', #9408, #20217 ) ;
#23377 = CARTESIAN_POINT ( 'NONE',  ( 10.00000000000000000, -62.50884508063395373, -41.76106447765554464 ) ) ;
#23378 = LINE ( 'NONE', #4547, #11051 ) ;
#23379 = VERTEX_POINT ( 'NONE', #25199 ) ;
#23380 = ORIENTED_EDGE ( 'NONE', *, *, #24103, .F. ) ;
#23381 = DIRECTION ( 'NONE',  ( 0.000000000000000000, 0.000000000000000000, 1.000000000000000000 ) ) ;
#23382 = EDGE_LOOP ( 'NONE', ( #34176, #6970, #48324, #27236 ) ) ;
#23383 = FACE_OUTER_BOUND ( 'NONE', #29005, .T. ) ;
#23384 = VECTOR ( 'NONE', #29800, 1000.000000000000000 ) ;
#23385 = LINE ( 'NONE', #7967, #39751 ) ;
#23386 = DIRECTION ( 'NONE',  ( 1.000000000000000000, 0.000000000000000000, 0.000000000000000000 ) ) ;
#23387 = CYLINDRICAL_SURFACE ( 'NONE', #42508, 77.49899999999999523 ) ;
#23388 = CARTESIAN_POINT ( 'NONE',  ( 11.99999999999999822, -0.8261519478436571973, 77.49459641780886443 ) ) ;
#23389 = DIRECTION ( 'NONE',  ( 0.000000000000000000, -0.7071067811865536790, 0.7071067811865414665 ) ) ;
#23390 = DIRECTION ( 'NONE',  ( -1.000000000000000000, 0.000000000000000000, 0.000000000000000000 ) ) ;
#23391 = DIRECTION ( 'NONE',  ( 0.000000000000000000, 0.000000000000000000, 1.000000000000000000 ) ) ;
#23392 = DIRECTION ( 'NONE',  ( -1.000000000000000000, -0.000000000000000000, -0.000000000000000000 ) ) ;
#23393 = DIRECTION ( 'NONE',  ( 0.000000000000000000, 0.000000000000000000, 1.000000000000000000 ) ) ;
#23394 = ADVANCED_FACE ( 'NONE', ( #21550 ), #2938, .T. ) ;
#23395 = DIRECTION ( 'NONE',  ( -0.000000000000000000, -0.000000000000000000, -1.000000000000000000 ) ) ;
#23396 = ORIENTED_EDGE ( 'NONE', *, *, #15094, .F. ) ;
#23397 = ORIENTED_EDGE ( 'NONE', *, *, #16636, .T. ) ;
#23398 = CIRCLE ( 'NONE', #47634, 31.99999999999999645 ) ;
#23399 = CARTESIAN_POINT ( 'NONE',  ( -3.961125083139900749, -143.2122702051246677, 5.500000000000000000 ) ) ;
#23400 = CARTESIAN_POINT ( 'NONE',  ( -9.055038557894883766, -98.31460683512894150, 2.500000000000000000 ) ) ;
#23401 = CARTESIAN_POINT ( 'NONE',  ( 5.999999999999999112, 51.29473840253223216, 63.97538442413444670 ) ) ;
#23402 = DIRECTION ( 'NONE',  ( -1.000000000000000000, 0.000000000000000000, -0.000000000000000000 ) ) ;
#23403 = EDGE_CURVE ( 'NONE', #41148, #35055, #45693, .T. ) ;
#23404 = CARTESIAN_POINT ( 'NONE',  ( 10.00000000000000000, 0.000000000000000000, 0.000000000000000000 ) ) ;
#23405 = CARTESIAN_POINT ( 'NONE',  ( 10.00000000000000000, 0.000000000000000000, 0.000000000000000000 ) ) ;
#23406 = ADVANCED_FACE ( 'NONE', ( #15650 ), #8055, .T. ) ;
#23407 = ORIENTED_EDGE ( 'NONE', *, *, #12664, .F. ) ;
#23408 = CARTESIAN_POINT ( 'NONE',  ( 0.000000000000000000, 0.000000000000000000, 0.000000000000000000 ) ) ;
#23409 = CARTESIAN_POINT ( 'NONE',  ( 10.00000000000000000, -26.08949754953005495, -27.05870788708258701 ) ) ;
#23410 = ORIENTED_EDGE ( 'NONE', *, *, #33166, .T. ) ;
#23411 = ORIENTED_EDGE ( 'NONE', *, *, #14040, .T. ) ;
#23412 = FILL_AREA_STYLE ('',( #19013 ) ) ;
#23413 = CARTESIAN_POINT ( 'NONE',  ( 10.00000000000000000, -37.58145647212455032, 0.6853352020789044152 ) ) ;
#23414 = EDGE_LOOP ( 'NONE', ( #40694, #5444, #7071, #40046 ) ) ;
#23415 = EDGE_CURVE ( 'NONE', #35410, #39037, #45498, .T. ) ;
#23416 = CIRCLE ( 'NONE', #15596, 16.00000000000000000 ) ;
#23417 = AXIS2_PLACEMENT_3D ( 'NONE', #32000, #46917, #13383 ) ;
#23418 = ADVANCED_FACE ( 'NONE', ( #4633 ), #30350, .T. ) ;
#23419 = ORIENTED_EDGE ( 'NONE', *, *, #21084, .T. ) ;
#23420 = AXIS2_PLACEMENT_3D ( 'NONE', #18492, #41261, #26326 ) ;
#23421 = CYLINDRICAL_SURFACE ( 'NONE', #32002, 82.00000000000000000 ) ;
#23422 = EDGE_CURVE ( 'NONE', #31590, #15551, #47296, .T. ) ;
#23423 = VERTEX_POINT ( 'NONE', #22745 ) ;
#23424 = VERTEX_POINT ( 'NONE', #7818 ) ;
#23425 = VECTOR ( 'NONE', #7130, 1000.000000000000000 ) ;
#23426 = EDGE_CURVE ( 'NONE', #17612, #4369, #19312, .T. ) ;
#23427 = CARTESIAN_POINT ( 'NONE',  ( 5.000000000000000000, -38.55633173626998911, -16.65560815589452304 ) ) ;
#23428 = LINE ( 'NONE', #13875, #26896 ) ;
#23429 = EDGE_LOOP ( 'NONE', ( #15871, #4769, #28923, #45704 ) ) ;
#23430 = ORIENTED_EDGE ( 'NONE', *, *, #38916, .T. ) ;
#23431 = DIRECTION ( 'NONE',  ( 0.000000000000000000, 0.8090169943749447867, 0.5877852522924769119 ) ) ;
#23433 = VERTEX_POINT ( 'NONE', #20459 ) ;
#23432 = CARTESIAN_POINT ( 'NONE',  ( 10.00000000000000000, 8.966570791701860443, -81.50828551894217355 ) ) ;
#23434 = DIRECTION ( 'NONE',  ( 0.000000000000000000, 0.000000000000000000, 1.000000000000000000 ) ) ;
#23435 = ORIENTED_EDGE ( 'NONE', *, *, #44123, .F. ) ;
#23436 = DIRECTION ( 'NONE',  ( 0.000000000000000000, 0.000000000000000000, 1.000000000000000000 ) ) ;
#23437 = ORIENTED_EDGE ( 'NONE', *, *, #17209, .T. ) ;
#23438 = ORIENTED_EDGE ( 'NONE', *, *, #15832, .F. ) ;
#23439 = DIRECTION ( 'NONE',  ( 0.000000000000000000, 0.000000000000000000, 1.000000000000000000 ) ) ;
#23440 = FACE_OUTER_BOUND ( 'NONE', #35421, .T. ) ;
#23441 = ORIENTED_EDGE ( 'NONE', *, *, #13480, .T. ) ;
#23442 = CARTESIAN_POINT ( 'NONE',  ( 0.000000000000000000, 31.47745569255140552, 68.26794271651274926 ) ) ;
#23443 = DIRECTION ( 'NONE',  ( -1.000000000000000000, 0.000000000000000000, -0.000000000000000000 ) ) ;
#23444 = EDGE_LOOP ( 'NONE', ( #11291, #2925, #47225, #36346 ) ) ;
#23445 = VERTEX_POINT ( 'NONE', #38168 ) ;
#23446 = EDGE_CURVE ( 'NONE', #3270, #24628, #22992, .T. ) ;
#23447 = CARTESIAN_POINT ( 'NONE',  ( 11.99999999999999822, -11.30684508768393748, 76.66974797899833050 ) ) ;
#23448 = CARTESIAN_POINT ( 'NONE',  ( 10.00000000000000000, -46.54456581323762521, -59.03342792756313884 ) ) ;
#23449 = ORIENTED_EDGE ( 'NONE', *, *, #40256, .F. ) ;
#23450 = AXIS2_PLACEMENT_3D ( 'NONE', #28504, #43440, #9896 ) ;
#23451 = DIRECTION ( 'NONE',  ( -1.000000000000000000, 0.000000000000000000, -0.000000000000000000 ) ) ;
#23452 = ORIENTED_EDGE ( 'NONE', *, *, #42379, .T. ) ;
#23453 = AXIS2_PLACEMENT_3D ( 'NONE', #32801, #18112, #47730 ) ;
#23454 = DIRECTION ( 'NONE',  ( 0.000000000000000000, 0.7604059656000276002, 0.6494480483301876550 ) ) ;
#23455 = CARTESIAN_POINT ( 'NONE',  ( 11.99999999999999822, 73.73191006444551476, 14.66109333815590254 ) ) ;
#23456 = CARTESIAN_POINT ( 'NONE',  ( 0.000000000000000000, 0.000000000000000000, 0.000000000000000000 ) ) ;
#23457 = DIRECTION ( 'NONE',  ( 0.000000000000000000, 0.000000000000000000, 1.000000000000000000 ) ) ;
#23458 = VECTOR ( 'NONE', #16249, 1000.000000000000000 ) ;
#23459 = CARTESIAN_POINT ( 'NONE',  ( 10.00000000000000000, 0.000000000000000000, 0.000000000000000000 ) ) ;
#23460 = CYLINDRICAL_SURFACE ( 'NONE', #27059, 77.49899999999999523 ) ;
#23461 = VECTOR ( 'NONE', #23028, 1000.000000000000000 ) ;
#23462 = DIRECTION ( 'NONE',  ( 0.000000000000000000, 0.000000000000000000, 1.000000000000000000 ) ) ;
#23463 = ORIENTED_EDGE ( 'NONE', *, *, #45513, .T. ) ;
#23464 = ADVANCED_FACE ( 'NONE', ( #15421 ), #34239, .F. ) ;
#23465 = CARTESIAN_POINT ( 'NONE',  ( 5.000000000000000000, 27.75498641678786527, -31.52238457039571173 ) ) ;
#23466 =( LENGTH_UNIT ( ) NAMED_UNIT ( * ) SI_UNIT ( .MILLI., .METRE. ) );
#23467 = DIRECTION ( 'NONE',  ( -1.000000000000000000, 0.000000000000000000, 0.000000000000000000 ) ) ;
#23468 = VERTEX_POINT ( 'NONE', #45271 ) ;
#23469 = VERTEX_POINT ( 'NONE', #1630 ) ;
#23470 = DIRECTION ( 'NONE',  ( 1.000000000000000000, 0.000000000000000000, 0.000000000000000000 ) ) ;
#23471 = ORIENTED_EDGE ( 'NONE', *, *, #45144, .F. ) ;
#23472 = CARTESIAN_POINT ( 'NONE',  ( 10.00000000000000000, -27.05870788708250885, 26.08949754953014022 ) ) ;
#23473 = EDGE_CURVE ( 'NONE', #21639, #11732, #44145, .T. ) ;
#23474 = FACE_OUTER_BOUND ( 'NONE', #47527, .T. ) ;
#23475 = ORIENTED_EDGE ( 'NONE', *, *, #22221, .T. ) ;
#23476 = EDGE_CURVE ( 'NONE', #44907, #23020, #28540, .T. ) ;
#23477 = ADVANCED_FACE ( 'NONE', ( #7587 ), #712, .T. ) ;
#23478 = ORIENTED_EDGE ( 'NONE', *, *, #35259, .T. ) ;
#23479 = AXIS2_PLACEMENT_3D ( 'NONE', #9347, #45582, #30924 ) ;
#23480 = EDGE_CURVE ( 'NONE', #41940, #34545, #26187, .T. ) ;
#23481 = CARTESIAN_POINT ( 'NONE',  ( 0.000000000000000000, 0.000000000000000000, 0.000000000000000000 ) ) ;
#23482 = AXIS2_PLACEMENT_3D ( 'NONE', #37058, #17734, #43921 ) ;
#23483 = AXIS2_PLACEMENT_3D ( 'NONE', #25952, #33774, #30601 ) ;
#23484 = ORIENTED_EDGE ( 'NONE', *, *, #42329, .F. ) ;
#23485 = EDGE_LOOP ( 'NONE', ( #17192, #10614, #19246, #24510 ) ) ;
#23486 = ORIENTED_EDGE ( 'NONE', *, *, #13185, .T. ) ;
#23487 = EDGE_LOOP ( 'NONE', ( #31355, #23463, #22638, #29248 ) ) ;
#23488 = EDGE_CURVE ( 'NONE', #47828, #24283, #41061, .T. ) ;
#23489 = ORIENTED_EDGE ( 'NONE', *, *, #23902, .T. ) ;
#23490 = COLOUR_RGB ( '', 0.31764706, 0.68627451, 0.89019608) ;
#23491 = VECTOR ( 'NONE', #13781, 1000.000000000000000 ) ;
#23492 = DIRECTION ( 'NONE',  ( 0.000000000000000000, 0.1564344650402311743, -0.9876883405951376593 ) ) ;
#23493 = AXIS2_PLACEMENT_3D ( 'NONE', #42356, #13226, #32307 ) ;
#23494 = ORIENTED_EDGE ( 'NONE', *, *, #19542, .F. ) ;
#23495 = DIRECTION ( 'NONE',  ( -1.000000000000000000, 0.000000000000000000, 0.000000000000000000 ) ) ;
#23496 = VERTEX_POINT ( 'NONE', #41599 ) ;
#23497 = CARTESIAN_POINT ( 'NONE',  ( 0.000000000000000000, 62.50884508063487033, -41.76106447765422303 ) ) ;
#23498 = ORIENTED_EDGE ( 'NONE', *, *, #41792, .F. ) ;
#23499 = CARTESIAN_POINT ( 'NONE',  ( 15.00000000000000000, -3.948201729842355068, -23.21447184625292692 ) ) ;
#23500 = DIRECTION ( 'NONE',  ( -1.000000000000000000, -0.000000000000000000, -0.000000000000000000 ) ) ;
#23501 = VERTEX_POINT ( 'NONE', #37442 ) ;
#23502 = DIRECTION ( 'NONE',  ( -1.000000000000000000, -0.000000000000000000, -0.000000000000000000 ) ) ;
#23503 = ORIENTED_EDGE ( 'NONE', *, *, #16087, .T. ) ;
#23504 = ADVANCED_FACE ( 'NONE', ( #37930 ), #15178, .T. ) ;
#23505 = CARTESIAN_POINT ( 'NONE',  ( 10.00000000000000000, -21.53537804866058991, -30.80686688397033635 ) ) ;
#23506 = CARTESIAN_POINT ( 'NONE',  ( 10.00000000000000000, 0.000000000000000000, 0.000000000000000000 ) ) ;
#23507 = ORIENTED_EDGE ( 'NONE', *, *, #2631, .F. ) ;
#23508 = DIRECTION ( 'NONE',  ( 1.000000000000000000, -0.000000000000000000, 0.000000000000000000 ) ) ;
#23509 = VERTEX_POINT ( 'NONE', #26434 ) ;
#23510 = DIRECTION ( 'NONE',  ( 0.000000000000000000, 0.000000000000000000, 1.000000000000000000 ) ) ;
#23511 = DIRECTION ( 'NONE',  ( -1.000000000000000000, -0.000000000000000000, 0.000000000000000000 ) ) ;
#23512 = FACE_OUTER_BOUND ( 'NONE', #37996, .T. ) ;
#23513 = CYLINDRICAL_SURFACE ( 'NONE', #29790, 37.49900000000000233 ) ;
#23514 = CARTESIAN_POINT ( 'NONE',  ( 10.00000000000000000, 0.000000000000000000, 0.000000000000000000 ) ) ;
#23515 = CYLINDRICAL_SURFACE ( 'NONE', #4653, 16.00000000000000000 ) ;
#23516 = CARTESIAN_POINT ( 'NONE',  ( 11.99999999999999822, 65.58780272294129077, -36.73666225445822420 ) ) ;
#23518 = VECTOR ( 'NONE', #30220, 1000.000000000000000 ) ;
#23517 = CYLINDRICAL_SURFACE ( 'NONE', #14603, 31.99999999999998579 ) ;
#23519 = EDGE_CURVE ( 'NONE', #27398, #43433, #41365, .T. ) ;
#23520 = CARTESIAN_POINT ( 'NONE',  ( -26.29030328629082902, -123.6496510949466341, -2.500000000000000000 ) ) ;
#23521 = DIRECTION ( 'NONE',  ( 0.000000000000000000, 0.000000000000000000, 1.000000000000000000 ) ) ;
#23522 = CARTESIAN_POINT ( 'NONE',  ( 0.000000000000000000, 0.000000000000000000, 0.000000000000000000 ) ) ;
#23523 = CIRCLE ( 'NONE', #15706, 77.49900000000000944 ) ;
#23524 = VECTOR ( 'NONE', #42105, 1000.000000000000000 ) ;
#23525 = ADVANCED_FACE ( 'NONE', ( #36360 ), #13860, .T. ) ;
#23526 = DIRECTION ( 'NONE',  ( -0.000000000000000000, -0.000000000000000000, -1.000000000000000000 ) ) ;
#23527 = DIRECTION ( 'NONE',  ( 0.000000000000000000, 0.000000000000000000, 1.000000000000000000 ) ) ;
#23528 = CARTESIAN_POINT ( 'NONE',  ( 15.00000000000000000, -13.04903810567675393, -19.60159698893424718 ) ) ;
#23529 = CARTESIAN_POINT ( 'NONE',  ( 10.00000000000000000, 35.53030884539084866, 12.26510123303271982 ) ) ;
#23530 = EDGE_CURVE ( 'NONE', #26404, #911, #1169, .T. ) ;
#23531 = ORIENTED_EDGE ( 'NONE', *, *, #9176, .F. ) ;
#23532 = AXIS2_PLACEMENT_3D ( 'NONE', #10269, #47004, #35746 ) ;
#23533 = ORIENTED_EDGE ( 'NONE', *, *, #30016, .T. ) ;
#23534 = DIRECTION ( 'NONE',  ( -1.000000000000000000, -0.000000000000000000, 0.000000000000000000 ) ) ;
#23535 = MECHANICAL_DESIGN_GEOMETRIC_PRESENTATION_REPRESENTATION (  '', ( #25064 ), #40725 ) ;
#23536 = ORIENTED_EDGE ( 'NONE', *, *, #3294, .T. ) ;
#23537 = DIRECTION ( 'NONE',  ( -1.000000000000000000, 0.000000000000000000, 0.000000000000000000 ) ) ;
#23538 = CONTEXT_DEPENDENT_SHAPE_REPRESENTATION ( #48227, #4295 ) ;
#23539 = DIRECTION ( 'NONE',  ( 0.000000000000000000, -0.9510565162951500895, -0.3090169943749583314 ) ) ;
#23540 = VERTEX_POINT ( 'NONE', #2119 ) ;
#23541 = EDGE_CURVE ( 'NONE', #32362, #34492, #27741, .T. ) ;
#23542 = EDGE_CURVE ( 'NONE', #32361, #44059, #6037, .T. ) ;
#23543 = CARTESIAN_POINT ( 'NONE',  ( 12.00000000000000000, -3.948201729842032215, 23.21447184625297666 ) ) ;
#23544 = EDGE_LOOP ( 'NONE', ( #30246, #7857, #30995, #9303 ) ) ;
#23545 = SURFACE_STYLE_USAGE ( .BOTH. , #24520 ) ;
#23546 = EDGE_CURVE ( 'NONE', #45870, #6838, #39481, .T. ) ;
#23547 = CIRCLE ( 'NONE', #19620, 12.49999999999999822 ) ;
#23548 = CYLINDRICAL_SURFACE ( 'NONE', #18297, 82.00000000000000000 ) ;
#23549 = AXIS2_PLACEMENT_3D ( 'NONE', #9906, #40261, #6237 ) ;
#23550 = DIRECTION ( 'NONE',  ( 1.000000000000000000, 0.000000000000000000, -0.000000000000000000 ) ) ;
#23551 = EDGE_LOOP ( 'NONE', ( #17697, #41975, #11038, #1724 ) ) ;
#23553 = ORIENTED_EDGE ( 'NONE', *, *, #44695, .T. ) ;
#23552 = DIRECTION ( 'NONE',  ( -1.000000000000000000, -0.000000000000000000, 0.000000000000000000 ) ) ;
#23554 = CIRCLE ( 'NONE', #2449, 37.49900000000000944 ) ;
#23555 = ORIENTED_EDGE ( 'NONE', *, *, #32332, .F. ) ;
#23556 = ORIENTED_EDGE ( 'NONE', *, *, #11506, .F. ) ;
#23557 = AXIS2_PLACEMENT_3D ( 'NONE', #42798, #9253, #9727 ) ;
#23558 = CARTESIAN_POINT ( 'NONE',  ( 10.00000000000000000, 55.20638768913831029, -51.02545421589267960 ) ) ;
#23559 = CARTESIAN_POINT ( 'NONE',  ( 10.00000000000000000, 30.00120703465205452, 22.64427369931179967 ) ) ;
#23560 = CARTESIAN_POINT ( 'NONE',  ( 20.85212586905261745, -130.9402397935870965, -2.500000000000000000 ) ) ;
#23561 = CARTESIAN_POINT ( 'NONE',  ( 11.99999999999999822, -55.20638768913724448, -51.02545421589383068 ) ) ;
#23562 = VERTEX_POINT ( 'NONE', #32460 ) ;
#23563 = DIRECTION ( 'NONE',  ( 0.000000000000000000, -0.8090169943749403458, -0.5877852522924830181 ) ) ;
#23564 = ORIENTED_EDGE ( 'NONE', *, *, #41830, .T. ) ;
#23565 = ORIENTED_EDGE ( 'NONE', *, *, #8449, .T. ) ;
#23566 = AXIS2_PLACEMENT_3D ( 'NONE', #41462, #7682, #810 ) ;
#23567 = DIRECTION ( 'NONE',  ( 0.000000000000000000, -0.4539904997395352027, -0.8910065241883737830 ) ) ;
#23568 = AXIS2_PLACEMENT_3D ( 'NONE', #19564, #973, #4188 ) ;
#23569 = DIRECTION ( 'NONE',  ( 1.000000000000000000, 0.000000000000000000, 0.000000000000000000 ) ) ;
#23570 = DIRECTION ( 'NONE',  ( 1.000000000000000000, 0.000000000000000000, -0.000000000000000000 ) ) ;
#23571 = LINE ( 'NONE', #16250, #46179 ) ;
#23572 = ORIENTED_EDGE ( 'NONE', *, *, #21965, .F. ) ;
#23573 = CARTESIAN_POINT ( 'NONE',  ( 5.000000000000000000, 27.74655509720779634, -77.16300072079631889 ) ) ;
#23574 = DIRECTION ( 'NONE',  ( 0.000000000000000000, 0.000000000000000000, 1.000000000000000000 ) ) ;
#23575 = DIRECTION ( 'NONE',  ( -1.000000000000000000, 0.000000000000000000, -0.000000000000000000 ) ) ;
#23576 = DIRECTION ( 'NONE',  ( 0.000000000000000000, -0.8910065241883627918, -0.4539904997395570185 ) ) ;
#23577 = DIRECTION ( 'NONE',  ( 0.9435911131814398445, -0.3311129884571295534, 0.000000000000000000 ) ) ;
#23578 = ADVANCED_FACE ( 'NONE', ( #21674 ), #36594, .T. ) ;
#23579 = LINE ( 'NONE', #4281, #30914 ) ;
#23580 = CARTESIAN_POINT ( 'NONE',  ( -23.54415474984308787, -120.4156646670583086, 5.500000000000000000 ) ) ;
#23581 = LINE ( 'NONE', #20892, #557 ) ;
#23582 = EDGE_CURVE ( 'NONE', #22554, #43090, #3058, .T. ) ;
#23583 = CARTESIAN_POINT ( 'NONE',  ( 10.00000000000000000, -74.65374052328644439, -8.840884882375878107 ) ) ;
#23584 = FACE_BOUND ( 'NONE', #15219, .T. ) ;
#23585 = EDGE_CURVE ( 'NONE', #29746, #24479, #6501, .T. ) ;
#23586 = ORIENTED_EDGE ( 'NONE', *, *, #14085, .T. ) ;
#23587 = AXIS2_PLACEMENT_3D ( 'NONE', #11675, #19474, #45438 ) ;
#23588 = EDGE_LOOP ( 'NONE', ( #44229, #12148, #34481, #39472 ) ) ;
#23589 = CARTESIAN_POINT ( 'NONE',  ( 10.00000000000000000, 0.000000000000000000, 0.000000000000000000 ) ) ;
#23590 = AXIS2_PLACEMENT_3D ( 'NONE', #20136, #23325, #27249 ) ;
#23591 = EDGE_LOOP ( 'NONE', ( #33923, #35459, #19434, #3569 ) ) ;
#23592 = ORIENTED_EDGE ( 'NONE', *, *, #45786, .T. ) ;
#23593 = CYLINDRICAL_SURFACE ( 'NONE', #44061, 37.49900000000000233 ) ;
#23594 = AXIS2_PLACEMENT_3D ( 'NONE', #13512, #28439, #31167 ) ;
#23595 = CIRCLE ( 'NONE', #36868, 77.49900000000000944 ) ;
#23596 = DIRECTION ( 'NONE',  ( 0.000000000000000000, 0.000000000000000000, 1.000000000000000000 ) ) ;
#23597 = CIRCLE ( 'NONE', #15014, 82.00000000000000000 ) ;
#23598 = ORIENTED_EDGE ( 'NONE', *, *, #18817, .F. ) ;
#23599 = EDGE_CURVE ( 'NONE', #41810, #8149, #43479, .T. ) ;
#23600 = EDGE_CURVE ( 'NONE', #21412, #45983, #12130, .T. ) ;
#23601 = EDGE_CURVE ( 'NONE', #15144, #12730, #13367, .T. ) ;
#23602 = VERTEX_POINT ( 'NONE', #32218 ) ;
#23603 = AXIS2_PLACEMENT_3D ( 'NONE', #31055, #16350, #12930 ) ;
#23604 = ORIENTED_EDGE ( 'NONE', *, *, #23886, .F. ) ;
#23605 = VERTEX_POINT ( 'NONE', #40041 ) ;
#23606 = ORIENTED_EDGE ( 'NONE', *, *, #16403, .F. ) ;
#23607 = EDGE_CURVE ( 'NONE', #29157, #42296, #19924, .T. ) ;
#23608 = DIRECTION ( 'NONE',  ( 0.3853207896976547087, -0.9227826878668540234, 0.000000000000000000 ) ) ;
#23609 = DIRECTION ( 'NONE',  ( 0.000000000000000000, 0.8090169943749445647, 0.5877852522924770229 ) ) ;
#23610 = CARTESIAN_POINT ( 'NONE',  ( -15.44521549751111422, -137.7748507232956001, -5.500000000000000000 ) ) ;
#23611 = ORIENTED_EDGE ( 'NONE', *, *, #16492, .F. ) ;
#23612 = CARTESIAN_POINT ( 'NONE',  ( 0.000000000000000000, 0.000000000000000000, 0.000000000000000000 ) ) ;
#23613 = ORIENTED_EDGE ( 'NONE', *, *, #19399, .F. ) ;
#23614 = ORIENTED_EDGE ( 'NONE', *, *, #20834, .F. ) ;
#23615 = DIRECTION ( 'NONE',  ( 1.000000000000000000, 0.000000000000000000, 0.000000000000000000 ) ) ;
#23616 = DIRECTION ( 'NONE',  ( -1.000000000000000000, 0.000000000000000000, -0.000000000000000000 ) ) ;
#23617 = DIRECTION ( 'NONE',  ( 0.000000000000000000, 0.000000000000000000, 1.000000000000000000 ) ) ;
#23618 = CIRCLE ( 'NONE', #4063, 82.00000000000000000 ) ;
#23619 = ORIENTED_EDGE ( 'NONE', *, *, #47557, .F. ) ;
#23620 = ORIENTED_EDGE ( 'NONE', *, *, #382, .F. ) ;
#23621 = FACE_OUTER_BOUND ( 'NONE', #29167, .T. ) ;
#23622 = ORIENTED_EDGE ( 'NONE', *, *, #5477, .F. ) ;
#23623 = AXIS2_PLACEMENT_3D ( 'NONE', #20803, #38699, #12988 ) ;
#23624 = DIRECTION ( 'NONE',  ( 0.000000000000000000, 0.000000000000000000, 1.000000000000000000 ) ) ;
#23625 = DIRECTION ( 'NONE',  ( -0.1850432970638667129, 0.9827303690289281857, 0.000000000000000000 ) ) ;
#23626 = FACE_OUTER_BOUND ( 'NONE', #21204, .T. ) ;
#23627 = DIRECTION ( 'NONE',  ( -1.000000000000000000, -0.000000000000000000, -0.000000000000000000 ) ) ;
#23628 = CARTESIAN_POINT ( 'NONE',  ( 0.000000000000000000, -71.87247863392384772, -39.47590169984923136 ) ) ;
#23629 = DIRECTION ( 'NONE',  ( 1.000000000000000000, 0.000000000000000000, -0.000000000000000000 ) ) ;
#23630 = CIRCLE ( 'NONE', #19733, 82.00000000000000000 ) ;
#23631 = FACE_OUTER_BOUND ( 'NONE', #44782, .T. ) ;
#23632 = CARTESIAN_POINT ( 'NONE',  ( 0.000000000000000000, -17.80606268964516659, -33.00180498840066434 ) ) ;
#23633 = CARTESIAN_POINT ( 'NONE',  ( 10.00000000000000000, 28.89263327155850902, -71.91182617369157981 ) ) ;
#23634 = DIRECTION ( 'NONE',  ( -0.000000000000000000, -0.000000000000000000, -1.000000000000000000 ) ) ;
#23635 = CYLINDRICAL_SURFACE ( 'NONE', #17588, 31.99999999999998579 ) ;
#23636 = ORIENTED_EDGE ( 'NONE', *, *, #23042, .F. ) ;
#23637 = ORIENTED_EDGE ( 'NONE', *, *, #47416, .F. ) ;
#23638 = SURFACE_STYLE_FILL_AREA ( #13123 ) ;
#23639 = CIRCLE ( 'NONE', #45504, 37.49900000000001654 ) ;
#23640 = EDGE_CURVE ( 'NONE', #41545, #45965, #9937, .T. ) ;
#23641 = CARTESIAN_POINT ( 'NONE',  ( 0.000000000000000000, 0.000000000000000000, 0.000000000000000000 ) ) ;
#23642 = DIRECTION ( 'NONE',  ( 0.000000000000000000, 0.000000000000000000, 1.000000000000000000 ) ) ;
#23643 = DIRECTION ( 'NONE',  ( 0.000000000000000000, 0.000000000000000000, 1.000000000000000000 ) ) ;
#23644 = EDGE_CURVE ( 'NONE', #3739, #17812, #46501, .T. ) ;
#23645 = ADVANCED_FACE ( 'NONE', ( #24378 ), #32680, .T. ) ;
#23646 = CARTESIAN_POINT ( 'NONE',  ( 10.00000000000000000, -41.91543099594819921, 2.663952781846001816 ) ) ;
#23647 = CARTESIAN_POINT ( 'NONE',  ( 0.000000000000000000, 2.946379043147425492, -75.11764819372145041 ) ) ;
#23648 = ADVANCED_FACE ( 'NONE', ( #14083 ), #10411, .T. ) ;
#23649 = FACE_OUTER_BOUND ( 'NONE', #24173, .T. ) ;
#23650 = DIRECTION ( 'NONE',  ( 0.000000000000000000, 0.000000000000000000, 1.000000000000000000 ) ) ;
#23652 = EDGE_CURVE ( 'NONE', #42694, #551, #24629, .T. ) ;
#23651 = VERTEX_POINT ( 'NONE', #9684 ) ;
#23653 = VERTEX_POINT ( 'NONE', #25809 ) ;
#23654 = VECTOR ( 'NONE', #15004, 1000.000000000000114 ) ;
#23655 = CARTESIAN_POINT ( 'NONE',  ( 0.000000000000000000, -68.26794271651286294, 31.47745569255117104 ) ) ;
#23656 = ORIENTED_EDGE ( 'NONE', *, *, #1437, .F. ) ;
#23657 = EDGE_CURVE ( 'NONE', #19570, #25110, #11397, .T. ) ;
#23658 = VECTOR ( 'NONE', #40688, 1000.000000000000000 ) ;
#23659 = AXIS2_PLACEMENT_3D ( 'NONE', #19698, #19955, #1854 ) ;
#23660 = ORIENTED_EDGE ( 'NONE', *, *, #39061, .T. ) ;
#23661 = ORIENTED_EDGE ( 'NONE', *, *, #47124, .F. ) ;
#23662 = EDGE_CURVE ( 'NONE', #30137, #7347, #2735, .T. ) ;
#23663 = VERTEX_POINT ( 'NONE', #14815 ) ;
#23664 = AXIS2_PLACEMENT_3D ( 'NONE', #8514, #45980, #12445 ) ;
#23665 = CIRCLE ( 'NONE', #31515, 82.00000000000000000 ) ;
#23666 = CARTESIAN_POINT ( 'NONE',  ( 22.94323693612312809, -114.6983135802921083, 2.500000000000000000 ) ) ;
#23667 = VERTEX_POINT ( 'NONE', #44913 ) ;
#23668 = AXIS2_PLACEMENT_3D ( 'NONE', #13417, #20998, #25142 ) ;
#23669 = EDGE_CURVE ( 'NONE', #18905, #1468, #7219, .T. ) ;
#23670 = VECTOR ( 'NONE', #33623, 1000.000000000000000 ) ;
#23671 = CARTESIAN_POINT ( 'NONE',  ( 10.00000000000000000, -74.65491531819111515, 23.16904090965678975 ) ) ;
#23672 = AXIS2_PLACEMENT_3D ( 'NONE', #40292, #25575, #15309 ) ;
#23673 = LINE ( 'NONE', #11286, #41740 ) ;
#23674 = ORIENTED_EDGE ( 'NONE', *, *, #8142, .F. ) ;
#23675 = CARTESIAN_POINT ( 'NONE',  ( 10.00000000000000000, 65.59268652807263322, -36.72794159290169347 ) ) ;
#23676 = DIRECTION ( 'NONE',  ( -1.000000000000000000, -0.000000000000000000, -0.000000000000000000 ) ) ;
#23677 = EDGE_CURVE ( 'NONE', #31653, #14555, #44188, .T. ) ;
#23678 = DIRECTION ( 'NONE',  ( -1.000000000000000000, -0.000000000000000000, -0.000000000000000000 ) ) ;
#23679 = ORIENTED_EDGE ( 'NONE', *, *, #38868, .F. ) ;
#23680 = DIRECTION ( 'NONE',  ( 0.000000000000000000, -0.7071067811865536790, 0.7071067811865414665 ) ) ;
#23681 = EDGE_LOOP ( 'NONE', ( #20162, #19949, #22553, #13971 ) ) ;
#23682 = ORIENTED_EDGE ( 'NONE', *, *, #44199, .F. ) ;
#23683 = DIRECTION ( 'NONE',  ( -1.000000000000000000, 0.000000000000000000, 0.000000000000000000 ) ) ;
#23684 = CARTESIAN_POINT ( 'NONE',  ( 10.00000000000000000, 20.40083707022882820, 72.35432306680490910 ) ) ;
#23685 = ORIENTED_EDGE ( 'NONE', *, *, #45820, .T. ) ;
#23686 = CARTESIAN_POINT ( 'NONE',  ( 10.00000000000000000, -22.74946021919153694, 29.81001611431000597 ) ) ;
#23687 = LINE ( 'NONE', #9720, #44794 ) ;
#23688 = CIRCLE ( 'NONE', #15869, 77.49900000000000944 ) ;
#23689 = CARTESIAN_POINT ( 'NONE',  ( 10.00000000000000000, -18.89407956138310496, 75.16055320797023853 ) ) ;
#23690 = ORIENTED_EDGE ( 'NONE', *, *, #45847, .T. ) ;
#23691 = AXIS2_PLACEMENT_3D ( 'NONE', #32566, #17144, #31870 ) ;
#23692 = DIRECTION ( 'NONE',  ( 0.000000000000000000, 0.000000000000000000, 1.000000000000000000 ) ) ;
#23693 = CARTESIAN_POINT ( 'NONE',  ( 0.000000000000000000, -77.32052557432845674, 5.256550761632577284 ) ) ;
#23694 = VERTEX_POINT ( 'NONE', #44428 ) ;
#23695 = EDGE_CURVE ( 'NONE', #1711, #19709, #21899, .T. ) ;
#23696 = CYLINDRICAL_SURFACE ( 'NONE', #11628, 16.00000000000000000 ) ;
#23697 = ORIENTED_EDGE ( 'NONE', *, *, #29993, .T. ) ;
#23698 = AXIS2_PLACEMENT_3D ( 'NONE', #16785, #27321, #23389 ) ;
#23699 = CIRCLE ( 'NONE', #33857, 31.99999999999998224 ) ;
#23700 = LINE ( 'NONE', #34958, #12913 ) ;
#23701 = AXIS2_PLACEMENT_3D ( 'NONE', #39838, #44461, #25370 ) ;
#23702 = CARTESIAN_POINT ( 'NONE',  ( 5.000000000000002665, -81.34940948281328588, -10.30890764327469711 ) ) ;
#23703 = DIRECTION ( 'NONE',  ( -1.000000000000000000, 0.000000000000000000, -0.000000000000000000 ) ) ;
#23704 = DIRECTION ( 'NONE',  ( 0.000000000000000000, 0.000000000000000000, -1.000000000000000000 ) ) ;
#23705 = CIRCLE ( 'NONE', #1838, 77.49899999999999523 ) ;
#23706 = EDGE_CURVE ( 'NONE', #14949, #43486, #26316, .T. ) ;
#23707 = DIRECTION ( 'NONE',  ( 0.000000000000000000, 0.6494480483301793283, 0.7604059656000345946 ) ) ;
#23708 = LINE ( 'NONE', #19307, #25551 ) ;
#23709 = VECTOR ( 'NONE', #48047, 1000.000000000000000 ) ;
#23710 = VECTOR ( 'NONE', #46598, 1000.000000000000000 ) ;
#23711 = LINE ( 'NONE', #1689, #15391 ) ;
#23712 = DIRECTION ( 'NONE',  ( -1.000000000000000000, -0.000000000000000000, -0.000000000000000000 ) ) ;
#23713 = EDGE_CURVE ( 'NONE', #36455, #4586, #21508, .T. ) ;
#23714 = CIRCLE ( 'NONE', #25271, 77.49899999999999523 ) ;
#23715 = CARTESIAN_POINT ( 'NONE',  ( -21.67772167707813935, -110.8034581014852762, 5.500000000000000000 ) ) ;
#23716 = VECTOR ( 'NONE', #2079, 1000.000000000000000 ) ;
#23717 = ORIENTED_EDGE ( 'NONE', *, *, #13798, .T. ) ;
#23718 = DIRECTION ( 'NONE',  ( -1.000000000000000000, 0.000000000000000000, 0.000000000000000000 ) ) ;
#23719 = EDGE_LOOP ( 'NONE', ( #23489, #8593, #22875, #1730 ) ) ;
#23720 = DIRECTION ( 'NONE',  ( 0.000000000000000000, 0.000000000000000000, 1.000000000000000000 ) ) ;
#23721 = DIRECTION ( 'NONE',  ( 1.000000000000000000, 0.000000000000000000, 0.000000000000000000 ) ) ;
#23722 = ORIENTED_EDGE ( 'NONE', *, *, #11878, .F. ) ;
#23723 = VECTOR ( 'NONE', #23237, 1000.000000000000000 ) ;
#23724 = DIRECTION ( 'NONE',  ( 0.000000000000000000, 0.000000000000000000, -1.000000000000000000 ) ) ;
#23725 = AXIS2_PLACEMENT_3D ( 'NONE', #33153, #7453, #7920 ) ;
#23726 = CIRCLE ( 'NONE', #38599, 77.49899999999999523 ) ;
#23728 = ORIENTED_EDGE ( 'NONE', *, *, #15979, .F. ) ;
#23727 = CIRCLE ( 'NONE', #22931, 42.00000000000000000 ) ;
#23729 = ORIENTED_EDGE ( 'NONE', *, *, #41308, .F. ) ;
#23730 = ORIENTED_EDGE ( 'NONE', *, *, #7285, .T. ) ;
#23731 = ORIENTED_EDGE ( 'NONE', *, *, #32752, .T. ) ;
#23732 = CARTESIAN_POINT ( 'NONE',  ( 10.00000000000000000, 35.91791733033570466, -68.67312586194960033 ) ) ;
#23733 = ORIENTED_EDGE ( 'NONE', *, *, #14091, .F. ) ;
#23734 = CIRCLE ( 'NONE', #37015, 82.00000000000000000 ) ;
#23735 = VECTOR ( 'NONE', #7465, 1000.000000000000000 ) ;
#23736 = ORIENTED_EDGE ( 'NONE', *, *, #29464, .F. ) ;
#23737 = LINE ( 'NONE', #16399, #6734 ) ;
#23738 = ORIENTED_EDGE ( 'NONE', *, *, #20289, .F. ) ;
#23739 = CIRCLE ( 'NONE', #42518, 31.99999999999998224 ) ;
#23740 = CARTESIAN_POINT ( 'NONE',  ( 4.250000000000000000, -13.95926121303099343, 0.000000000000000000 ) ) ;
#23741 = VECTOR ( 'NONE', #26928, 1000.000000000000000 ) ;
#23742 = DIRECTION ( 'NONE',  ( 0.000000000000000000, 0.000000000000000000, 1.000000000000000000 ) ) ;
#23743 = DIRECTION ( 'NONE',  ( 1.000000000000000000, -0.000000000000000000, -0.000000000000000000 ) ) ;
#23745 = VERTEX_POINT ( 'NONE', #18945 ) ;
#23744 = AXIS2_PLACEMENT_3D ( 'NONE', #7663, #15016, #26512 ) ;
#23746 = DIRECTION ( 'NONE',  ( -1.000000000000000000, -0.000000000000000000, -0.000000000000000000 ) ) ;
#23747 = ORIENTED_EDGE ( 'NONE', *, *, #28789, .T. ) ;
#23748 = CARTESIAN_POINT ( 'NONE',  ( 0.000000000000000000, 6.903761155837791819, 77.19088730480525840 ) ) ;
#23749 = CARTESIAN_POINT ( 'NONE',  ( 0.000000000000000000, 46.11716303203188261, 67.80270845531904911 ) ) ;
#23750 = ORIENTED_EDGE ( 'NONE', *, *, #47425, .F. ) ;
#23751 = DIRECTION ( 'NONE',  ( -1.000000000000000000, 0.000000000000000000, -0.000000000000000000 ) ) ;
#23752 = EDGE_LOOP ( 'NONE', ( #7496, #19337, #1656, #20149 ) ) ;
#23753 = EDGE_LOOP ( 'NONE', ( #6691, #12193, #4176, #15064 ) ) ;
#23754 = ADVANCED_FACE ( 'NONE', ( #33640 ), #7702, .T. ) ;
#23755 = LINE ( 'NONE', #35013, #10380 ) ;
#23756 = CARTESIAN_POINT ( 'NONE',  ( 0.000000000000000000, -0.8299999999999999600, -1.199999999999999956 ) ) ;
#23757 = CARTESIAN_POINT ( 'NONE',  ( 11.99999999999999822, 41.19522573413826194, -65.64334221924865176 ) ) ;
#23758 = DIRECTION ( 'NONE',  ( 0.000000000000000000, -0.2079116908177532363, 0.9781476007338069101 ) ) ;
#23759 = DIRECTION ( 'NONE',  ( 0.7950889364178796992, -0.6064928550163511956, 0.000000000000000000 ) ) ;
#23760 = EDGE_CURVE ( 'NONE', #5341, #20027, #27780, .T. ) ;
#23761 = CARTESIAN_POINT ( 'NONE',  ( 0.000000000000000000, 22.48208911017551515, -35.47612816024499693 ) ) ;
#23762 = DIRECTION ( 'NONE',  ( -0.000000000000000000, -0.000000000000000000, -1.000000000000000000 ) ) ;
#23763 = AXIS2_PLACEMENT_3D ( 'NONE', #10477, #21960, #33703 ) ;
#23764 = PLANE ( 'NONE',  #47403 ) ;
#23765 = VECTOR ( 'NONE', #30883, 1000.000000000000000 ) ;
#23766 = CARTESIAN_POINT ( 'NONE',  ( 16.84844760790522855, -103.5491698323862124, 5.500000000000000000 ) ) ;
#23767 = DIRECTION ( 'NONE',  ( 0.8774505977381978905, 0.4796670183876304283, -0.000000000000000000 ) ) ;
#23768 = CARTESIAN_POINT ( 'NONE',  ( 10.00000000000000000, 70.53064760720316428, -26.01480285779861035 ) ) ;
#23769 = EDGE_CURVE ( 'NONE', #26989, #18327, #29259, .T. ) ;
#23770 = VECTOR ( 'NONE', #38271, 1000.000000000000114 ) ;
#23771 = AXIS2_PLACEMENT_3D ( 'NONE', #38827, #5287, #39286 ) ;
#23772 = AXIS2_PLACEMENT_3D ( 'NONE', #48332, #14812, #25325 ) ;
#23773 = ADVANCED_FACE ( 'NONE', ( #110 ), #25573, .T. ) ;
#23774 = DIRECTION ( 'NONE',  ( 0.000000000000000000, 0.000000000000000000, 1.000000000000000000 ) ) ;
#23775 = CARTESIAN_POINT ( 'NONE',  ( 10.00000000000000000, 27.05870788708231700, 26.08949754953034272 ) ) ;
#23776 = LINE ( 'NONE', #46295, #1395 ) ;
#23777 = CARTESIAN_POINT ( 'NONE',  ( -11.99999999999999645, 1.702802944658382841E-15, 13.90444123027096879 ) ) ;
#23778 = VERTEX_POINT ( 'NONE', #10900 ) ;
#23779 = VERTEX_POINT ( 'NONE', #18483 ) ;
#23781 = CARTESIAN_POINT ( 'NONE',  ( 0.000000000000000000, -9.188173127307001309, -40.98264845739759465 ) ) ;
#23780 = AXIS2_PLACEMENT_3D ( 'NONE', #7534, #32977, #37142 ) ;
#23782 = AXIS2_PLACEMENT_3D ( 'NONE', #14997, #44603, #29187 ) ;
#23783 = ORIENTED_EDGE ( 'NONE', *, *, #18091, .F. ) ;
#23784 = AXIS2_PLACEMENT_3D ( 'NONE', #18339, #33020, #37188 ) ;
#23785 = CARTESIAN_POINT ( 'NONE',  ( 10.00000000000000000, 31.47745569255237896, -68.26794271651228030 ) ) ;
#23786 = VECTOR ( 'NONE', #27909, 999.9999999999998863 ) ;
#23787 = PRODUCT_CONTEXT ( 'NONE', #3183, 'mechanical' ) ;
#23788 = CARTESIAN_POINT ( 'NONE',  ( 10.00000000000000000, 37.48860685352291000, -0.8828120875901940279 ) ) ;
#23789 = VECTOR ( 'NONE', #5524, 1000.000000000000000 ) ;
#23790 = ORIENTED_EDGE ( 'NONE', *, *, #12761, .F. ) ;
#23791 = EDGE_CURVE ( 'NONE', #4718, #25973, #48334, .T. ) ;
#23792 = DIRECTION ( 'NONE',  ( -1.000000000000000000, 0.000000000000000000, 0.000000000000000000 ) ) ;
#23793 = ORIENTED_EDGE ( 'NONE', *, *, #11221, .T. ) ;
#23794 = CIRCLE ( 'NONE', #8947, 16.00000000000000000 ) ;
#23795 = CARTESIAN_POINT ( 'NONE',  ( -10.00000000000000000, 0.000000000000000000, 0.000000000000000000 ) ) ;
#23796 = EDGE_LOOP ( 'NONE', ( #36618, #34504, #12864, #30015 ) ) ;
#23797 = CIRCLE ( 'NONE', #41770, 31.99999999999998224 ) ;
#23798 = EDGE_CURVE ( 'NONE', #18377, #39100, #29979, .T. ) ;
#23799 = CARTESIAN_POINT ( 'NONE',  ( -10.00000000000000000, 0.000000000000000000, 0.000000000000000000 ) ) ;
#23800 = DIRECTION ( 'NONE',  ( -1.000000000000000000, 0.000000000000000000, 0.000000000000000000 ) ) ;
#23801 = ORIENTED_EDGE ( 'NONE', *, *, #5428, .F. ) ;
#23803 = VERTEX_POINT ( 'NONE', #37563 ) ;
#23802 = CARTESIAN_POINT ( 'NONE',  ( 0.000000000000000000, -41.76937507738745836, -62.50329211542482710 ) ) ;
#23804 = AXIS2_PLACEMENT_3D ( 'NONE', #7933, #30703, #4522 ) ;
#23805 = EDGE_CURVE ( 'NONE', #44086, #33547, #24655, .T. ) ;
#23806 = EDGE_LOOP ( 'NONE', ( #45202, #15872, #9050, #981 ) ) ;
#23807 = CARTESIAN_POINT ( 'NONE',  ( -13.05994868825747446, -139.5943292883446532, -5.500000000000000000 ) ) ;
#23808 = ADVANCED_FACE ( 'NONE', ( #2255 ), #36507, .T. ) ;
#23809 = FACE_OUTER_BOUND ( 'NONE', #2547, .T. ) ;
#23810 = DIRECTION ( 'NONE',  ( 0.000000000000000000, -0.3090169943749548342, 0.9510565162951510887 ) ) ;
#23811 = LINE ( 'NONE', #19632, #29844 ) ;
#23813 = ORIENTED_EDGE ( 'NONE', *, *, #9541, .T. ) ;
#23812 = LINE ( 'NONE', #323, #749 ) ;
#23814 = CIRCLE ( 'NONE', #40244, 77.49900000000000944 ) ;
#23815 = AXIS2_PLACEMENT_3D ( 'NONE', #17145, #24745, #35755 ) ;
#23816 = EDGE_LOOP ( 'NONE', ( #3857, #13909, #45607, #21296 ) ) ;
#23817 = DIRECTION ( 'NONE',  ( -1.000000000000000000, 0.000000000000000000, 0.000000000000000000 ) ) ;
#23818 = VERTEX_POINT ( 'NONE', #32370 ) ;
#23819 = ORIENTED_EDGE ( 'NONE', *, *, #16872, .T. ) ;
#23820 = CIRCLE ( 'NONE', #18320, 12.49999999999999645 ) ;
#23821 = DIRECTION ( 'NONE',  ( -1.000000000000000000, 0.000000000000000000, 0.000000000000000000 ) ) ;
#23822 = CIRCLE ( 'NONE', #44804, 31.99999999999999289 ) ;
#23823 = CARTESIAN_POINT ( 'NONE',  ( 0.000000000000000000, -37.58145647212455032, 0.6853352020789044152 ) ) ;
#23824 = CIRCLE ( 'NONE', #30079, 16.00000000000000000 ) ;
#23825 = CYLINDRICAL_SURFACE ( 'NONE', #18801, 77.49899999999999523 ) ;
#23826 = CARTESIAN_POINT ( 'NONE',  ( 15.00000000000000000, -18.13022148937242761, 15.02647892043569122 ) ) ;
#23827 = ORIENTED_EDGE ( 'NONE', *, *, #17606, .T. ) ;
#23828 = CARTESIAN_POINT ( 'NONE',  ( -11.70000000000000107, 0.000000000000000000, 0.000000000000000000 ) ) ;
#23829 = EDGE_CURVE ( 'NONE', #46921, #14358, #10576, .T. ) ;
#23830 = CIRCLE ( 'NONE', #19140, 82.00000000000000000 ) ;
#23831 = CARTESIAN_POINT ( 'NONE',  ( 0.000000000000000000, -75.11725578898466438, -2.956366410621452001 ) ) ;
#23832 = EDGE_CURVE ( 'NONE', #33124, #9519, #11393, .T. ) ;
#23833 = EDGE_CURVE ( 'NONE', #27870, #15338, #45765, .T. ) ;
#23834 = CARTESIAN_POINT ( 'NONE',  ( 11.99999999999999822, -81.50828551894220197, -8.966570791701590437 ) ) ;
#23835 = FACE_OUTER_BOUND ( 'NONE', #1336, .T. ) ;
#23836 = DIRECTION ( 'NONE',  ( -0.000000000000000000, -0.000000000000000000, 1.000000000000000000 ) ) ;
#23837 = DIRECTION ( 'NONE',  ( -1.000000000000000000, 0.000000000000000000, 0.000000000000000000 ) ) ;
#23838 = CARTESIAN_POINT ( 'NONE',  ( 10.00000000000000000, 21.32104025579158701, -30.84782396557194772 ) ) ;
#23839 = DIRECTION ( 'NONE',  ( 0.9918136447140100120, -0.1276937514489704939, 0.000000000000000000 ) ) ;
#23840 = ORIENTED_EDGE ( 'NONE', *, *, #19269, .F. ) ;
#23841 = DIRECTION ( 'NONE',  ( 0.000000000000000000, 0.9510565162951503115, 0.3090169943749573878 ) ) ;
#23842 = CARTESIAN_POINT ( 'NONE',  ( 10.00000000000000000, 59.03342792756263435, 46.54456581323825048 ) ) ;
#23843 = ORIENTED_EDGE ( 'NONE', *, *, #12554, .T. ) ;
#23844 = AXIS2_PLACEMENT_3D ( 'NONE', #42310, #38894, #46720 ) ;
#23845 = DIRECTION ( 'NONE',  ( 0.000000000000000000, 0.000000000000000000, 1.000000000000000000 ) ) ;
#23846 = VERTEX_POINT ( 'NONE', #6181 ) ;
#23847 = DIRECTION ( 'NONE',  ( -1.000000000000000000, 0.000000000000000000, 0.000000000000000000 ) ) ;
#23848 = CARTESIAN_POINT ( 'NONE',  ( 0.000000000000000000, 20.41045688087824317, 72.35160999960824313 ) ) ;
#23849 = ORIENTED_EDGE ( 'NONE', *, *, #11233, .F. ) ;
#23850 = CIRCLE ( 'NONE', #40283, 31.99999999999998934 ) ;
#23851 = VECTOR ( 'NONE', #33414, 1000.000000000000000 ) ;
#23852 = CIRCLE ( 'NONE', #46542, 16.00000000000000000 ) ;
#23853 = ORIENTED_EDGE ( 'NONE', *, *, #35759, .F. ) ;
#23854 = ORIENTED_EDGE ( 'NONE', *, *, #19993, .T. ) ;
#23855 = ORIENTED_EDGE ( 'NONE', *, *, #18980, .T. ) ;
#23856 = AXIS2_PLACEMENT_3D ( 'NONE', #19695, #4791, #23624 ) ;
#23857 = ADVANCED_FACE ( 'NONE', ( #21814 ), #17665, .T. ) ;
#23858 = DIRECTION ( 'NONE',  ( 0.9997280174009349762, -0.02332147558787674158, 0.000000000000000000 ) ) ;
#23859 = ORIENTED_EDGE ( 'NONE', *, *, #19482, .F. ) ;
#23860 = DIRECTION ( 'NONE',  ( -0.08130631524009862554, 0.9966891607226787686, 0.000000000000000000 ) ) ;
#23861 = DIRECTION ( 'NONE',  ( -1.000000000000000000, -0.000000000000000000, -0.000000000000000000 ) ) ;
#23862 = EDGE_CURVE ( 'NONE', #20052, #24067, #26229, .T. ) ;
#23863 = EDGE_LOOP ( 'NONE', ( #6708, #45515, #34859, #13567 ) ) ;
#23864 = CARTESIAN_POINT ( 'NONE',  ( 10.00000000000000000, -29.81001611431024756, 22.74946021919122785 ) ) ;
#23865 = ORIENTED_EDGE ( 'NONE', *, *, #14878, .F. ) ;
#23866 = EDGE_CURVE ( 'NONE', #17444, #43536, #25404, .T. ) ;
#23867 = VERTEX_POINT ( 'NONE', #2733 ) ;
#23868 = DIRECTION ( 'NONE',  ( 0.000000000000000000, 0.000000000000000000, 1.000000000000000000 ) ) ;
#23869 = LINE ( 'NONE', #38817, #14543 ) ;
#23870 = CARTESIAN_POINT ( 'NONE',  ( 0.000000000000000000, 36.88895765772642221, -6.736453364083161865 ) ) ;
#23871 = AXIS2_PLACEMENT_3D ( 'NONE', #37793, #23837, #4513 ) ;
#23872 = ORIENTED_EDGE ( 'NONE', *, *, #31330, .F. ) ;
#23873 = ORIENTED_EDGE ( 'NONE', *, *, #25333, .F. ) ;
#23874 = EDGE_LOOP ( 'NONE', ( #3185, #2264, #33017, #1308 ) ) ;
#23875 = DIRECTION ( 'NONE',  ( 1.000000000000000000, 0.000000000000000000, 0.000000000000000000 ) ) ;
#23876 = ORIENTED_EDGE ( 'NONE', *, *, #39431, .T. ) ;
#23877 = CARTESIAN_POINT ( 'NONE',  ( 10.00000000000000000, 0.000000000000000000, 0.000000000000000000 ) ) ;
#23878 = CARTESIAN_POINT ( 'NONE',  ( 0.000000000000000000, -26.23277895567251505, 4.042438405569750870 ) ) ;
#23879 = DIRECTION ( 'NONE',  ( -1.000000000000000000, -0.000000000000000000, 0.000000000000000000 ) ) ;
#23880 = CARTESIAN_POINT ( 'NONE',  ( 10.00000000000000000, 77.32052557432841411, 5.256550761633138613 ) ) ;
#23881 = CARTESIAN_POINT ( 'NONE',  ( 10.00000000000000000, 0.000000000000000000, 0.000000000000000000 ) ) ;
#23882 = CARTESIAN_POINT ( 'NONE',  ( 0.000000000000000000, 0.000000000000000000, 0.000000000000000000 ) ) ;
#23883 = DIRECTION ( 'NONE',  ( -0.000000000000000000, 0.5877852522924696954, 0.8090169943749498938 ) ) ;
#23884 = ADVANCED_FACE ( 'NONE', ( #39479 ), #5953, .T. ) ;
#23885 = ORIENTED_EDGE ( 'NONE', *, *, #10328, .F. ) ;
#23886 = EDGE_CURVE ( 'NONE', #44567, #38630, #10578, .T. ) ;
#23887 = DIRECTION ( 'NONE',  ( 0.000000000000000000, 0.000000000000000000, -1.000000000000000000 ) ) ;
#23888 = LINE ( 'NONE', #24130, #26942 ) ;
#23889 = DIRECTION ( 'NONE',  ( -1.000000000000000000, 0.000000000000000000, 0.000000000000000000 ) ) ;
#23890 = DIRECTION ( 'NONE',  ( 0.000000000000000000, 0.9510565162951521989, 0.3090169943749515591 ) ) ;
#23891 = CIRCLE ( 'NONE', #2774, 82.00000000000000000 ) ;
#23892 = VERTEX_POINT ( 'NONE', #10315 ) ;
#23893 = ORIENTED_EDGE ( 'NONE', *, *, #4266, .T. ) ;
#23894 = CARTESIAN_POINT ( 'NONE',  ( 11.99999999999999822, -41.76106447765533147, 62.50884508063410294 ) ) ;
#23895 = AXIS2_PLACEMENT_3D ( 'NONE', #16731, #30690, #27270 ) ;
#23896 = FACE_OUTER_BOUND ( 'NONE', #26204, .T. ) ;
#23897 = CARTESIAN_POINT ( 'NONE',  ( 5.999999999999999112, 51.29473840253317007, -63.97538442413369353 ) ) ;
#23898 = CIRCLE ( 'NONE', #29378, 31.99999999999999645 ) ;
#23899 = AXIS2_PLACEMENT_3D ( 'NONE', #9063, #35961, #5632 ) ;
#23900 = FACE_OUTER_BOUND ( 'NONE', #33959, .T. ) ;
#23901 = FACE_OUTER_BOUND ( 'NONE', #33724, .T. ) ;
#23902 = EDGE_CURVE ( 'NONE', #21501, #44761, #28203, .T. ) ;
#23903 = VERTEX_POINT ( 'NONE', #2490 ) ;
#23904 = AXIS2_PLACEMENT_3D ( 'NONE', #6204, #13793, #2992 ) ;
#23905 = CARTESIAN_POINT ( 'NONE',  ( 11.99999999999999822, -70.53064760720297954, -26.01480285779911839 ) ) ;
#23906 = LINE ( 'NONE', #2572, #12052 ) ;
#23907 = VERTEX_POINT ( 'NONE', #35792 ) ;
#23908 = AXIS2_PLACEMENT_3D ( 'NONE', #23377, #27797, #42722 ) ;
#23909 = ORIENTED_EDGE ( 'NONE', *, *, #41476, .F. ) ;
#23910 = SHAPE_REPRESENTATION_RELATIONSHIP ( 'NONE' , 'NONE' ,  #21223, #27490 ) ;
#23911 = AXIS2_PLACEMENT_3D ( 'NONE', #27494, #24286, #31169 ) ;
#23912 = DIRECTION ( 'NONE',  ( -1.000000000000000000, 0.000000000000000000, 0.000000000000000000 ) ) ;
#23913 = ORIENTED_EDGE ( 'NONE', *, *, #48173, .F. ) ;
#23914 = CONICAL_SURFACE ( 'NONE', #27845, 13.71319123027096865, 1.361356816555593596 ) ;
#23915 = VERTEX_POINT ( 'NONE', #43144 ) ;
#23916 = ORIENTED_EDGE ( 'NONE', *, *, #34576, .T. ) ;
#23917 = CARTESIAN_POINT ( 'NONE',  ( 0.000000000000000000, 0.000000000000000000, 0.000000000000000000 ) ) ;
#23918 = VERTEX_POINT ( 'NONE', #6660 ) ;
#23919 = EDGE_LOOP ( 'NONE', ( #3691, #46187, #21385, #38565 ) ) ;
#23920 = VECTOR ( 'NONE', #37289, 1000.000000000000114 ) ;
#23921 = DIRECTION ( 'NONE',  ( -1.000000000000000000, 0.000000000000000000, 0.000000000000000000 ) ) ;
#23923 = ORIENTED_EDGE ( 'NONE', *, *, #22873, .T. ) ;
#23922 = DIRECTION ( 'NONE',  ( -1.000000000000000000, -0.000000000000000000, 0.000000000000000000 ) ) ;
#23924 = ADVANCED_FACE ( 'NONE', ( #21333 ), #21088, .T. ) ;
#23925 = ORIENTED_EDGE ( 'NONE', *, *, #17385, .T. ) ;
#23926 = CIRCLE ( 'NONE', #38791, 31.99999999999999289 ) ;
#23927 = VERTEX_POINT ( 'NONE', #32132 ) ;
#23928 = CIRCLE ( 'NONE', #36431, 32.00000000000000711 ) ;
#23929 = EDGE_CURVE ( 'NONE', #45282, #23124, #44184, .T. ) ;
#23930 = DIRECTION ( 'NONE',  ( -1.000000000000000000, -0.000000000000000000, 0.000000000000000000 ) ) ;
#23932 = ORIENTED_EDGE ( 'NONE', *, *, #31584, .T. ) ;
#23931 = LINE ( 'NONE', #27598, #32134 ) ;
#23933 = LINE ( 'NONE', #12675, #42326 ) ;
#23934 = ORIENTED_EDGE ( 'NONE', *, *, #21935, .F. ) ;
#23935 = ORIENTED_EDGE ( 'NONE', *, *, #13150, .T. ) ;
#23936 = CIRCLE ( 'NONE', #35642, 82.00000000000000000 ) ;
#23937 = FACE_OUTER_BOUND ( 'NONE', #198, .T. ) ;
#23938 = EDGE_CURVE ( 'NONE', #47062, #40883, #30921, .T. ) ;
#23939 = VERTEX_POINT ( 'NONE', #28446 ) ;
#23940 = ORIENTED_EDGE ( 'NONE', *, *, #8820, .F. ) ;
#23941 = DIRECTION ( 'NONE',  ( 0.000000000000000000, 0.000000000000000000, 1.000000000000000000 ) ) ;
#23942 = DIRECTION ( 'NONE',  ( -1.000000000000000000, 0.000000000000000000, 0.000000000000000000 ) ) ;
#23943 = ORIENTED_EDGE ( 'NONE', *, *, #3796, .F. ) ;
#23944 = AXIS2_PLACEMENT_3D ( 'NONE', #40221, #47772, #14019 ) ;
#23945 = DIRECTION ( 'NONE',  ( -1.000000000000000000, 0.000000000000000000, 0.000000000000000000 ) ) ;
#23946 = CARTESIAN_POINT ( 'NONE',  ( 10.00000000000000000, -8.966570791701267140, 81.50828551894223040 ) ) ;
#23947 = DIRECTION ( 'NONE',  ( -1.000000000000000000, 0.000000000000000000, 0.000000000000000000 ) ) ;
#23948 = AXIS2_PLACEMENT_3D ( 'NONE', #32365, #21330, #24778 ) ;
#23949 = ORIENTED_EDGE ( 'NONE', *, *, #14592, .T. ) ;
#23950 = ORIENTED_EDGE ( 'NONE', *, *, #21722, .F. ) ;
#23951 = EDGE_CURVE ( 'NONE', #20800, #37732, #19967, .T. ) ;
#23952 = DIRECTION ( 'NONE',  ( -1.000000000000000000, -0.000000000000000000, -0.000000000000000000 ) ) ;
#23953 = AXIS2_PLACEMENT_3D ( 'NONE', #43809, #28655, #25927 ) ;
#23954 = LINE ( 'NONE', #38889, #18833 ) ;
#23955 = EDGE_LOOP ( 'NONE', ( #3452, #30646, #40973, #36804 ) ) ;
#23956 = EDGE_CURVE ( 'NONE', #45280, #44883, #34006, .T. ) ;
#23957 = LINE ( 'NONE', #31549, #11117 ) ;
#23958 = ORIENTED_EDGE ( 'NONE', *, *, #15324, .F. ) ;
#23959 = DIRECTION ( 'NONE',  ( 0.000000000000000000, 0.3090169943749410120, 0.9510565162951556406 ) ) ;
#23960 = LINE ( 'NONE', #34960, #9113 ) ;
#23961 = DIRECTION ( 'NONE',  ( 1.000000000000000000, 0.000000000000000000, 0.000000000000000000 ) ) ;
#23962 = VERTEX_POINT ( 'NONE', #17879 ) ;
#23963 = LINE ( 'NONE', #16604, #31519 ) ;
#23964 = CARTESIAN_POINT ( 'NONE',  ( -3.000000000000000000, 8.688484142254221609, -21.88630264137359660 ) ) ;
#23965 = CARTESIAN_POINT ( 'NONE',  ( 11.99999999999999822, 60.67117009219136037, 55.16347631943064300 ) ) ;
#23966 = EDGE_CURVE ( 'NONE', #44892, #9789, #40714, .T. ) ;
#23967 = CIRCLE ( 'NONE', #17698, 16.00000000000000711 ) ;
#23968 = DIRECTION ( 'NONE',  ( -1.000000000000000000, 0.000000000000000000, 0.000000000000000000 ) ) ;
#23969 = DIRECTION ( 'NONE',  ( -0.9580045777625452175, -0.2867529058022035837, 0.000000000000000000 ) ) ;
#23970 = EDGE_LOOP ( 'NONE', ( #9996, #29040, #7415, #46588 ) ) ;
#23971 = CYLINDRICAL_SURFACE ( 'NONE', #8873, 37.49900000000000233 ) ;
#23972 = ORIENTED_EDGE ( 'NONE', *, *, #4440, .F. ) ;
#23973 = ORIENTED_EDGE ( 'NONE', *, *, #3408, .T. ) ;
#23974 = EDGE_CURVE ( 'NONE', #46639, #42124, #23076, .T. ) ;
#23975 = AXIS2_PLACEMENT_3D ( 'NONE', #38398, #48089, #18472 ) ;
#23976 = CARTESIAN_POINT ( 'NONE',  ( 10.00000000000000000, -28.89263327155797967, 71.91182617369179297 ) ) ;
#23977 = ORIENTED_EDGE ( 'NONE', *, *, #28618, .T. ) ;
#23978 = ORIENTED_EDGE ( 'NONE', *, *, #45829, .T. ) ;
#23979 = FACE_OUTER_BOUND ( 'NONE', #39165, .T. ) ;
#23980 = AXIS2_PLACEMENT_3D ( 'NONE', #883, #30762, #22924 ) ;
#23981 = FACE_OUTER_BOUND ( 'NONE', #10021, .T. ) ;
#23982 = VERTEX_POINT ( 'NONE', #37042 ) ;
#23983 = AXIS2_PLACEMENT_3D ( 'NONE', #26127, #4351, #44974 ) ;
#23984 = EDGE_CURVE ( 'NONE', #27526, #5723, #44990, .T. ) ;
#23985 = CARTESIAN_POINT ( 'NONE',  ( 5.000000000000000000, 32.34446384429971744, 26.79245525562726016 ) ) ;
#23986 = EDGE_CURVE ( 'NONE', #35412, #37888, #37158, .T. ) ;
#23987 = ORIENTED_EDGE ( 'NONE', *, *, #11813, .T. ) ;
#23988 = ORIENTED_EDGE ( 'NONE', *, *, #34639, .F. ) ;
#23989 = EDGE_LOOP ( 'NONE', ( #23091, #44540 ) ) ;
#23990 = EDGE_CURVE ( 'NONE', #9753, #46024, #25054, .T. ) ;
#23991 = CIRCLE ( 'NONE', #47435, 77.49899999999999523 ) ;
#23992 = DIRECTION ( 'NONE',  ( 0.000000000000000000, -0.7071067811865536790, 0.7071067811865414665 ) ) ;
#23993 = ORIENTED_EDGE ( 'NONE', *, *, #46065, .T. ) ;
#23994 = CARTESIAN_POINT ( 'NONE',  ( 0.000000000000000000, -81.90746397400391743, 3.894527615417586741 ) ) ;
#23995 = EDGE_CURVE ( 'NONE', #19224, #15249, #10862, .T. ) ;
#23996 = ORIENTED_EDGE ( 'NONE', *, *, #7478, .F. ) ;
#23997 = CYLINDRICAL_SURFACE ( 'NONE', #14174, 31.99999999999999289 ) ;
#23998 = AXIS2_PLACEMENT_3D ( 'NONE', #11502, #40152, #6611 ) ;
#23999 = CARTESIAN_POINT ( 'NONE',  ( 11.99999999999999822, 51.03279382321088065, 55.19960302592086521 ) ) ;
#24000 = CYLINDRICAL_SURFACE ( 'NONE', #8000, 31.99999999999999289 ) ;
#24001 = ORIENTED_EDGE ( 'NONE', *, *, #34034, .T. ) ;
#24002 = CARTESIAN_POINT ( 'NONE',  ( 15.00000000000000000, -22.67460108101782978, -6.353146135317906840 ) ) ;
#24003 = ORIENTED_EDGE ( 'NONE', *, *, #436, .F. ) ;
#24004 = CARTESIAN_POINT ( 'NONE',  ( 0.000000000000000000, 0.000000000000000000, 0.000000000000000000 ) ) ;
#24005 = CARTESIAN_POINT ( 'NONE',  ( 10.00000000000000000, 71.91182617369189245, 28.89263327155772743 ) ) ;
#24006 = ORIENTED_EDGE ( 'NONE', *, *, #38081, .T. ) ;
#24007 = AXIS2_PLACEMENT_3D ( 'NONE', #4030, #33874, #4515 ) ;
#24008 = DIRECTION ( 'NONE',  ( 0.000000000000000000, -0.8910065241883722287, 0.4539904997395383668 ) ) ;
#24009 = ORIENTED_EDGE ( 'NONE', *, *, #26943, .F. ) ;
#24010 = ORIENTED_EDGE ( 'NONE', *, *, #17382, .F. ) ;
#24011 = LINE ( 'NONE', #31855, #8025 ) ;
#24012 = DIRECTION ( 'NONE',  ( -1.000000000000000000, 0.000000000000000000, -0.000000000000000000 ) ) ;
#24013 = CARTESIAN_POINT ( 'NONE',  ( 10.00000000000000000, 79.10210256391367523, 21.60688246758613218 ) ) ;
#24014 = DIRECTION ( 'NONE',  ( -1.000000000000000000, 0.000000000000000000, 0.000000000000000000 ) ) ;
#24015 = CARTESIAN_POINT ( 'NONE',  ( -10.00000000000000000, 0.000000000000000000, 0.000000000000000000 ) ) ;
#24016 = CIRCLE ( 'NONE', #5256, 37.49900000000000944 ) ;
#24017 = DIRECTION ( 'NONE',  ( -1.000000000000000000, 0.000000000000000000, -0.000000000000000000 ) ) ;
#24018 = DIRECTION ( 'NONE',  ( 0.000000000000000000, 0.000000000000000000, 1.000000000000000000 ) ) ;
#24019 = AXIS2_PLACEMENT_3D ( 'NONE', #3055, #25570, #40516 ) ;
#24020 = CARTESIAN_POINT ( 'NONE',  ( 0.000000000000000000, 0.000000000000000000, 0.000000000000000000 ) ) ;
#24021 = EDGE_CURVE ( 'NONE', #19470, #45584, #435, .T. ) ;
#24022 = EDGE_LOOP ( 'NONE', ( #15082, #45781, #40357, #10443 ) ) ;
#24023 = CARTESIAN_POINT ( 'NONE',  ( 32.50000000000000000, -120.0000000000000000, 2.500000000000000000 ) ) ;
#24024 = CARTESIAN_POINT ( 'NONE',  ( 0.000000000000000000, 16.65972982744933972, 80.28980883073764119 ) ) ;
#24025 = FACE_OUTER_BOUND ( 'NONE', #19229, .T. ) ;
#24026 = ORIENTED_EDGE ( 'NONE', *, *, #7822, .T. ) ;
#24027 = DIRECTION ( 'NONE',  ( 0.000000000000000000, -0.7071067811865389130, -0.7071067811865561215 ) ) ;
#24028 = DIRECTION ( 'NONE',  ( 0.000000000000000000, 0.000000000000000000, -1.000000000000000000 ) ) ;
#24029 =( NAMED_UNIT ( * ) PLANE_ANGLE_UNIT ( ) SI_UNIT ( $, .RADIAN. ) );
#24030 = EDGE_CURVE ( 'NONE', #22304, #10568, #13727, .T. ) ;
#24031 = DIRECTION ( 'NONE',  ( 0.000000000000000000, 0.000000000000000000, 1.000000000000000000 ) ) ;
#24032 = ORIENTED_EDGE ( 'NONE', *, *, #30515, .F. ) ;
#24033 = AXIS2_PLACEMENT_3D ( 'NONE', #29489, #10402, #40277 ) ;
#24034 = EDGE_LOOP ( 'NONE', ( #43199, #18491, #39646, #12295 ) ) ;
#24035 = AXIS2_PLACEMENT_3D ( 'NONE', #33141, #14057, #29704 ) ;
#24036 = DIRECTION ( 'NONE',  ( 0.000000000000000000, -1.000000000000000000, 0.000000000000000000 ) ) ;
#24037 = DIRECTION ( 'NONE',  ( -1.000000000000000000, 0.000000000000000000, -0.000000000000000000 ) ) ;
#24038 = AXIS2_PLACEMENT_3D ( 'NONE', #34653, #12408, #19477 ) ;
#24039 = DIRECTION ( 'NONE',  ( 0.000000000000000000, -0.6494480483301903195, 0.7604059656000251577 ) ) ;
#24040 = ORIENTED_EDGE ( 'NONE', *, *, #2877, .T. ) ;
#24041 = CIRCLE ( 'NONE', #7608, 31.99999999999998579 ) ;
#24042 = EDGE_CURVE ( 'NONE', #32098, #6289, #23891, .T. ) ;
#24043 = LINE ( 'NONE', #27964, #2317 ) ;
#24044 = VERTEX_POINT ( 'NONE', #3260 ) ;
#24045 = CARTESIAN_POINT ( 'NONE',  ( 5.000000000000002665, -68.55367621811173251, 44.99326035066031437 ) ) ;
#24046 = ORIENTED_EDGE ( 'NONE', *, *, #46924, .T. ) ;
#24048 = EDGE_CURVE ( 'NONE', #6120, #23445, #14542, .T. ) ;
#24047 = FACE_OUTER_BOUND ( 'NONE', #47797, .T. ) ;
#24049 = AXIS2_PLACEMENT_3D ( 'NONE', #13961, #7091, #14693 ) ;
#24050 = DIRECTION ( 'NONE',  ( 0.000000000000000000, 0.000000000000000000, 1.000000000000000000 ) ) ;
#24051 = EDGE_CURVE ( 'NONE', #5642, #10514, #9039, .T. ) ;
#24052 = CARTESIAN_POINT ( 'NONE',  ( 10.00000000000000000, -11.30684508768284680, -76.66974797899850103 ) ) ;
#24053 = ORIENTED_EDGE ( 'NONE', *, *, #42458, .T. ) ;
#24055 = ORIENTED_EDGE ( 'NONE', *, *, #6152, .T. ) ;
#24054 = DIRECTION ( 'NONE',  ( -1.000000000000000000, 0.000000000000000000, -0.000000000000000000 ) ) ;
#24056 = EDGE_LOOP ( 'NONE', ( #6997, #38606, #33960, #48256 ) ) ;
#24057 = ADVANCED_FACE ( 'NONE', ( #3022 ), #3510, .T. ) ;
#24058 = ORIENTED_EDGE ( 'NONE', *, *, #14087, .T. ) ;
#24059 = CARTESIAN_POINT ( 'NONE',  ( 11.99999999999999822, -8.840884882375609877, 74.65374052328647281 ) ) ;
#24060 = CARTESIAN_POINT ( 'NONE',  ( 0.000000000000000000, -14.67089635893658794, -73.72996012237454977 ) ) ;
#24061 = CARTESIAN_POINT ( 'NONE',  ( -23.30023580412278861, -123.4057321492263384, -2.500000000000000000 ) ) ;
#24062 = CARTESIAN_POINT ( 'NONE',  ( 11.99999999999999822, 0.000000000000000000, 0.000000000000000000 ) ) ;
#24064 = DIRECTION ( 'NONE',  ( -1.000000000000000000, 0.000000000000000000, 0.000000000000000000 ) ) ;
#24063 = CIRCLE ( 'NONE', #42029, 82.00000000000000000 ) ;
#24065 = ORIENTED_EDGE ( 'NONE', *, *, #19002, .F. ) ;
#24066 = FACE_OUTER_BOUND ( 'NONE', #36111, .T. ) ;
#24067 = VERTEX_POINT ( 'NONE', #6464 ) ;
#24068 = DIRECTION ( 'NONE',  ( -1.000000000000000000, -0.000000000000000000, 0.000000000000000000 ) ) ;
#24069 = VERTEX_POINT ( 'NONE', #36324 ) ;
#24071 = CIRCLE ( 'NONE', #45169, 42.00000000000000000 ) ;
#24070 = CARTESIAN_POINT ( 'NONE',  ( 10.00000000000000000, 6.903761155837774943, 77.19088730480525840 ) ) ;
#24072 = CARTESIAN_POINT ( 'NONE',  ( 11.99999999999999822, 0.000000000000000000, 0.000000000000000000 ) ) ;
#24073 = DIRECTION ( 'NONE',  ( -1.000000000000000000, 0.000000000000000000, 0.000000000000000000 ) ) ;
#24074 = ORIENTED_EDGE ( 'NONE', *, *, #27496, .F. ) ;
#24075 = CARTESIAN_POINT ( 'NONE',  ( 0.000000000000000000, -6.736453364083290651, -36.88895765772640090 ) ) ;
#24076 = CARTESIAN_POINT ( 'NONE',  ( 10.00000000000000000, -35.92658777277517856, 10.74501242461269257 ) ) ;
#24077 = CARTESIAN_POINT ( 'NONE',  ( 0.000000000000000000, 0.000000000000000000, 0.000000000000000000 ) ) ;
#24078 = DIRECTION ( 'NONE',  ( -0.000000000000000000, -0.000000000000000000, -1.000000000000000000 ) ) ;
#24079 = CARTESIAN_POINT ( 'NONE',  ( 0.000000000000000000, -16.65560815589439159, 38.55633173627004595 ) ) ;
#24080 = CARTESIAN_POINT ( 'NONE',  ( 11.99999999999999822, -73.73191006444582740, 14.66109333815435889 ) ) ;
#24081 = DIRECTION ( 'NONE',  ( 1.000000000000000000, 0.000000000000000000, 0.000000000000000000 ) ) ;
#24082 = CARTESIAN_POINT ( 'NONE',  ( 10.00000000000000000, 25.88420570971400991, 27.13269053701105449 ) ) ;
#24083 = CARTESIAN_POINT ( 'NONE',  ( 10.00000000000000000, -68.27212725128298132, 31.46837873494953541 ) ) ;
#24084 = DIRECTION ( 'NONE',  ( -1.000000000000000000, 0.000000000000000000, 0.000000000000000000 ) ) ;
#24085 = ORIENTED_EDGE ( 'NONE', *, *, #11552, .T. ) ;
#24086 = AXIS2_PLACEMENT_3D ( 'NONE', #32714, #11177, #41049 ) ;
#24087 = CARTESIAN_POINT ( 'NONE',  ( 5.000000000000002665, 22.90783923731629912, 78.73519480814962890 ) ) ;
#24088 = VERTEX_POINT ( 'NONE', #10372 ) ;
#24089 = CARTESIAN_POINT ( 'NONE',  ( 0.000000000000000000, 6.762365576493645669, -25.66652317338392209 ) ) ;
#24090 = EDGE_CURVE ( 'NONE', #31305, #12188, #10629, .T. ) ;
#24091 = LINE ( 'NONE', #20398, #27593 ) ;
#24092 = ORIENTED_EDGE ( 'NONE', *, *, #29985, .T. ) ;
#24093 = CIRCLE ( 'NONE', #35789, 31.99999999999998934 ) ;
#24094 = DIRECTION ( 'NONE',  ( 0.000000000000000000, 0.000000000000000000, 1.000000000000000000 ) ) ;
#24095 = MECHANICAL_DESIGN_GEOMETRIC_PRESENTATION_REPRESENTATION (  '', ( #17063 ), #17822 ) ;
#24096 = ORIENTED_EDGE ( 'NONE', *, *, #24919, .F. ) ;
#24097 = ADVANCED_FACE ( 'NONE', ( #44630 ), #21638, .T. ) ;
#24098 = VECTOR ( 'NONE', #24397, 1000.000000000000114 ) ;
#24099 = VERTEX_POINT ( 'NONE', #17718 ) ;
#24100 = ADVANCED_FACE ( 'NONE', ( #21862 ), #7436, .T. ) ;
#24101 = EDGE_CURVE ( 'NONE', #37099, #9873, #32423, .T. ) ;
#24102 = CARTESIAN_POINT ( 'NONE',  ( 4.999999999999999112, -10.41901085202107247, 40.68715046381925049 ) ) ;
#24103 = EDGE_CURVE ( 'NONE', #27674, #29067, #14489, .T. ) ;
#24104 = CARTESIAN_POINT ( 'NONE',  ( 0.000000000000000000, -12.26510123303284594, 35.53030884539080603 ) ) ;
#24106 = EDGE_LOOP ( 'NONE', ( #14520, #25463, #20726, #3009 ) ) ;
#24105 = DIRECTION ( 'NONE',  ( -1.000000000000000000, 0.000000000000000000, 0.000000000000000000 ) ) ;
#24107 = EDGE_LOOP ( 'NONE', ( #41432, #29450, #28949, #25217 ) ) ;
#24108 = CARTESIAN_POINT ( 'NONE',  ( 0.000000000000000000, 0.000000000000000000, 0.000000000000000000 ) ) ;
#24109 = EDGE_CURVE ( 'NONE', #46672, #6962, #20743, .T. ) ;
#24110 = AXIS2_PLACEMENT_3D ( 'NONE', #30183, #3240, #15254 ) ;
#24111 = ORIENTED_EDGE ( 'NONE', *, *, #30300, .F. ) ;
#24112 = DIRECTION ( 'NONE',  ( -1.000000000000000000, 0.000000000000000000, -0.000000000000000000 ) ) ;
#24113 = CYLINDRICAL_SURFACE ( 'NONE', #34832, 82.00000000000000000 ) ;
#24114 = LINE ( 'NONE', #35113, #39184 ) ;
#24115 = VECTOR ( 'NONE', #42383, 999.9999999999998863 ) ;
#24116 = ORIENTED_EDGE ( 'NONE', *, *, #8773, .F. ) ;
#24117 = ORIENTED_EDGE ( 'NONE', *, *, #8373, .T. ) ;
#24118 = CARTESIAN_POINT ( 'NONE',  ( 10.00000000000000000, -0.6853352020793173072, 37.58145647212453611 ) ) ;
#24119 = ORIENTED_EDGE ( 'NONE', *, *, #35922, .T. ) ;
#24120 = CARTESIAN_POINT ( 'NONE',  ( 10.00000000000000000, -66.50666863321973210, -39.78640506895676765 ) ) ;
#24121 = ADVANCED_FACE ( 'NONE', ( #5387 ), #31591, .T. ) ;
#24122 = CARTESIAN_POINT ( 'NONE',  ( 0.000000000000000000, 27.05870788708231700, 26.08949754953034272 ) ) ;
#24123 = DIRECTION ( 'NONE',  ( 0.000000000000000000, 0.000000000000000000, 1.000000000000000000 ) ) ;
#24124 = DIRECTION ( 'NONE',  ( -1.000000000000000000, 0.000000000000000000, -0.000000000000000000 ) ) ;
#24125 = DIRECTION ( 'NONE',  ( 0.000000000000000000, -0.9945218953682742891, -0.1045284632676436315 ) ) ;
#24126 = DIRECTION ( 'NONE',  ( 0.000000000000000000, -6.938893903907228378E-15, 1.000000000000000000 ) ) ;
#24127 = DIRECTION ( 'NONE',  ( 0.9997280174009349762, -0.02332147558787671729, 0.000000000000000000 ) ) ;
#24128 = ORIENTED_EDGE ( 'NONE', *, *, #40242, .T. ) ;
#24129 = CARTESIAN_POINT ( 'NONE',  ( 11.99999999999999822, -81.96053171279901051, -2.543863470249249747 ) ) ;
#24130 = CARTESIAN_POINT ( 'NONE',  ( 11.99999999999999822, 49.70050353004889132, 59.46389618801982380 ) ) ;
#24131 = DIRECTION ( 'NONE',  ( -1.000000000000000000, 0.000000000000000000, -0.000000000000000000 ) ) ;
#24132 = DIRECTION ( 'NONE',  ( 0.4796670183876317051, -0.8774505977381971134, 0.000000000000000000 ) ) ;
#24133 = VERTEX_POINT ( 'NONE', #1476 ) ;
#24134 = AXIS2_PLACEMENT_3D ( 'NONE', #28123, #12970, #9758 ) ;
#24135 = CARTESIAN_POINT ( 'NONE',  ( 10.00000000000000000, 0.000000000000000000, 0.000000000000000000 ) ) ;
#24136 = DIRECTION ( 'NONE',  ( -1.000000000000000000, -0.000000000000000000, -0.000000000000000000 ) ) ;
#24137 = AXIS2_PLACEMENT_3D ( 'NONE', #30991, #42222, #9178 ) ;
#24138 = CARTESIAN_POINT ( 'NONE',  ( 0.000000000000000000, -0.8261519478425669583, -77.49459641780886443 ) ) ;
#24139 = DIRECTION ( 'NONE',  ( 0.000000000000000000, 0.9510565162951523099, 0.3090169943749513926 ) ) ;
#24140 = EDGE_CURVE ( 'NONE', #25302, #7292, #26947, .T. ) ;
#24141 = CARTESIAN_POINT ( 'NONE',  ( -10.00000000000000000, 0.000000000000000000, 0.000000000000000000 ) ) ;
#24142 = DIRECTION ( 'NONE',  ( 0.000000000000000000, 0.4067366430757887730, 0.9135454576426059736 ) ) ;
#24143 = VERTEX_POINT ( 'NONE', #27663 ) ;
#24144 = DIRECTION ( 'NONE',  ( -1.000000000000000000, -0.000000000000000000, -0.000000000000000000 ) ) ;
#24145 = EDGE_CURVE ( 'NONE', #20591, #25493, #34849, .T. ) ;
#24146 = ORIENTED_EDGE ( 'NONE', *, *, #5265, .T. ) ;
#24147 = FILL_AREA_STYLE ('',( #5313 ) ) ;
#24148 = EDGE_CURVE ( 'NONE', #35892, #10741, #27183, .T. ) ;
#24149 = CARTESIAN_POINT ( 'NONE',  ( 10.00000000000000000, -65.59268652807237743, 36.72794159290217664 ) ) ;
#24150 = ORIENTED_EDGE ( 'NONE', *, *, #31810, .F. ) ;
#24151 = ORIENTED_EDGE ( 'NONE', *, *, #36433, .T. ) ;
#24152 = VERTEX_POINT ( 'NONE', #5157 ) ;
#24153 = DIRECTION ( 'NONE',  ( -1.000000000000000000, 0.000000000000000000, 0.000000000000000000 ) ) ;
#24154 = ORIENTED_EDGE ( 'NONE', *, *, #40417, .F. ) ;
#24155 = EDGE_CURVE ( 'NONE', #14947, #41627, #38929, .T. ) ;
#24156 = ADVANCED_FACE ( 'NONE', ( #20069 ), #12731, .T. ) ;
#24157 = ORIENTED_EDGE ( 'NONE', *, *, #4960, .F. ) ;
#24158 = CIRCLE ( 'NONE', #16332, 37.49900000000000944 ) ;
#24159 = CYLINDRICAL_SURFACE ( 'NONE', #26542, 31.99999999999998579 ) ;
#24160 = CARTESIAN_POINT ( 'NONE',  ( 12.00000000000000000, -13.04903810567646971, 19.60159698893442481 ) ) ;
#24161 = AXIS2_PLACEMENT_3D ( 'NONE', #34426, #7544, #44985 ) ;
#24162 = ORIENTED_EDGE ( 'NONE', *, *, #14706, .F. ) ;
#24163 = EDGE_LOOP ( 'NONE', ( #12224, #41067, #17608, #31647 ) ) ;
#24164 = CIRCLE ( 'NONE', #5408, 77.49899999999999523 ) ;
#24165 = ORIENTED_EDGE ( 'NONE', *, *, #32539, .T. ) ;
#24166 = CARTESIAN_POINT ( 'NONE',  ( -23.54415474984308787, -120.4156646670583086, 5.500000000000000000 ) ) ;
#24167 = ADVANCED_FACE ( 'NONE', ( #31104 ), #970, .T. ) ;
#24169 = VERTEX_POINT ( 'NONE', #8330 ) ;
#24168 = CYLINDRICAL_SURFACE ( 'NONE', #29778, 31.99999999999998579 ) ;
#24170 = DIRECTION ( 'NONE',  ( 0.000000000000000000, -0.1045284632676437703, 0.9945218953682742891 ) ) ;
#24171 = ORIENTED_EDGE ( 'NONE', *, *, #40821, .F. ) ;
#24172 = CARTESIAN_POINT ( 'NONE',  ( 0.000000000000000000, -20.40083707022935400, 72.35432306680478121 ) ) ;
#24173 = EDGE_LOOP ( 'NONE', ( #34701, #27401, #8686, #19994 ) ) ;
#24174 = ORIENTED_EDGE ( 'NONE', *, *, #42573, .F. ) ;
#24175 = LINE ( 'NONE', #16838, #22023 ) ;
#24176 = CARTESIAN_POINT ( 'NONE',  ( 10.00000000000000000, -65.58780272294048075, -36.73666225445966660 ) ) ;
#24177 = EDGE_LOOP ( 'NONE', ( #29229, #38773, #20606, #47451 ) ) ;
#24178 = CARTESIAN_POINT ( 'NONE',  ( 10.00000000000000000, 37.58145647212455032, -0.6853352020786441789 ) ) ;
#24179 = CYLINDRICAL_SURFACE ( 'NONE', #46373, 16.00000000000000000 ) ;
#24180 = DIRECTION ( 'NONE',  ( -1.000000000000000000, 0.000000000000000000, -0.000000000000000000 ) ) ;
#24181 = ORIENTED_EDGE ( 'NONE', *, *, #12178, .F. ) ;
#24182 = VERTEX_POINT ( 'NONE', #19338 ) ;
#24183 = DIRECTION ( 'NONE',  ( -1.000000000000000000, -0.000000000000000000, 0.000000000000000000 ) ) ;
#24184 = CYLINDRICAL_SURFACE ( 'NONE', #29810, 77.49899999999999523 ) ;
#24185 = ORIENTED_EDGE ( 'NONE', *, *, #8622, .T. ) ;
#24186 = DIRECTION ( 'NONE',  ( -1.000000000000000000, 0.000000000000000000, -0.000000000000000000 ) ) ;
#24187 = ORIENTED_EDGE ( 'NONE', *, *, #34655, .F. ) ;
#24188 = DIRECTION ( 'NONE',  ( -1.000000000000000000, 0.000000000000000000, 0.000000000000000000 ) ) ;
#24189 = CARTESIAN_POINT ( 'NONE',  ( 11.99999999999999822, -39.47590169984795239, -71.87247863392457248 ) ) ;
#24190 = DIRECTION ( 'NONE',  ( -1.000000000000000000, 0.000000000000000000, 0.000000000000000000 ) ) ;
#24191 = DIRECTION ( 'NONE',  ( -1.000000000000000000, -0.000000000000000000, -0.000000000000000000 ) ) ;
#24192 = CARTESIAN_POINT ( 'NONE',  ( 0.000000000000000000, 41.91543099594818500, 2.663952781846294915 ) ) ;
#24193 = AXIS2_PLACEMENT_3D ( 'NONE', #10329, #44831, #43869 ) ;
#24194 = VERTEX_POINT ( 'NONE', #34498 ) ;
#24195 = EDGE_CURVE ( 'NONE', #30860, #14490, #23737, .T. ) ;
#24196 = CARTESIAN_POINT ( 'NONE',  ( 0.000000000000000000, -75.16055320797043748, 18.89407956138231270 ) ) ;
#24197 = LINE ( 'NONE', #39133, #30040 ) ;
#24198 = VECTOR ( 'NONE', #1156, 1000.000000000000000 ) ;
#24199 = DIRECTION ( 'NONE',  ( 0.000000000000000000, 0.000000000000000000, 1.000000000000000000 ) ) ;
#24200 = VERTEX_POINT ( 'NONE', #23994 ) ;
#24201 = EDGE_CURVE ( 'NONE', #40188, #21764, #38693, .T. ) ;
#24202 = CARTESIAN_POINT ( 'NONE',  ( 6.000000000000000000, -74.18225833017913828, 34.94270380257611208 ) ) ;
#24203 = EDGE_CURVE ( 'NONE', #9886, #30256, #35235, .T. ) ;
#24204 = EDGE_LOOP ( 'NONE', ( #7007, #27932, #12222, #35403 ) ) ;
#24205 = ORIENTED_EDGE ( 'NONE', *, *, #31805, .T. ) ;
#24206 = AXIS2_PLACEMENT_3D ( 'NONE', #45127, #26523, #575 ) ;
#24207 = CARTESIAN_POINT ( 'NONE',  ( 0.000000000000000000, 14.66109333815564852, -73.73191006444555740 ) ) ;
#24208 = DIRECTION ( 'NONE',  ( -0.3853207896976523772, 0.9227826878668550226, 0.000000000000000000 ) ) ;
#24209 = VERTEX_POINT ( 'NONE', #1715 ) ;
#24210 = EDGE_CURVE ( 'NONE', #16571, #13285, #30603, .T. ) ;
#24211 = EDGE_CURVE ( 'NONE', #8489, #3193, #16640, .T. ) ;
#24212 = EDGE_CURVE ( 'NONE', #5067, #33061, #45522, .T. ) ;
#24213 = DIRECTION ( 'NONE',  ( 0.000000000000000000, 0.000000000000000000, 1.000000000000000000 ) ) ;
#24214 = ORIENTED_EDGE ( 'NONE', *, *, #35759, .T. ) ;
#24215 = ORIENTED_EDGE ( 'NONE', *, *, #8681, .F. ) ;
#24216 = VERTEX_POINT ( 'NONE', #38195 ) ;
#24217 = EDGE_CURVE ( 'NONE', #38437, #30519, #4657, .T. ) ;
#24218 = AXIS2_PLACEMENT_3D ( 'NONE', #2929, #48206, #36696 ) ;
#24219 = CARTESIAN_POINT ( 'NONE',  ( 11.99999999999999822, 75.11764819372149304, 29.05362095685338275 ) ) ;
#24221 = VERTEX_POINT ( 'NONE', #30861 ) ;
#24220 = CIRCLE ( 'NONE', #34370, 31.99999999999998579 ) ;
#24222 = DIRECTION ( 'NONE',  ( 0.000000000000000000, 0.8910065241883688980, -0.4539904997395445840 ) ) ;
#24223 = ORIENTED_EDGE ( 'NONE', *, *, #43280, .T. ) ;
#24224 = DIRECTION ( 'NONE',  ( 0.000000000000000000, -0.9969173337331271867, -0.07845909572785571273 ) ) ;
#24225 = CIRCLE ( 'NONE', #10955, 77.49900000000000944 ) ;
#24226 = DIRECTION ( 'NONE',  ( 0.000000000000000000, 0.000000000000000000, 1.000000000000000000 ) ) ;
#24227 = CARTESIAN_POINT ( 'NONE',  ( -10.00000000000000000, 0.000000000000000000, 0.000000000000000000 ) ) ;
#24228 = VERTEX_POINT ( 'NONE', #45790 ) ;
#24229 = COLOUR_RGB ( '', 0.09019608, 0.27058824, 0.51372549) ;
#24230 = DIRECTION ( 'NONE',  ( 0.6575728627325957421, -0.7533909544171994987, 0.000000000000000000 ) ) ;
#24231 = VERTEX_POINT ( 'NONE', #12260 ) ;
#24232 = CARTESIAN_POINT ( 'NONE',  ( 10.00000000000000000, 0.000000000000000000, 0.000000000000000000 ) ) ;
#24233 = CARTESIAN_POINT ( 'NONE',  ( 0.000000000000000000, 41.91543099594818500, 2.663952781846294915 ) ) ;
#24234 = DIRECTION ( 'NONE',  ( 0.000000000000000000, 0.000000000000000000, -1.000000000000000000 ) ) ;
#24235 = ORIENTED_EDGE ( 'NONE', *, *, #6163, .F. ) ;
#24236 = VECTOR ( 'NONE', #27738, 1000.000000000000000 ) ;
#24237 = EDGE_LOOP ( 'NONE', ( #34254, #10607, #28152, #20334 ) ) ;
#24238 = FACE_OUTER_BOUND ( 'NONE', #48254, .T. ) ;
#24239 = DIRECTION ( 'NONE',  ( 0.000000000000000000, 0.000000000000000000, 1.000000000000000000 ) ) ;
#24240 = ORIENTED_EDGE ( 'NONE', *, *, #46493, .F. ) ;
#24241 = FACE_OUTER_BOUND ( 'NONE', #43549, .T. ) ;
#24242 = FACE_OUTER_BOUND ( 'NONE', #3057, .T. ) ;
#24243 = DIRECTION ( 'NONE',  ( 0.000000000000000000, 0.000000000000000000, 1.000000000000000000 ) ) ;
#24244 = CARTESIAN_POINT ( 'NONE',  ( 10.00000000000000000, 35.53030884539102630, -12.26510123303222599 ) ) ;
#24245 = CARTESIAN_POINT ( 'NONE',  ( 0.000000000000000000, 71.27951684758026829, 30.41916302227139113 ) ) ;
#24246 = FACE_OUTER_BOUND ( 'NONE', #43010, .T. ) ;
#24247 = CYLINDRICAL_SURFACE ( 'NONE', #9820, 77.49899999999999523 ) ;
#24248 = LINE ( 'NONE', #8830, #44373 ) ;
#24249 = DIRECTION ( 'NONE',  ( -1.000000000000000000, -0.000000000000000000, 0.000000000000000000 ) ) ;
#24250 = EDGE_CURVE ( 'NONE', #22099, #27232, #42107, .T. ) ;
#24251 = DIRECTION ( 'NONE',  ( -1.000000000000000000, 0.000000000000000000, -0.000000000000000000 ) ) ;
#24252 = FACE_OUTER_BOUND ( 'NONE', #3003, .T. ) ;
#24253 = LINE ( 'NONE', #9554, #36595 ) ;
#24254 = EDGE_CURVE ( 'NONE', #46727, #34724, #19995, .T. ) ;
#24255 = CARTESIAN_POINT ( 'NONE',  ( -10.00000000000000000, 0.000000000000000000, 0.000000000000000000 ) ) ;
#24256 = DIRECTION ( 'NONE',  ( 0.000000000000000000, 0.000000000000000000, 1.000000000000000000 ) ) ;
#24257 = EDGE_CURVE ( 'NONE', #1330, #11693, #5881, .T. ) ;
#24258 = ORIENTED_EDGE ( 'NONE', *, *, #48287, .F. ) ;
#24259 = EDGE_CURVE ( 'NONE', #26816, #32422, #25442, .T. ) ;
#24260 = VECTOR ( 'NONE', #32937, 1000.000000000000000 ) ;
#24261 = CARTESIAN_POINT ( 'NONE',  ( -1.200000000000000030E-05, 16.95692799528845995, 2.500000000000000000 ) ) ;
#24262 = EDGE_CURVE ( 'NONE', #45536, #2845, #12194, .T. ) ;
#24263 = CIRCLE ( 'NONE', #3131, 42.00000000000000000 ) ;
#24264 = ADVANCED_FACE ( 'NONE', ( #16886 ), #39406, .T. ) ;
#24265 = DIRECTION ( 'NONE',  ( 0.000000000000000000, 1.000000000000000000, 3.491481338843133750E-15 ) ) ;
#24266 = VECTOR ( 'NONE', #43204, 1000.000000000000000 ) ;
#24267 = AXIS2_PLACEMENT_3D ( 'NONE', #17881, #32809, #47734 ) ;
#24268 = CARTESIAN_POINT ( 'NONE',  ( 5.000000000000002665, 80.28980883073758434, 16.65972982744963460 ) ) ;
#24269 = VERTEX_POINT ( 'NONE', #31839 ) ;
#24270 = AXIS2_PLACEMENT_3D ( 'NONE', #35285, #39213, #13267 ) ;
#24271 = AXIS2_PLACEMENT_3D ( 'NONE', #18402, #7389, #11060 ) ;
#24272 = CIRCLE ( 'NONE', #3150, 37.49900000000000944 ) ;
#24273 = EDGE_CURVE ( 'NONE', #17933, #33199, #21520, .T. ) ;
#24274 = CARTESIAN_POINT ( 'NONE',  ( 19.12409105625795291, -101.5943176906707919, 5.500000000000000000 ) ) ;
#24275 = CARTESIAN_POINT ( 'NONE',  ( -3.000000000000000000, -19.89357724624987256, -12.59942793731086041 ) ) ;
#24276 = ORIENTED_EDGE ( 'NONE', *, *, #22539, .T. ) ;
#24277 = EDGE_CURVE ( 'NONE', #15551, #46699, #16105, .T. ) ;
#24278 = DIRECTION ( 'NONE',  ( -1.000000000000000000, -0.000000000000000000, 0.000000000000000000 ) ) ;
#24279 = LINE ( 'NONE', #38982, #33646 ) ;
#24280 = EDGE_LOOP ( 'NONE', ( #10620, #7610 ) ) ;
#24282 = ORIENTED_EDGE ( 'NONE', *, *, #13158, .T. ) ;
#24281 = CYLINDRICAL_SURFACE ( 'NONE', #43428, 37.49900000000000233 ) ;
#24283 = VERTEX_POINT ( 'NONE', #47224 ) ;
#24284 = FACE_OUTER_BOUND ( 'NONE', #13627, .T. ) ;
#24285 = CARTESIAN_POINT ( 'NONE',  ( 10.00000000000000000, -26.79245525562691199, -32.34446384430000876 ) ) ;
#24286 = DIRECTION ( 'NONE',  ( -1.000000000000000000, -0.000000000000000000, -0.000000000000000000 ) ) ;
#24287 = DIRECTION ( 'NONE',  ( 0.000000000000000000, 0.000000000000000000, 1.000000000000000000 ) ) ;
#24288 = AXIS2_PLACEMENT_3D ( 'NONE', #16519, #2305, #43444 ) ;
#24289 = EDGE_CURVE ( 'NONE', #28665, #3463, #24940, .T. ) ;
#24290 = CARTESIAN_POINT ( 'NONE',  ( -1.250000000000002442, -12.36245420541525242, -1.199999999999999956 ) ) ;
#24291 = ORIENTED_EDGE ( 'NONE', *, *, #37409, .F. ) ;
#24292 = AXIS2_PLACEMENT_3D ( 'NONE', #41329, #26630, #4839 ) ;
#24293 = LINE ( 'NONE', #1545, #45942 ) ;
#24294 = ORIENTED_EDGE ( 'NONE', *, *, #19142, .F. ) ;
#24295 = VERTEX_POINT ( 'NONE', #9523 ) ;
#24296 = CARTESIAN_POINT ( 'NONE',  ( 5.999999999999999112, 59.75363087400153006, -56.15606465354896670 ) ) ;
#24297 = CIRCLE ( 'NONE', #46975, 31.99999999999999289 ) ;
#24298 = CIRCLE ( 'NONE', #37614, 37.49900000000000944 ) ;
#24299 = CARTESIAN_POINT ( 'NONE',  ( -3.000000000000002665, 2.549714635824789697E-15, -20.64000000000000057 ) ) ;
#24300 = CARTESIAN_POINT ( 'NONE',  ( -10.00000000000000000, 0.000000000000000000, 0.000000000000000000 ) ) ;
#24301 = CARTESIAN_POINT ( 'NONE',  ( 0.000000000000000000, -132.5000000000000000, 40.00000000000000711 ) ) ;
#24302 = EDGE_LOOP ( 'NONE', ( #47299, #35659, #33556, #6926 ) ) ;
#24303 = DIRECTION ( 'NONE',  ( 0.000000000000000000, 0.000000000000000000, 1.000000000000000000 ) ) ;
#24304 = DIRECTION ( 'NONE',  ( -1.000000000000000000, -0.000000000000000000, 0.000000000000000000 ) ) ;
#24305 = AXIS2_PLACEMENT_3D ( 'NONE', #29888, #33789, #22786 ) ;
#24306 = DIRECTION ( 'NONE',  ( -1.000000000000000000, -0.000000000000000000, 0.000000000000000000 ) ) ;
#24307 = AXIS2_PLACEMENT_3D ( 'NONE', #43575, #6373, #44292 ) ;
#24308 = LINE ( 'NONE', #16488, #17368 ) ;
#24309 = EDGE_CURVE ( 'NONE', #38915, #22027, #12995, .T. ) ;
#24310 = CARTESIAN_POINT ( 'NONE',  ( 10.00000000000000178, 0.000000000000000000, 0.000000000000000000 ) ) ;
#24311 = CIRCLE ( 'NONE', #9453, 10.00000000000000178 ) ;
#24312 = CARTESIAN_POINT ( 'NONE',  ( 15.00000000000000000, 14.60985201121729737, 18.46759930825687235 ) ) ;
#24313 = LINE ( 'NONE', #20388, #35297 ) ;
#24314 = LINE ( 'NONE', #8898, #16185 ) ;
#24315 = EDGE_CURVE ( 'NONE', #1295, #12027, #28611, .T. ) ;
#24316 = CARTESIAN_POINT ( 'NONE',  ( 10.00000000000000000, 0.000000000000000000, 0.000000000000000000 ) ) ;
#24317 = DIRECTION ( 'NONE',  ( -1.000000000000000000, 0.000000000000000000, 0.000000000000000000 ) ) ;
#24318 = EDGE_CURVE ( 'NONE', #9001, #19747, #45801, .T. ) ;
#24319 = EDGE_CURVE ( 'NONE', #28070, #37785, #32521, .T. ) ;
#24320 = VERTEX_POINT ( 'NONE', #43075 ) ;
#24321 = DIRECTION ( 'NONE',  ( 1.000000000000000000, 0.000000000000000000, 0.000000000000000000 ) ) ;
#24322 = ORIENTED_EDGE ( 'NONE', *, *, #44015, .F. ) ;
#24323 = EDGE_CURVE ( 'NONE', #8099, #46550, #7502, .T. ) ;
#24324 = FACE_OUTER_BOUND ( 'NONE', #5320, .T. ) ;
#24325 = CARTESIAN_POINT ( 'NONE',  ( 10.00000000000000178, 12.24744871391589385, -2.499999999999995559 ) ) ;
#24326 = VERTEX_POINT ( 'NONE', #39157 ) ;
#24327 = AXIS2_PLACEMENT_3D ( 'NONE', #8934, #13339, #39542 ) ;
#24328 = AXIS2_PLACEMENT_3D ( 'NONE', #12202, #15858, #27360 ) ;
#24329 = FACE_OUTER_BOUND ( 'NONE', #28036, .T. ) ;
#24330 = ORIENTED_EDGE ( 'NONE', *, *, #21248, .T. ) ;
#24331 = ORIENTED_EDGE ( 'NONE', *, *, #35704, .T. ) ;
#24332 = AXIS2_PLACEMENT_3D ( 'NONE', #25911, #3646, #40850 ) ;
#24333 = VECTOR ( 'NONE', #7806, 1000.000000000000000 ) ;
#24334 = CARTESIAN_POINT ( 'NONE',  ( 11.99999999999999822, 72.35432306680455383, 20.40083707023012494 ) ) ;
#24335 = CARTESIAN_POINT ( 'NONE',  ( 10.00000000000000000, 0.000000000000000000, 0.000000000000000000 ) ) ;
#24336 = DIRECTION ( 'NONE',  ( 0.000000000000000000, 0.000000000000000000, 1.000000000000000000 ) ) ;
#24337 = AXIS2_PLACEMENT_3D ( 'NONE', #43077, #35727, #42841 ) ;
#24338 = ORIENTED_EDGE ( 'NONE', *, *, #28584, .T. ) ;
#24339 = DIRECTION ( 'NONE',  ( -1.000000000000000000, -0.000000000000000000, -0.000000000000000000 ) ) ;
#24340 = ORIENTED_EDGE ( 'NONE', *, *, #24386, .F. ) ;
#24341 = ORIENTED_EDGE ( 'NONE', *, *, #22635, .F. ) ;
#24342 = DIRECTION ( 'NONE',  ( 0.2306669878475637314, 0.9730327541852493711, -0.000000000000000000 ) ) ;
#24343 = LINE ( 'NONE', #1596, #20765 ) ;
#24344 = CARTESIAN_POINT ( 'NONE',  ( 10.00000000000000000, 0.000000000000000000, 0.000000000000000000 ) ) ;
#24345 = VERTEX_POINT ( 'NONE', #17593 ) ;
#24346 = VERTEX_POINT ( 'NONE', #9774 ) ;
#24347 = FACE_BOUND ( 'NONE', #5559, .T. ) ;
#24348 = ORIENTED_EDGE ( 'NONE', *, *, #36461, .T. ) ;
#24349 = CARTESIAN_POINT ( 'NONE',  ( 11.99999999999999822, -72.35160999960831418, 20.41045688087797672 ) ) ;
#24350 = FACE_OUTER_BOUND ( 'NONE', #29397, .T. ) ;
#24351 = CARTESIAN_POINT ( 'NONE',  ( 12.50000000000000000, -120.0000000000000000, -40.00000000000000711 ) ) ;
#24352 = CARTESIAN_POINT ( 'NONE',  ( 0.000000000000000000, 51.03279382321088065, 55.19960302592086521 ) ) ;
#24353 = CARTESIAN_POINT ( 'NONE',  ( 10.00000000000000000, 0.000000000000000000, 0.000000000000000000 ) ) ;
#24354 = DIRECTION ( 'NONE',  ( 0.000000000000000000, 0.000000000000000000, 1.000000000000000000 ) ) ;
#24355 = CARTESIAN_POINT ( 'NONE',  ( 0.000000000000000000, 75.54627589209970040, -17.28742895386005785 ) ) ;
#24356 = DIRECTION ( 'NONE',  ( 0.000000000000000000, 0.000000000000000000, 1.000000000000000000 ) ) ;
#24357 = AXIS2_PLACEMENT_3D ( 'NONE', #4570, #15361, #880 ) ;
#24358 = CARTESIAN_POINT ( 'NONE',  ( 10.00000000000000000, -32.34446384429989507, 26.79245525562703278 ) ) ;
#24359 = ADVANCED_FACE ( 'NONE', ( #2657 ), #6115, .T. ) ;
#24360 = PLANE ( 'NONE',  #2033 ) ;
#24361 = ORIENTED_EDGE ( 'NONE', *, *, #47591, .F. ) ;
#24362 = AXIS2_PLACEMENT_3D ( 'NONE', #45591, #22841, #11366 ) ;
#24363 = FACE_OUTER_BOUND ( 'NONE', #7684, .T. ) ;
#24364 = EDGE_CURVE ( 'NONE', #24727, #46139, #26270, .T. ) ;
#24365 = CIRCLE ( 'NONE', #30625, 42.00000000000000000 ) ;
#24366 = DIRECTION ( 'NONE',  ( 0.000000000000000000, -0.1045284632676570791, 0.9945218953682730678 ) ) ;
#24367 = AXIS2_PLACEMENT_3D ( 'NONE', #47819, #21403, #13584 ) ;
#24368 = DIRECTION ( 'NONE',  ( -1.000000000000000000, -0.000000000000000000, -0.000000000000000000 ) ) ;
#24369 = EDGE_CURVE ( 'NONE', #34495, #16571, #45028, .T. ) ;
#24370 = CIRCLE ( 'NONE', #7942, 37.49900000000000233 ) ;
#24371 = DIRECTION ( 'NONE',  ( 0.000000000000000000, 0.7071067811865486830, -0.7071067811865463515 ) ) ;
#24372 = DIRECTION ( 'NONE',  ( -1.000000000000000000, 0.000000000000000000, 0.000000000000000000 ) ) ;
#24373 = ADVANCED_FACE ( 'NONE', ( #43783 ), #10251, .T. ) ;
#24374 = CARTESIAN_POINT ( 'NONE',  ( 0.000000000000000000, 36.13751322684419165, 21.40280677340384585 ) ) ;
#24375 = DIRECTION ( 'NONE',  ( -0.000000000000000000, 0.5877852522924696954, 0.8090169943749498938 ) ) ;
#24376 = EDGE_LOOP ( 'NONE', ( #27648, #7720, #18909, #2042 ) ) ;
#24377 = EDGE_CURVE ( 'NONE', #39658, #9486, #18790, .T. ) ;
#24378 = FACE_OUTER_BOUND ( 'NONE', #14690, .T. ) ;
#24379 = ADVANCED_FACE ( 'NONE', ( #14895 ), #3634, .T. ) ;
#24380 = ORIENTED_EDGE ( 'NONE', *, *, #44544, .F. ) ;
#24381 = FACE_OUTER_BOUND ( 'NONE', #37834, .T. ) ;
#24382 = ORIENTED_EDGE ( 'NONE', *, *, #14984, .T. ) ;
#24383 = ORIENTED_EDGE ( 'NONE', *, *, #7397, .F. ) ;
#24384 = CARTESIAN_POINT ( 'NONE',  ( 0.000000000000000000, -33.71516098798685590, -74.74816331893465815 ) ) ;
#24385 = VERTEX_POINT ( 'NONE', #29816 ) ;
#24386 = EDGE_CURVE ( 'NONE', #908, #36805, #15337, .T. ) ;
#24387 = EDGE_LOOP ( 'NONE', ( #16932, #24656, #30534, #43187 ) ) ;
#24388 = AXIS2_PLACEMENT_3D ( 'NONE', #34121, #596, #10891 ) ;
#24389 = CARTESIAN_POINT ( 'NONE',  ( 0.000000000000000000, 0.000000000000000000, 125.0000000000000000 ) ) ;
#24390 = VECTOR ( 'NONE', #26220, 1000.000000000000114 ) ;
#24392 = ORIENTED_EDGE ( 'NONE', *, *, #44532, .F. ) ;
#24391 = CARTESIAN_POINT ( 'NONE',  ( 0.000000000000000000, 0.000000000000000000, 0.000000000000000000 ) ) ;
#24393 = EDGE_LOOP ( 'NONE', ( #23242, #16627, #38995, #265 ) ) ;
#24394 = ORIENTED_EDGE ( 'NONE', *, *, #38592, .T. ) ;
#24395 = ORIENTED_EDGE ( 'NONE', *, *, #36190, .F. ) ;
#24396 = AXIS2_PLACEMENT_3D ( 'NONE', #42743, #35131, #5774 ) ;
#24397 = DIRECTION ( 'NONE',  ( 0.3853207896976533209, -0.9227826878668545785, 0.000000000000000000 ) ) ;
#24399 = ORIENTED_EDGE ( 'NONE', *, *, #27544, .T. ) ;
#24398 = CARTESIAN_POINT ( 'NONE',  ( 0.000000000000000000, -40.65526001592664329, 71.21200624218782593 ) ) ;
#24400 = DIRECTION ( 'NONE',  ( 1.000000000000000000, 0.000000000000000000, 0.000000000000000000 ) ) ;
#24401 = EDGE_CURVE ( 'NONE', #9128, #3813, #4366, .T. ) ;
#24402 = ORIENTED_EDGE ( 'NONE', *, *, #42812, .F. ) ;
#24403 = ORIENTED_EDGE ( 'NONE', *, *, #46316, .F. ) ;
#24404 = LINE ( 'NONE', #47411, #38007 ) ;
#24405 = ORIENTED_EDGE ( 'NONE', *, *, #10526, .T. ) ;
#24406 = CARTESIAN_POINT ( 'NONE',  ( 11.99999999999999822, -50.95692526931287603, -58.39081064771804819 ) ) ;
#24407 = CARTESIAN_POINT ( 'NONE',  ( 0.000000000000000000, 63.18004540533092239, -44.88180994100307686 ) ) ;
#24408 = CIRCLE ( 'NONE', #32250, 31.99999999999998579 ) ;
#24409 = ADVANCED_FACE ( 'NONE', ( #4124 ), #19036, .T. ) ;
#24410 = DIRECTION ( 'NONE',  ( -1.000000000000000000, 0.000000000000000000, 0.000000000000000000 ) ) ;
#24411 = LINE ( 'NONE', #39346, #15908 ) ;
#24412 = CARTESIAN_POINT ( 'NONE',  ( 0.000000000000000000, -2.446882695291883605E-15, -2.499999999999983569 ) ) ;
#24413 = EDGE_CURVE ( 'NONE', #14963, #3188, #3876, .T. ) ;
#24414 = ORIENTED_EDGE ( 'NONE', *, *, #31038, .T. ) ;
#24415 = ORIENTED_EDGE ( 'NONE', *, *, #47501, .F. ) ;
#24416 = CYLINDRICAL_SURFACE ( 'NONE', #11026, 16.00000000000000000 ) ;
#24417 = DIRECTION ( 'NONE',  ( 0.02332147558787931590, 0.9997280174009348652, -0.000000000000000000 ) ) ;
#24418 = EDGE_LOOP ( 'NONE', ( #17925, #33434, #42406, #23733 ) ) ;
#24419 = CARTESIAN_POINT ( 'NONE',  ( 0.000000000000000000, 0.000000000000000000, 0.000000000000000000 ) ) ;
#24420 = VERTEX_POINT ( 'NONE', #21746 ) ;
#24421 = AXIS2_PLACEMENT_3D ( 'NONE', #31069, #696, #41832 ) ;
#24422 = FACE_OUTER_BOUND ( 'NONE', #30743, .T. ) ;
#24423 = DIRECTION ( 'NONE',  ( 1.000000000000000000, -0.000000000000000000, -0.000000000000000000 ) ) ;
#24424 = LINE ( 'NONE', #6085, #9731 ) ;
#24425 = EDGE_LOOP ( 'NONE', ( #16776, #47234, #42408, #22773 ) ) ;
#24426 = DIRECTION ( 'NONE',  ( 0.000000000000000000, 0.000000000000000000, 1.000000000000000000 ) ) ;
#24427 = EDGE_CURVE ( 'NONE', #23222, #4970, #7055, .T. ) ;
#24428 = EDGE_CURVE ( 'NONE', #17321, #42306, #29579, .T. ) ;
#24429 = ADVANCED_FACE ( 'NONE', ( #47925 ), #450, .T. ) ;
#24430 = SURFACE_STYLE_USAGE ( .BOTH. , #13182 ) ;
#24432 = AXIS2_PLACEMENT_3D ( 'NONE', #14751, #14514, #45320 ) ;
#24431 = CARTESIAN_POINT ( 'NONE',  ( 10.00000000000000000, -26.01480285779885904, 70.53064760720306481 ) ) ;
#24434 = ORIENTED_EDGE ( 'NONE', *, *, #41245, .F. ) ;
#24433 = VECTOR ( 'NONE', #37486, 1000.000000000000000 ) ;
#24435 = DIRECTION ( 'NONE',  ( 0.000000000000000000, -0.6691306063588661202, -0.7431448254773871387 ) ) ;
#24436 = CARTESIAN_POINT ( 'NONE',  ( 0.000000000000000000, -55.16347631942998220, -60.67117009219196433 ) ) ;
#24437 = LINE ( 'NONE', #43532, #18418 ) ;
#24438 = AXIS2_PLACEMENT_3D ( 'NONE', #47172, #35908, #43514 ) ;
#24439 = CIRCLE ( 'NONE', #22891, 77.49900000000000944 ) ;
#24440 = DIRECTION ( 'NONE',  ( 0.000000000000000000, 0.000000000000000000, 1.000000000000000000 ) ) ;
#24441 = AXIS2_PLACEMENT_3D ( 'NONE', #16255, #11612, #27269 ) ;
#24442 = PRODUCT_DEFINITION ( 'UNKNOWN', '', #23305, #3173 ) ;
#24443 = ORIENTED_EDGE ( 'NONE', *, *, #39415, .F. ) ;
#24444 = VECTOR ( 'NONE', #23883, 1000.000000000000227 ) ;
#24445 = AXIS2_PLACEMENT_3D ( 'NONE', #13805, #9624, #24575 ) ;
#24446 = CARTESIAN_POINT ( 'NONE',  ( 0.000000000000000000, 0.000000000000000000, 0.000000000000000000 ) ) ;
#24447 = CARTESIAN_POINT ( 'NONE',  ( 0.000000000000000000, -46.11716303203233736, 67.80270845531873647 ) ) ;
#24448 = ORIENTED_EDGE ( 'NONE', *, *, #13926, .T. ) ;
#24449 = DIRECTION ( 'NONE',  ( 0.000000000000000000, 0.2079116908177664758, -0.9781476007338042455 ) ) ;
#24450 = FACE_OUTER_BOUND ( 'NONE', #25351, .T. ) ;
#24451 = ORIENTED_EDGE ( 'NONE', *, *, #16518, .T. ) ;
#24452 = ORIENTED_EDGE ( 'NONE', *, *, #32614, .F. ) ;
#24453 = ORIENTED_EDGE ( 'NONE', *, *, #15737, .T. ) ;
#24454 = VECTOR ( 'NONE', #19146, 1000.000000000000000 ) ;
#24455 = EDGE_LOOP ( 'NONE', ( #33248, #4263, #8141, #26760 ) ) ;
#24456 = VECTOR ( 'NONE', #20829, 1000.000000000000000 ) ;
#24457 = DIRECTION ( 'NONE',  ( 0.000000000000000000, 0.000000000000000000, -1.000000000000000000 ) ) ;
#24458 = EDGE_CURVE ( 'NONE', #24955, #22527, #33279, .T. ) ;
#24459 = ORIENTED_EDGE ( 'NONE', *, *, #3252, .T. ) ;
#24460 = VERTEX_POINT ( 'NONE', #41333 ) ;
#24461 = DIRECTION ( 'NONE',  ( 1.000000000000000000, 0.000000000000000000, 0.000000000000000000 ) ) ;
#24462 = VERTEX_POINT ( 'NONE', #22485 ) ;
#24463 = CARTESIAN_POINT ( 'NONE',  ( -18.24502636017238899, -100.7225776329765665, 5.500000000000000000 ) ) ;
#24464 = AXIS2_PLACEMENT_3D ( 'NONE', #5289, #46649, #13112 ) ;
#24465 = AXIS2_PLACEMENT_3D ( 'NONE', #23558, #20134, #12086 ) ;
#24466 = EDGE_CURVE ( 'NONE', #44497, #4911, #44255, .T. ) ;
#24467 = VECTOR ( 'NONE', #9968, 1000.000000000000000 ) ;
#24468 = LINE ( 'NONE', #31353, #14505 ) ;
#24469 = FACE_OUTER_BOUND ( 'NONE', #6047, .T. ) ;
#24470 = EDGE_CURVE ( 'NONE', #27706, #39316, #9105, .T. ) ;
#24471 = AXIS2_PLACEMENT_3D ( 'NONE', #5596, #41840, #34465 ) ;
#24472 = ORIENTED_EDGE ( 'NONE', *, *, #1740, .T. ) ;
#24473 = DIRECTION ( 'NONE',  ( 0.000000000000000000, 0.8660254037844374864, -0.5000000000000019984 ) ) ;
#24474 = VERTEX_POINT ( 'NONE', #22245 ) ;
#24475 = DIRECTION ( 'NONE',  ( 0.7273375899149793211, -0.6862798483830554463, 0.000000000000000000 ) ) ;
#24476 = DIRECTION ( 'NONE',  ( -1.000000000000000000, 0.000000000000000000, 0.000000000000000000 ) ) ;
#24477 = CIRCLE ( 'NONE', #36175, 31.99999999999999289 ) ;
#24478 = CARTESIAN_POINT ( 'NONE',  ( -1.250000000000002442, -12.36245420541525242, 0.000000000000000000 ) ) ;
#24479 = VERTEX_POINT ( 'NONE', #44022 ) ;
#24480 = ORIENTED_EDGE ( 'NONE', *, *, #22520, .T. ) ;
#24481 = DIRECTION ( 'NONE',  ( 0.000000000000000000, 0.000000000000000000, 1.000000000000000000 ) ) ;
#24482 = FACE_OUTER_BOUND ( 'NONE', #33287, .T. ) ;
#24483 = ORIENTED_EDGE ( 'NONE', *, *, #43617, .T. ) ;
#24484 = CIRCLE ( 'NONE', #44047, 77.49900000000000944 ) ;
#24485 = LINE ( 'NONE', #1989, #32408 ) ;
#24486 = DIRECTION ( 'NONE',  ( -1.000000000000000000, 0.000000000000000000, 0.000000000000000000 ) ) ;
#24487 = DIRECTION ( 'NONE',  ( 0.9730327541852497042, -0.2306669878475622604, 0.000000000000000000 ) ) ;
#24488 = LINE ( 'NONE', #12754, #47653 ) ;
#24489 = EDGE_CURVE ( 'NONE', #38387, #43468, #18066, .T. ) ;
#24490 = ADVANCED_FACE ( 'NONE', ( #18565 ), #21982, .T. ) ;
#24491 = LINE ( 'NONE', #9316, #9913 ) ;
#24492 = FACE_OUTER_BOUND ( 'NONE', #32415, .T. ) ;
#24493 = DIRECTION ( 'NONE',  ( -1.000000000000000000, 0.000000000000000000, 0.000000000000000000 ) ) ;
#24494 = CARTESIAN_POINT ( 'NONE',  ( 11.99999999999999822, 68.67312586195046720, -35.91791733033404199 ) ) ;
#24495 = DIRECTION ( 'NONE',  ( 0.000000000000000000, 0.000000000000000000, 1.000000000000000000 ) ) ;
#24497 = CIRCLE ( 'NONE', #29939, 77.49899999999999523 ) ;
#24496 =( NAMED_UNIT ( * ) PLANE_ANGLE_UNIT ( ) SI_UNIT ( $, .RADIAN. ) );
#24498 = CYLINDRICAL_SURFACE ( 'NONE', #12450, 16.00000000000000000 ) ;
#24499 = DIRECTION ( 'NONE',  ( 0.000000000000000000, 0.000000000000000000, -1.000000000000000000 ) ) ;
#24500 = EDGE_LOOP ( 'NONE', ( #25946, #12658, #28852, #1440 ) ) ;
#24501 = AXIS2_PLACEMENT_3D ( 'NONE', #12707, #22991, #27639 ) ;
#24502 = EDGE_CURVE ( 'NONE', #9321, #9223, #31773, .T. ) ;
#24503 = ORIENTED_EDGE ( 'NONE', *, *, #41648, .T. ) ;
#24504 = DIRECTION ( 'NONE',  ( 1.000000000000000000, 1.387778780781445478E-15, 0.000000000000000000 ) ) ;
#24505 = DIRECTION ( 'NONE',  ( 0.000000000000000000, 0.000000000000000000, 1.000000000000000000 ) ) ;
#24506 = CIRCLE ( 'NONE', #44027, 82.00000000000000000 ) ;
#24507 = AXIS2_PLACEMENT_3D ( 'NONE', #32102, #38967, #13486 ) ;
#24508 = CARTESIAN_POINT ( 'NONE',  ( 11.99999999999999822, -72.35432306680469594, -20.40083707022958848 ) ) ;
#24509 = AXIS2_PLACEMENT_3D ( 'NONE', #38590, #38340, #38841 ) ;
#24510 = ORIENTED_EDGE ( 'NONE', *, *, #25398, .T. ) ;
#24511 = ORIENTED_EDGE ( 'NONE', *, *, #43267, .F. ) ;
#24512 = AXIS2_PLACEMENT_3D ( 'NONE', #16696, #20596, #36003 ) ;
#24513 = AXIS2_PLACEMENT_3D ( 'NONE', #13358, #43696, #25085 ) ;
#24514 = AXIS2_PLACEMENT_3D ( 'NONE', #46284, #9312, #19835 ) ;
#24515 = FACE_OUTER_BOUND ( 'NONE', #46486, .T. ) ;
#24516 = AXIS2_PLACEMENT_3D ( 'NONE', #17103, #46013, #38913 ) ;
#24517 = EDGE_LOOP ( 'NONE', ( #1074, #23622, #44936, #15320 ) ) ;
#24518 = CYLINDRICAL_SURFACE ( 'NONE', #31588, 31.99999999999998579 ) ;
#24519 = EDGE_LOOP ( 'NONE', ( #47120, #15418, #24361, #43587, #771, #31343 ) ) ;
#24520 = SURFACE_SIDE_STYLE ('',( #31891 ) ) ;
#24521 = VECTOR ( 'NONE', #23858, 1000.000000000000114 ) ;
#24522 = DIRECTION ( 'NONE',  ( 1.000000000000000000, 0.000000000000000000, 0.000000000000000000 ) ) ;
#24523 = CARTESIAN_POINT ( 'NONE',  ( 10.00000000000000000, 0.000000000000000000, 0.000000000000000000 ) ) ;
#24524 = VERTEX_POINT ( 'NONE', #25897 ) ;
#24526 = VERTEX_POINT ( 'NONE', #7298 ) ;
#24525 = DIRECTION ( 'NONE',  ( 0.000000000000000000, 0.000000000000000000, -1.000000000000000000 ) ) ;
#24527 = ORIENTED_EDGE ( 'NONE', *, *, #27644, .T. ) ;
#24528 = EDGE_CURVE ( 'NONE', #41278, #5585, #23145, .T. ) ;
#24529 = DIRECTION ( 'NONE',  ( 1.000000000000000000, -9.814797785686868941E-17, 0.000000000000000000 ) ) ;
#24530 = EDGE_CURVE ( 'NONE', #47530, #16794, #14570, .T. ) ;
#24531 = DIRECTION ( 'NONE',  ( 0.000000000000000000, 0.000000000000000000, 1.000000000000000000 ) ) ;
#24532 = DIRECTION ( 'NONE',  ( -0.8774505977381978905, -0.4796670183876304283, 0.000000000000000000 ) ) ;
#24533 = AXIS2_PLACEMENT_3D ( 'NONE', #48393, #30046, #26132 ) ;
#24534 = DIRECTION ( 'NONE',  ( -1.000000000000000000, 0.000000000000000000, 0.000000000000000000 ) ) ;
#24535 = CIRCLE ( 'NONE', #18270, 77.49899999999999523 ) ;
#24536 = CARTESIAN_POINT ( 'NONE',  ( -10.00000000000000000, 0.000000000000000000, 0.000000000000000000 ) ) ;
#24537 = VERTEX_POINT ( 'NONE', #19504 ) ;
#24538 = CARTESIAN_POINT ( 'NONE',  ( 15.00000000000000000, -22.67460108101774452, 6.353146135318220367 ) ) ;
#24539 = ORIENTED_EDGE ( 'NONE', *, *, #44734, .T. ) ;
#24540 = VERTEX_POINT ( 'NONE', #45239 ) ;
#24541 = ADVANCED_FACE ( 'NONE', ( #26883 ), #8278, .T. ) ;
#24542 = AXIS2_PLACEMENT_3D ( 'NONE', #2747, #28710, #31677 ) ;
#24543 = LINE ( 'NONE', #2495, #40334 ) ;
#24544 = CIRCLE ( 'NONE', #36237, 37.49900000000000233 ) ;
#24545 = AXIS2_PLACEMENT_3D ( 'NONE', #4036, #27281, #26552 ) ;
#24546 = DIRECTION ( 'NONE',  ( -1.000000000000000000, 0.000000000000000000, 0.000000000000000000 ) ) ;
#24547 = DIRECTION ( 'NONE',  ( 0.000000000000000000, 0.000000000000000000, 1.000000000000000000 ) ) ;
#24548 = DIRECTION ( 'NONE',  ( -1.000000000000000000, 0.000000000000000000, 0.000000000000000000 ) ) ;
#24549 = VERTEX_POINT ( 'NONE', #12436 ) ;
#24550 = DIRECTION ( 'NONE',  ( 0.000000000000000000, 0.000000000000000000, -1.000000000000000000 ) ) ;
#24551 = LINE ( 'NONE', #2503, #39818 ) ;
#24552 = DIRECTION ( 'NONE',  ( -1.000000000000000000, 0.000000000000000000, -0.000000000000000000 ) ) ;
#24553 = EDGE_CURVE ( 'NONE', #24690, #13149, #23967, .T. ) ;
#24554 = CARTESIAN_POINT ( 'NONE',  ( 11.99999999999999822, -73.73191006444582740, 14.66109333815435889 ) ) ;
#24555 = PLANE ( 'NONE',  #45032 ) ;
#24556 = VERTEX_POINT ( 'NONE', #5095 ) ;
#24557 = AXIS2_PLACEMENT_3D ( 'NONE', #46439, #17277, #36380 ) ;
#24558 = CIRCLE ( 'NONE', #44072, 77.49900000000000944 ) ;
#24559 = CARTESIAN_POINT ( 'NONE',  ( 5.000000000000002665, 71.21200624218852226, -40.65526001592539984 ) ) ;
#24560 = ADVANCED_FACE ( 'NONE', ( #23937 ), #27363, .F. ) ;
#24561 = DIRECTION ( 'NONE',  ( 0.000000000000000000, 0.9238795325112878487, -0.3826834323650874503 ) ) ;
#24562 = DIRECTION ( 'NONE',  ( -0.1276937514489705217, -0.9918136447140101231, 0.000000000000000000 ) ) ;
#24564 = AXIS2_PLACEMENT_3D ( 'NONE', #6852, #13470, #21767 ) ;
#24563 = DIRECTION ( 'NONE',  ( 0.000000000000000000, 0.6691306063588579045, -0.7431448254773945772 ) ) ;
#24565 = AXIS2_PLACEMENT_3D ( 'NONE', #38230, #7825, #30119 ) ;
#24566 = CARTESIAN_POINT ( 'NONE',  ( 12.13205353604972991, -140.1820037904669789, -5.500000000000000000 ) ) ;
#24567 = CARTESIAN_POINT ( 'NONE',  ( -35.37301231164799731, -117.0000000000000000, -2.500000000000000000 ) ) ;
#24568 = CIRCLE ( 'NONE', #16742, 31.99999999999997868 ) ;
#24569 = EDGE_CURVE ( 'NONE', #15076, #31175, #20010, .T. ) ;
#24570 = EDGE_LOOP ( 'NONE', ( #43570, #8083, #39620, #42246 ) ) ;
#24571 = DIRECTION ( 'NONE',  ( 0.000000000000000000, 0.000000000000000000, 1.000000000000000000 ) ) ;
#24572 = ORIENTED_EDGE ( 'NONE', *, *, #4905, .T. ) ;
#24573 = LINE ( 'NONE', #32860, #1872 ) ;
#24574 = VERTEX_POINT ( 'NONE', #34941 ) ;
#24575 = DIRECTION ( 'NONE',  ( 0.000000000000000000, 0.000000000000000000, 1.000000000000000000 ) ) ;
#24576 = ORIENTED_EDGE ( 'NONE', *, *, #13086, .F. ) ;
#24577 = EDGE_CURVE ( 'NONE', #23219, #13751, #13031, .T. ) ;
#24578 = AXIS2_PLACEMENT_3D ( 'NONE', #41836, #209, #26175 ) ;
#24579 = CIRCLE ( 'NONE', #41808, 31.99999999999999645 ) ;
#24580 = CARTESIAN_POINT ( 'NONE',  ( 10.00000000000000000, 6.736453364083557105, 36.88895765772635826 ) ) ;
#24581 = ORIENTED_EDGE ( 'NONE', *, *, #34579, .F. ) ;
#24582 = VECTOR ( 'NONE', #6890, 1000.000000000000000 ) ;
#24583 = ORIENTED_EDGE ( 'NONE', *, *, #9334, .F. ) ;
#24584 = AXIS2_PLACEMENT_3D ( 'NONE', #37824, #26566, #4309 ) ;
#24585 = AXIS2_PLACEMENT_3D ( 'NONE', #37740, #30407, #11800 ) ;
#24586 = CARTESIAN_POINT ( 'NONE',  ( 0.000000000000000000, -22.48208911017474065, -35.47612816024548721 ) ) ;
#24587 = AXIS2_PLACEMENT_3D ( 'NONE', #17801, #36159, #32502 ) ;
#24588 = EDGE_CURVE ( 'NONE', #32422, #8858, #8746, .T. ) ;
#24589 = CARTESIAN_POINT ( 'NONE',  ( -10.90076147243505211, 0.000000000000000000, 0.000000000000000000 ) ) ;
#24590 = CIRCLE ( 'NONE', #3484, 77.49899999999999523 ) ;
#24592 = ORIENTED_EDGE ( 'NONE', *, *, #18050, .T. ) ;
#24591 = DIRECTION ( 'NONE',  ( -1.000000000000000000, 0.000000000000000000, -0.000000000000000000 ) ) ;
#24593 = ORIENTED_EDGE ( 'NONE', *, *, #42206, .T. ) ;
#24594 = EDGE_CURVE ( 'NONE', #26813, #28893, #38377, .T. ) ;
#24595 = DIRECTION ( 'NONE',  ( 0.000000000000000000, 0.7431448254773862505, 0.6691306063588672304 ) ) ;
#24596 = EDGE_LOOP ( 'NONE', ( #20180, #33901, #42097, #2357 ) ) ;
#24597 = CARTESIAN_POINT ( 'NONE',  ( 10.00000000000000000, 0.000000000000000000, 0.000000000000000000 ) ) ;
#24598 = DIRECTION ( 'NONE',  ( -1.000000000000000000, 0.000000000000000000, -0.000000000000000000 ) ) ;
#24599 = CARTESIAN_POINT ( 'NONE',  ( 10.00000000000000000, 33.17418723428333749, -17.67226234102790272 ) ) ;
#24600 = ORIENTED_EDGE ( 'NONE', *, *, #1456, .F. ) ;
#24601 = ORIENTED_EDGE ( 'NONE', *, *, #25823, .T. ) ;
#24602 = EDGE_LOOP ( 'NONE', ( #5141, #23498, #40407, #36124 ) ) ;
#24603 = CARTESIAN_POINT ( 'NONE',  ( 0.000000000000000000, 0.000000000000000000, 0.000000000000000000 ) ) ;
#24604 = ORIENTED_EDGE ( 'NONE', *, *, #8979, .T. ) ;
#24605 = EDGE_CURVE ( 'NONE', #14595, #43138, #48163, .T. ) ;
#24606 = FACE_BOUND ( 'NONE', #20370, .T. ) ;
#24607 = CARTESIAN_POINT ( 'NONE',  ( 0.000000000000000000, 27.05870788708267582, -26.08949754952995903 ) ) ;
#24608 = CARTESIAN_POINT ( 'NONE',  ( 10.00000000000000000, 74.65374052328648702, 8.840884882375350529 ) ) ;
#24609 = DIRECTION ( 'NONE',  ( 0.000000000000000000, 0.000000000000000000, -1.000000000000000000 ) ) ;
#24610 = CARTESIAN_POINT ( 'NONE',  ( 11.99999999999999822, 0.000000000000000000, 0.000000000000000000 ) ) ;
#24611 = DIRECTION ( 'NONE',  ( -1.000000000000000000, -0.000000000000000000, 0.000000000000000000 ) ) ;
#24612 = CARTESIAN_POINT ( 'NONE',  ( 10.00000000000000000, 6.555932627142418312, 37.01155633439060466 ) ) ;
#24613 = CARTESIAN_POINT ( 'NONE',  ( 10.00000000000000000, 10.96151621346487914, 35.95386929396260456 ) ) ;
#24614 = FACE_OUTER_BOUND ( 'NONE', #4011, .T. ) ;
#24615 = CARTESIAN_POINT ( 'NONE',  ( 0.000000000000000000, 14.67089635893713684, 73.72996012237443608 ) ) ;
#24616 = ORIENTED_EDGE ( 'NONE', *, *, #13635, .F. ) ;
#24617 = CARTESIAN_POINT ( 'NONE',  ( 0.000000000000000000, 59.03342792756328095, -46.54456581323744757 ) ) ;
#24618 = AXIS2_PLACEMENT_3D ( 'NONE', #40267, #6724, #17732 ) ;
#24619 = CARTESIAN_POINT ( 'NONE',  ( 0.000000000000000000, 29.01471420065564644, 76.69515212746026123 ) ) ;
#24620 = DIRECTION ( 'NONE',  ( 0.000000000000000000, -0.8526401643540860720, -0.5224985647159589019 ) ) ;
#24621 = DIRECTION ( 'NONE',  ( -1.000000000000000000, 0.000000000000000000, -0.000000000000000000 ) ) ;
#24622 = ADVANCED_FACE ( 'NONE', ( #37898 ), #41571, .T. ) ;
#24623 = VERTEX_POINT ( 'NONE', #34440 ) ;
#24624 = AXIS2_PLACEMENT_3D ( 'NONE', #1031, #30925, #22593 ) ;
#24625 = VECTOR ( 'NONE', #46420, 999.9999999999998863 ) ;
#24626 = DIRECTION ( 'NONE',  ( -0.000000000000000000, -0.000000000000000000, -1.000000000000000000 ) ) ;
#24627 = DIRECTION ( 'NONE',  ( 0.000000000000000000, 0.000000000000000000, 1.000000000000000000 ) ) ;
#24628 = VERTEX_POINT ( 'NONE', #8021 ) ;
#24629 = LINE ( 'NONE', #39573, #4299 ) ;
#24630 = AXIS2_PLACEMENT_3D ( 'NONE', #40855, #48198, #18335 ) ;
#24631 = ORIENTED_EDGE ( 'NONE', *, *, #29765, .F. ) ;
#24632 = FACE_OUTER_BOUND ( 'NONE', #29829, .T. ) ;
#24633 = VECTOR ( 'NONE', #2806, 1000.000000000000000 ) ;
#24634 = ORIENTED_EDGE ( 'NONE', *, *, #30913, .T. ) ;
#24635 = ORIENTED_EDGE ( 'NONE', *, *, #15889, .T. ) ;
#24636 = EDGE_CURVE ( 'NONE', #31998, #14073, #36453, .T. ) ;
#24637 = FACE_OUTER_BOUND ( 'NONE', #26836, .T. ) ;
#24638 = EDGE_LOOP ( 'NONE', ( #42040, #9298, #10510, #14703 ) ) ;
#24639 = VERTEX_POINT ( 'NONE', #27603 ) ;
#24640 = AXIS2_PLACEMENT_3D ( 'NONE', #13302, #47318, #9374 ) ;
#24641 = ADVANCED_FACE ( 'NONE', ( #26636 ), #27131, .T. ) ;
#24642 = CARTESIAN_POINT ( 'NONE',  ( 0.000000000000000000, -14.66109333815513160, 73.73191006444567108 ) ) ;
#24643 = VECTOR ( 'NONE', #30443, 1000.000000000000114 ) ;
#24645 = ORIENTED_EDGE ( 'NONE', *, *, #37768, .T. ) ;
#24644 = DIRECTION ( 'NONE',  ( 0.000000000000000000, 0.8526401643540897357, 0.5224985647159527957 ) ) ;
#24646 = ORIENTED_EDGE ( 'NONE', *, *, #1703, .F. ) ;
#24647 = EDGE_LOOP ( 'NONE', ( #43183, #13974, #15684, #18079 ) ) ;
#24648 = EDGE_CURVE ( 'NONE', #4757, #45468, #15616, .T. ) ;
#24649 = VERTEX_POINT ( 'NONE', #31052 ) ;
#24650 = CARTESIAN_POINT ( 'NONE',  ( 5.000000000000000000, -51.29473840253270112, 63.97538442413407012 ) ) ;
#24652 = VERTEX_POINT ( 'NONE', #45469 ) ;
#24651 = DIRECTION ( 'NONE',  ( -0.9966891607226785466, -0.08130631524009969413, 0.000000000000000000 ) ) ;
#24653 = CARTESIAN_POINT ( 'NONE',  ( 10.00000000000000000, -69.42325613327466272, 34.44570377933573724 ) ) ;
#24654 = AXIS2_PLACEMENT_3D ( 'NONE', #26279, #18904, #7665 ) ;
#24655 = CIRCLE ( 'NONE', #1212, 32.00000000000000000 ) ;
#24656 = ORIENTED_EDGE ( 'NONE', *, *, #12249, .F. ) ;
#24657 = ORIENTED_EDGE ( 'NONE', *, *, #26934, .F. ) ;
#24658 = CARTESIAN_POINT ( 'NONE',  ( 0.000000000000000000, 0.000000000000000000, 0.000000000000000000 ) ) ;
#24659 = ORIENTED_EDGE ( 'NONE', *, *, #25487, .T. ) ;
#24660 = EDGE_CURVE ( 'NONE', #38904, #14239, #11953, .T. ) ;
#24661 = CARTESIAN_POINT ( 'NONE',  ( 10.00000000000000000, 0.000000000000000000, 0.000000000000000000 ) ) ;
#24662 = FACE_OUTER_BOUND ( 'NONE', #44151, .T. ) ;
#24663 = AXIS2_PLACEMENT_3D ( 'NONE', #26300, #18467, #26540 ) ;
#24664 = ADVANCED_FACE ( 'NONE', ( #12205 ), #8505, .T. ) ;
#24665 = LINE ( 'NONE', #5343, #44766 ) ;
#24666 = DIRECTION ( 'NONE',  ( 1.000000000000000000, 0.000000000000000000, 0.000000000000000000 ) ) ;
#24667 = CARTESIAN_POINT ( 'NONE',  ( 10.00000000000000000, 46.11716303203284184, -67.80270845531838120 ) ) ;
#24668 = AXIS2_PLACEMENT_3D ( 'NONE', #15808, #42006, #38569 ) ;
#24669 = CIRCLE ( 'NONE', #38756, 82.00000000000000000 ) ;
#24670 = CARTESIAN_POINT ( 'NONE',  ( -10.00000000000000000, 0.000000000000000000, 0.000000000000000000 ) ) ;
#24671 = CARTESIAN_POINT ( 'NONE',  ( 0.000000000000000000, 0.000000000000000000, 0.000000000000000000 ) ) ;
#24672 = ORIENTED_EDGE ( 'NONE', *, *, #36630, .T. ) ;
#24673 = LINE ( 'NONE', #27619, #13957 ) ;
#24674 = ORIENTED_EDGE ( 'NONE', *, *, #45312, .F. ) ;
#24675 = DIRECTION ( 'NONE',  ( -1.000000000000000000, 0.000000000000000000, 0.000000000000000000 ) ) ;
#24676 = DIRECTION ( 'NONE',  ( -1.000000000000000000, -0.000000000000000000, -0.000000000000000000 ) ) ;
#24677 = DIRECTION ( 'NONE',  ( 0.000000000000000000, -0.2334453638558921795, -0.9723699203976797767 ) ) ;
#24678 = AXIS2_PLACEMENT_3D ( 'NONE', #42958, #9179, #45911 ) ;
#24679 = ORIENTED_EDGE ( 'NONE', *, *, #6359, .F. ) ;
#24680 = CARTESIAN_POINT ( 'NONE',  ( -12.40464318976454727, 10.41032311384371845, -55.00000000000000000 ) ) ;
#24681 = DIRECTION ( 'NONE',  ( -1.000000000000000000, 0.000000000000000000, 0.000000000000000000 ) ) ;
#24682 = CARTESIAN_POINT ( 'NONE',  ( 10.00000000000000000, -16.45098606841149902, 33.79645857604508308 ) ) ;
#24683 = AXIS2_PLACEMENT_3D ( 'NONE', #30167, #46056, #12046 ) ;
#24684 = ORIENTED_EDGE ( 'NONE', *, *, #25340, .F. ) ;
#24685 = CARTESIAN_POINT ( 'NONE',  ( 10.00000000000000000, -81.90746397400391743, 3.894527615417593847 ) ) ;
#24686 = DIRECTION ( 'NONE',  ( -0.000000000000000000, -0.000000000000000000, 1.000000000000000000 ) ) ;
#24687 = DIRECTION ( 'NONE',  ( -1.000000000000000000, 0.000000000000000000, 0.000000000000000000 ) ) ;
#24688 = CARTESIAN_POINT ( 'NONE',  ( 0.000000000000000000, 0.000000000000000000, 0.000000000000000000 ) ) ;
#24689 = ORIENTED_EDGE ( 'NONE', *, *, #43282, .T. ) ;
#24690 = VERTEX_POINT ( 'NONE', #17291 ) ;
#24691 = VERTEX_POINT ( 'NONE', #1912 ) ;
#24692 = EDGE_CURVE ( 'NONE', #29358, #19822, #18468, .T. ) ;
#24693 = AXIS2_PLACEMENT_3D ( 'NONE', #32296, #46985, #32066 ) ;
#24694 = ADVANCED_FACE ( 'NONE', ( #25120 ), #9964, .T. ) ;
#24695 = AXIS2_PLACEMENT_3D ( 'NONE', #17914, #46602, #9371 ) ;
#24696 = DIRECTION ( 'NONE',  ( -1.000000000000000000, -0.000000000000000000, 0.000000000000000000 ) ) ;
#24697 = CARTESIAN_POINT ( 'NONE',  ( 0.000000000000000000, -26.23277895567245821, -4.042438405570103477 ) ) ;
#24698 = ADVANCED_FACE ( 'NONE', ( #42784 ), #13884, .T. ) ;
#24699 = AXIS2_PLACEMENT_3D ( 'NONE', #13055, #5699, #42911 ) ;
#24700 = ORIENTED_EDGE ( 'NONE', *, *, #38571, .F. ) ;
#24701 = AXIS2_PLACEMENT_3D ( 'NONE', #15055, #7701, #7472 ) ;
#24702 = CYLINDRICAL_SURFACE ( 'NONE', #21879, 31.99999999999999289 ) ;
#24703 = ORIENTED_EDGE ( 'NONE', *, *, #43590, .T. ) ;
#24704 = ORIENTED_EDGE ( 'NONE', *, *, #11552, .F. ) ;
#24705 = VECTOR ( 'NONE', #26250, 1000.000000000000000 ) ;
#24706 = ORIENTED_EDGE ( 'NONE', *, *, #26011, .F. ) ;
#24707 = ADVANCED_FACE ( 'NONE', ( #47166 ), #13638, .F. ) ;
#24708 = AXIS2_PLACEMENT_3D ( 'NONE', #36354, #29252, #32908 ) ;
#24709 = EDGE_CURVE ( 'NONE', #11885, #13391, #7539, .T. ) ;
#24710 = EDGE_CURVE ( 'NONE', #28615, #41574, #5202, .T. ) ;
#24711 = AXIS2_PLACEMENT_3D ( 'NONE', #43046, #46957, #24435 ) ;
#24712 = DIRECTION ( 'NONE',  ( 0.000000000000000000, 0.000000000000000000, 1.000000000000000000 ) ) ;
#24713 = ORIENTED_EDGE ( 'NONE', *, *, #38451, .T. ) ;
#24714 = CARTESIAN_POINT ( 'NONE',  ( -10.00000000000000000, 0.000000000000000000, 0.000000000000000000 ) ) ;
#24715 = ORIENTED_EDGE ( 'NONE', *, *, #27715, .F. ) ;
#24716 = CARTESIAN_POINT ( 'NONE',  ( -16.06301359042743115, -102.7814171781257357, 5.500000000000000000 ) ) ;
#24717 = EDGE_CURVE ( 'NONE', #14664, #16979, #24404, .T. ) ;
#24718 = DIRECTION ( 'NONE',  ( 0.000000000000000000, 0.3090169943749411230, 0.9510565162951555296 ) ) ;
#24719 = DIRECTION ( 'NONE',  ( 1.000000000000000000, -0.000000000000000000, -0.000000000000000000 ) ) ;
#24720 = AXIS2_PLACEMENT_3D ( 'NONE', #42747, #39299, #39064 ) ;
#24721 = VERTEX_POINT ( 'NONE', #2600 ) ;
#24722 = DIRECTION ( 'NONE',  ( 0.000000000000000000, 0.000000000000000000, 1.000000000000000000 ) ) ;
#24723 = ORIENTED_EDGE ( 'NONE', *, *, #47559, .F. ) ;
#24724 = DIRECTION ( 'NONE',  ( 0.000000000000000000, 0.000000000000000000, 1.000000000000000000 ) ) ;
#24725 = DIRECTION ( 'NONE',  ( -1.000000000000000000, 0.000000000000000000, -0.000000000000000000 ) ) ;
#24726 = AXIS2_PLACEMENT_3D ( 'NONE', #5570, #28807, #9238 ) ;
#24727 = VERTEX_POINT ( 'NONE', #17541 ) ;
#24728 = VERTEX_POINT ( 'NONE', #31533 ) ;
#24729 = LINE ( 'NONE', #35250, #41652 ) ;
#24730 = FACE_OUTER_BOUND ( 'NONE', #44063, .T. ) ;
#24731 = ORIENTED_EDGE ( 'NONE', *, *, #34338, .F. ) ;
#24733 = EDGE_CURVE ( 'NONE', #34678, #15200, #37218, .T. ) ;
#24732 = CARTESIAN_POINT ( 'NONE',  ( 10.00000000000000000, 12.42422080174639021, 35.38097989696516521 ) ) ;
#24734 = CIRCLE ( 'NONE', #38010, 77.49899999999999523 ) ;
#24735 = CARTESIAN_POINT ( 'NONE',  ( 10.00000000000000000, 77.49459641780886443, -0.8261519478433788644 ) ) ;
#24736 = DIRECTION ( 'NONE',  ( 0.000000000000000000, 0.000000000000000000, 1.000000000000000000 ) ) ;
#24737 = ORIENTED_EDGE ( 'NONE', *, *, #47467, .T. ) ;
#24738 = FACE_OUTER_BOUND ( 'NONE', #27362, .T. ) ;
#24739 = DIRECTION ( 'NONE',  ( -1.000000000000000000, 0.000000000000000000, 0.000000000000000000 ) ) ;
#24740 = VECTOR ( 'NONE', #48326, 1000.000000000000000 ) ;
#24741 = CIRCLE ( 'NONE', #29316, 32.50000000000000000 ) ;
#24742 = DIRECTION ( 'NONE',  ( -1.000000000000000000, -0.000000000000000000, -0.000000000000000000 ) ) ;
#24743 = DIRECTION ( 'NONE',  ( -0.9781476007338042455, -0.2079116908177664758, 0.000000000000000000 ) ) ;
#24744 = CARTESIAN_POINT ( 'NONE',  ( -10.43921258969510824, -98.89258801967538659, 2.500000000000000000 ) ) ;
#24745 = DIRECTION ( 'NONE',  ( -1.000000000000000000, 0.000000000000000000, 0.000000000000000000 ) ) ;
#24746 = DIRECTION ( 'NONE',  ( -0.000000000000000000, -0.000000000000000000, -1.000000000000000000 ) ) ;
#24747 = VECTOR ( 'NONE', #42413, 1000.000000000000000 ) ;
#24748 = DIRECTION ( 'NONE',  ( -1.000000000000000000, -0.000000000000000000, -0.000000000000000000 ) ) ;
#24749 = DIRECTION ( 'NONE',  ( -0.000000000000000000, 0.9781476007338064660, 0.2079116908177554846 ) ) ;
#24750 = ORIENTED_EDGE ( 'NONE', *, *, #5423, .F. ) ;
#24751 = ORIENTED_EDGE ( 'NONE', *, *, #23060, .F. ) ;
#24752 = AXIS2_PLACEMENT_3D ( 'NONE', #886, #37383, #11457 ) ;
#24753 = ADVANCED_FACE ( 'NONE', ( #39341 ), #43738, .T. ) ;
#24754 = FACE_OUTER_BOUND ( 'NONE', #1192, .T. ) ;
#24755 = CARTESIAN_POINT ( 'NONE',  ( 11.99999999999999822, 34.44570377933693806, -69.42325613327405165 ) ) ;
#24756 = EDGE_CURVE ( 'NONE', #25415, #43483, #25473, .T. ) ;
#24757 = CARTESIAN_POINT ( 'NONE',  ( 0.000000000000000000, 0.000000000000000000, 0.000000000000000000 ) ) ;
#24758 = EDGE_CURVE ( 'NONE', #29067, #38747, #39101, .T. ) ;
#24759 = ORIENTED_EDGE ( 'NONE', *, *, #255, .T. ) ;
#24760 = VECTOR ( 'NONE', #27074, 1000.000000000000000 ) ;
#24761 = CARTESIAN_POINT ( 'NONE',  ( 0.000000000000000000, -76.66974797899828786, -11.30684508768420393 ) ) ;
#24762 = VERTEX_POINT ( 'NONE', #35419 ) ;
#24763 = CARTESIAN_POINT ( 'NONE',  ( -12.50000000000000000, -132.5000000000000000, 40.00000000000000000 ) ) ;
#24764 = AXIS2_PLACEMENT_3D ( 'NONE', #2681, #24962, #27948 ) ;
#24765 = EDGE_LOOP ( 'NONE', ( #36390, #14024, #24009, #9329 ) ) ;
#24766 = LINE ( 'NONE', #29399, #11803 ) ;
#24767 = EDGE_CURVE ( 'NONE', #43974, #39583, #16835, .T. ) ;
#24768 = EDGE_CURVE ( 'NONE', #44062, #35871, #10654, .T. ) ;
#24769 = DIRECTION ( 'NONE',  ( -0.000000000000000000, 0.9781476007338042455, 0.2079116908177664758 ) ) ;
#24770 = AXIS2_PLACEMENT_3D ( 'NONE', #30693, #44901, #19656 ) ;
#24771 = CARTESIAN_POINT ( 'NONE',  ( 13.36581099891334645, -139.3288669181958710, 2.500000000000000000 ) ) ;
#24772 = ORIENTED_EDGE ( 'NONE', *, *, #36575, .T. ) ;
#24773 = CARTESIAN_POINT ( 'NONE',  ( 0.000000000000000000, 65.59268652807210742, 36.72794159290264560 ) ) ;
#24774 = EDGE_LOOP ( 'NONE', ( #34013, #47472, #1886, #10201 ) ) ;
#24775 = CIRCLE ( 'NONE', #37279, 37.49900000000001654 ) ;
#24776 = FACE_BOUND ( 'NONE', #4736, .T. ) ;
#24777 = CARTESIAN_POINT ( 'NONE',  ( -3.000000000000000000, 6.762365576493643893, -25.66652317338391853 ) ) ;
#24778 = DIRECTION ( 'NONE',  ( -1.000000000000000000, 0.000000000000000000, 0.000000000000000000 ) ) ;
#24779 = ADVANCED_FACE ( 'NONE', ( #40069 ), #16580, .T. ) ;
#24780 = AXIS2_PLACEMENT_3D ( 'NONE', #35143, #42988, #16554 ) ;
#24781 = FACE_OUTER_BOUND ( 'NONE', #32191, .T. ) ;
#24782 = CARTESIAN_POINT ( 'NONE',  ( -10.90093335751250692, 0.000000000000000000, 0.000000000000000000 ) ) ;
#24783 = ORIENTED_EDGE ( 'NONE', *, *, #13333, .T. ) ;
#24784 = FACE_OUTER_BOUND ( 'NONE', #46003, .T. ) ;
#24785 = ORIENTED_EDGE ( 'NONE', *, *, #9750, .F. ) ;
#24786 = ORIENTED_EDGE ( 'NONE', *, *, #37646, .T. ) ;
#24787 = DIRECTION ( 'NONE',  ( -1.000000000000000000, 0.000000000000000000, 0.000000000000000000 ) ) ;
#24788 = ORIENTED_EDGE ( 'NONE', *, *, #47620, .F. ) ;
#24789 = CARTESIAN_POINT ( 'NONE',  ( 10.00000000000000000, 0.000000000000000000, 0.000000000000000000 ) ) ;
#24790 = LINE ( 'NONE', #10588, #43829 ) ;
#24791 = DIRECTION ( 'NONE',  ( 0.000000000000000000, 0.000000000000000000, -1.000000000000000000 ) ) ;
#24792 = EDGE_LOOP ( 'NONE', ( #24415, #17095, #22175, #1600 ) ) ;
#24793 = DIRECTION ( 'NONE',  ( -0.9038112904824846527, 0.4279312458752990711, 0.000000000000000000 ) ) ;
#24794 = DIRECTION ( 'NONE',  ( 0.000000000000000000, -0.9945218953682730678, 0.1045284632676570929 ) ) ;
#24795 = CARTESIAN_POINT ( 'NONE',  ( 26.47460221209471598, -121.8961639463267090, -5.500000000000000000 ) ) ;
#24796 = CARTESIAN_POINT ( 'NONE',  ( 0.000000000000000000, -10.41901085202050581, -40.68715046381939970 ) ) ;
#24797 = FACE_OUTER_BOUND ( 'NONE', #34150, .T. ) ;
#24798 = CIRCLE ( 'NONE', #11560, 37.49900000000000233 ) ;
#24799 = CARTESIAN_POINT ( 'NONE',  ( 10.00000000000000000, -38.55633173627023069, 16.65560815589396526 ) ) ;
#24800 = CARTESIAN_POINT ( 'NONE',  ( 10.00000000000000000, 35.95386929396256903, -10.96151621346501237 ) ) ;
#24801 = DIRECTION ( 'NONE',  ( 0.000000000000000000, 0.000000000000000000, 1.000000000000000000 ) ) ;
#24802 = LINE ( 'NONE', #39744, #21599 ) ;
#24803 = AXIS2_PLACEMENT_3D ( 'NONE', #45263, #41843, #12232 ) ;
#24804 = LINE ( 'NONE', #43878, #25178 ) ;
#24805 = DIRECTION ( 'NONE',  ( 0.000000000000000000, 0.000000000000000000, -1.000000000000000000 ) ) ;
#24806 = ORIENTED_EDGE ( 'NONE', *, *, #32980, .T. ) ;
#24807 = CARTESIAN_POINT ( 'NONE',  ( -22.53294031248082163, -134.0273518838794757, 5.500000000000000000 ) ) ;
#24808 = AXIS2_PLACEMENT_3D ( 'NONE', #1393, #4352, #8483 ) ;
#24809 = ORIENTED_EDGE ( 'NONE', *, *, #39531, .T. ) ;
#24810 = CARTESIAN_POINT ( 'NONE',  ( 0.000000000000000000, 11.30684508768452368, -76.66974797899824523 ) ) ;
#24811 = ADVANCED_FACE ( 'NONE', ( #20746 ), #46932, .T. ) ;
#24812 = DIRECTION ( 'NONE',  ( 0.000000000000000000, 0.000000000000000000, 1.000000000000000000 ) ) ;
#24813 = EDGE_CURVE ( 'NONE', #10410, #9130, #8304, .T. ) ;
#24814 = ORIENTED_EDGE ( 'NONE', *, *, #8913, .F. ) ;
#24815 = DIRECTION ( 'NONE',  ( 0.000000000000000000, 0.000000000000000000, 1.000000000000000000 ) ) ;
#24816 = ORIENTED_EDGE ( 'NONE', *, *, #15324, .T. ) ;
#24817 = ORIENTED_EDGE ( 'NONE', *, *, #37337, .F. ) ;
#24818 = EDGE_CURVE ( 'NONE', #11933, #409, #39588, .T. ) ;
#24819 = EDGE_CURVE ( 'NONE', #31175, #1469, #15086, .T. ) ;
#24820 = CIRCLE ( 'NONE', #44358, 16.00000000000000000 ) ;
#24821 = FACE_OUTER_BOUND ( 'NONE', #3633, .T. ) ;
#24822 = ORIENTED_EDGE ( 'NONE', *, *, #8192, .T. ) ;
#24823 = EDGE_CURVE ( 'NONE', #23779, #34978, #43528, .T. ) ;
#24824 = LINE ( 'NONE', #32420, #29703 ) ;
#24825 = CARTESIAN_POINT ( 'NONE',  ( -2.499999999999997780, 8.494897427831771708, -10.00000000000000178 ) ) ;
#24826 = ORIENTED_EDGE ( 'NONE', *, *, #46431, .T. ) ;
#24827 = AXIS2_PLACEMENT_3D ( 'NONE', #10468, #47897, #10717 ) ;
#24828 = FACE_OUTER_BOUND ( 'NONE', #47693, .T. ) ;
#24829 = ORIENTED_EDGE ( 'NONE', *, *, #19761, .T. ) ;
#24830 = DIRECTION ( 'NONE',  ( -0.000000000000000000, 0.9510565162951539753, -0.3090169943749460635 ) ) ;
#24831 = CARTESIAN_POINT ( 'NONE',  ( 11.99999999999999822, 74.65491531819105830, 8.830959090343693418 ) ) ;
#24832 = DIRECTION ( 'NONE',  ( 0.000000000000000000, 0.000000000000000000, 1.000000000000000000 ) ) ;
#24833 = EDGE_CURVE ( 'NONE', #30139, #8790, #32576, .T. ) ;
#24834 = AXIS2_PLACEMENT_3D ( 'NONE', #46176, #4579, #22685 ) ;
#24835 = ORIENTED_EDGE ( 'NONE', *, *, #36676, .F. ) ;
#24836 = DIRECTION ( 'NONE',  ( 0.000000000000000000, 0.000000000000000000, 1.000000000000000000 ) ) ;
#24837 = ORIENTED_EDGE ( 'NONE', *, *, #39027, .F. ) ;
#24838 = CARTESIAN_POINT ( 'NONE',  ( -11.70000000000000107, 0.000000000000000000, 0.000000000000000000 ) ) ;
#24839 = PLANE ( 'NONE',  #47255 ) ;
#24840 = DIRECTION ( 'NONE',  ( -1.000000000000000000, 0.000000000000000000, 0.000000000000000000 ) ) ;
#24841 = DIRECTION ( 'NONE',  ( 0.000000000000000000, -0.9238795325112822976, -0.3826834323651008285 ) ) ;
#24842 = DIRECTION ( 'NONE',  ( -1.000000000000000000, -0.000000000000000000, 0.000000000000000000 ) ) ;
#24843 = CYLINDRICAL_SURFACE ( 'NONE', #33147, 37.49900000000000233 ) ;
#24844 = LINE ( 'NONE', #32200, #14099 ) ;
#24845 = CARTESIAN_POINT ( 'NONE',  ( 10.00000000000000000, 16.65560815589411092, 38.55633173627015964 ) ) ;
#24846 = AXIS2_PLACEMENT_3D ( 'NONE', #30495, #45417, #19697 ) ;
#24847 = CARTESIAN_POINT ( 'NONE',  ( -11.59999999999999787, 0.000000000000000000, -43.79999999999998295 ) ) ;
#24848 = LINE ( 'NONE', #44176, #12969 ) ;
#24849 = ORIENTED_EDGE ( 'NONE', *, *, #10328, .T. ) ;
#24850 = DIRECTION ( 'NONE',  ( 0.000000000000000000, 0.000000000000000000, 1.000000000000000000 ) ) ;
#24851 = FACE_OUTER_BOUND ( 'NONE', #2356, .T. ) ;
#24852 = FACE_OUTER_BOUND ( 'NONE', #25165, .T. ) ;
#24853 = CARTESIAN_POINT ( 'NONE',  ( -12.49999999999999645, 0.000000000000000000, 125.0000000000000000 ) ) ;
#24854 = AXIS2_PLACEMENT_3D ( 'NONE', #31362, #39421, #35247 ) ;
#24855 = FACE_OUTER_BOUND ( 'NONE', #24500, .T. ) ;
#24856 = CARTESIAN_POINT ( 'NONE',  ( 0.000000000000000000, -20.55727247249748046, 16.78983467731285018 ) ) ;
#24857 = EDGE_LOOP ( 'NONE', ( #48072, #31264, #12978, #47554 ) ) ;
#24858 = EDGE_CURVE ( 'NONE', #41796, #41833, #23991, .T. ) ;
#24859 = CARTESIAN_POINT ( 'NONE',  ( 10.00000000000000000, 55.38113227695782115, 54.21277698773695164 ) ) ;
#24861 = EDGE_CURVE ( 'NONE', #18, #26898, #6780, .T. ) ;
#24860 = CIRCLE ( 'NONE', #28778, 31.99999999999998934 ) ;
#24862 = EDGE_CURVE ( 'NONE', #31962, #33470, #13831, .T. ) ;
#24863 = AXIS2_PLACEMENT_3D ( 'NONE', #18969, #854, #22655 ) ;
#24864 = DIRECTION ( 'NONE',  ( 1.000000000000000000, 0.000000000000000000, 0.000000000000000000 ) ) ;
#24865 = ADVANCED_FACE ( 'NONE', ( #21933 ), #11430, .T. ) ;
#24866 = ORIENTED_EDGE ( 'NONE', *, *, #16677, .T. ) ;
#24867 = EDGE_LOOP ( 'NONE', ( #37897, #34942, #20921, #20464 ) ) ;
#24868 = EDGE_CURVE ( 'NONE', #35718, #37838, #41199, .T. ) ;
#24869 = EDGE_CURVE ( 'NONE', #27429, #9625, #29293, .T. ) ;
#24870 = PLANE ( 'NONE',  #12496 ) ;
#24871 = MECHANICAL_DESIGN_GEOMETRIC_PRESENTATION_REPRESENTATION (  '', ( #47547 ), #31952 ) ;
#24872 = ORIENTED_EDGE ( 'NONE', *, *, #15191, .T. ) ;
#24873 = AXIS2_PLACEMENT_3D ( 'NONE', #19372, #30410, #22814 ) ;
#24874 = ORIENTED_EDGE ( 'NONE', *, *, #23833, .T. ) ;
#24875 = EDGE_CURVE ( 'NONE', #4907, #13485, #26345, .T. ) ;
#24876 = DIRECTION ( 'NONE',  ( 0.000000000000000000, 0.000000000000000000, 1.000000000000000000 ) ) ;
#24877 = CARTESIAN_POINT ( 'NONE',  ( 5.999999999999999112, 33.71516098798741012, 74.74816331893441657 ) ) ;
#24878 = EDGE_LOOP ( 'NONE', ( #40084, #6371, #28680, #2070 ) ) ;
#24879 = ORIENTED_EDGE ( 'NONE', *, *, #15541, .T. ) ;
#24880 = ORIENTED_EDGE ( 'NONE', *, *, #10310, .F. ) ;
#24881 = FACE_OUTER_BOUND ( 'NONE', #23816, .T. ) ;
#24882 = CARTESIAN_POINT ( 'NONE',  ( 5.999999999999999112, -71.21200624218768382, -40.65526001592688488 ) ) ;
#24883 = EDGE_CURVE ( 'NONE', #39350, #12661, #15403, .T. ) ;
#24884 = CARTESIAN_POINT ( 'NONE',  ( 0.000000000000000000, -62.50884508063453637, 41.76106447765467777 ) ) ;
#24885 = VERTEX_POINT ( 'NONE', #22662 ) ;
#24886 = ORIENTED_EDGE ( 'NONE', *, *, #21215, .T. ) ;
#24887 = VERTEX_POINT ( 'NONE', #2855 ) ;
#24888 = CARTESIAN_POINT ( 'NONE',  ( 10.00000000000000000, 72.35432306680485226, -20.40083707022909110 ) ) ;
#24889 = ORIENTED_EDGE ( 'NONE', *, *, #13766, .T. ) ;
#24890 = CYLINDRICAL_SURFACE ( 'NONE', #5442, 31.99999999999998579 ) ;
#24891 = DIRECTION ( 'NONE',  ( -1.000000000000000000, 0.000000000000000000, 0.000000000000000000 ) ) ;
#24892 = VECTOR ( 'NONE', #5340, 999.9999999999998863 ) ;
#24894 = CARTESIAN_POINT ( 'NONE',  ( 0.000000000000000000, -27.05870788708250885, 26.08949754953014022 ) ) ;
#24893 = VECTOR ( 'NONE', #32499, 1000.000000000000000 ) ;
#24895 = PLANE ( 'NONE',  #3422 ) ;
#24896 = DIRECTION ( 'NONE',  ( 0.000000000000000000, 0.8090169943749498938, 0.5877852522924696954 ) ) ;
#24897 = EDGE_CURVE ( 'NONE', #17292, #38735, #10444, .T. ) ;
#24898 = AXIS2_PLACEMENT_3D ( 'NONE', #33905, #4784, #1595 ) ;
#24899 = CARTESIAN_POINT ( 'NONE',  ( 0.000000000000000000, -9.188173127307001309, -40.98264845739759465 ) ) ;
#24900 = ADVANCED_FACE ( 'NONE', ( #11172 ), #3328, .T. ) ;
#24901 = LINE ( 'NONE', #20758, #47798 ) ;
#24902 = ORIENTED_EDGE ( 'NONE', *, *, #11602, .F. ) ;
#24903 = DIRECTION ( 'NONE',  ( 0.000000000000000000, 0.000000000000000000, 1.000000000000000000 ) ) ;
#24904 = ORIENTED_EDGE ( 'NONE', *, *, #22345, .F. ) ;
#24905 = DIRECTION ( 'NONE',  ( -1.000000000000000000, 0.000000000000000000, 0.000000000000000000 ) ) ;
#24906 = LINE ( 'NONE', #28336, #20044 ) ;
#24907 = CARTESIAN_POINT ( 'NONE',  ( 10.00000000000000000, 5.202137450156389953, 37.22597642581160216 ) ) ;
#24908 = ORIENTED_EDGE ( 'NONE', *, *, #36844, .F. ) ;
#24909 = CARTESIAN_POINT ( 'NONE',  ( 18.80329974962065265, -105.8248132807389084, -5.500000000000000000 ) ) ;
#24910 = ORIENTED_EDGE ( 'NONE', *, *, #2, .T. ) ;
#24911 = CARTESIAN_POINT ( 'NONE',  ( 10.00000000000000000, 0.000000000000000000, 0.000000000000000000 ) ) ;
#24912 = VECTOR ( 'NONE', #7878, 1000.000000000000000 ) ;
#24913 = DIRECTION ( 'NONE',  ( -1.000000000000000000, -0.000000000000000000, 0.000000000000000000 ) ) ;
#24914 = ADVANCED_FACE ( 'NONE', ( #33201 ), #41045, .T. ) ;
#24915 = ORIENTED_EDGE ( 'NONE', *, *, #32539, .F. ) ;
#24916 = CARTESIAN_POINT ( 'NONE',  ( -0.8815729230226007074, -93.47222532549339746, -2.500000000000000000 ) ) ;
#24917 = CARTESIAN_POINT ( 'NONE',  ( 10.00000000000000000, 59.75363087400074846, 56.15606465354979804 ) ) ;
#24918 = DIRECTION ( 'NONE',  ( 0.000000000000000000, 0.000000000000000000, 1.000000000000000000 ) ) ;
#24919 = EDGE_CURVE ( 'NONE', #31513, #46010, #40325, .T. ) ;
#24920 = CYLINDRICAL_SURFACE ( 'NONE', #37772, 31.99999999999999289 ) ;
#24921 = EDGE_CURVE ( 'NONE', #19610, #22767, #22183, .T. ) ;
#24922 = SHAPE_REPRESENTATION_RELATIONSHIP ( 'NONE' , 'NONE' ,  #22809, #26873 ) ;
#24923 = VERTEX_POINT ( 'NONE', #44945 ) ;
#24924 = ORIENTED_EDGE ( 'NONE', *, *, #6963, .F. ) ;
#24925 = CIRCLE ( 'NONE', #44492, 32.00000000000000000 ) ;
#24926 = ADVANCED_FACE ( 'NONE', ( #12154 ), #15561, .T. ) ;
#24927 = EDGE_LOOP ( 'NONE', ( #5590, #10519, #15534, #26382 ) ) ;
#24928 = AXIS2_PLACEMENT_3D ( 'NONE', #36179, #3366, #6335 ) ;
#24929 = CIRCLE ( 'NONE', #48370, 82.00000000000000000 ) ;
#24930 = DIRECTION ( 'NONE',  ( -1.000000000000000000, -0.000000000000000000, -0.000000000000000000 ) ) ;
#24931 = DIRECTION ( 'NONE',  ( -1.000000000000000000, 0.000000000000000000, 0.000000000000000000 ) ) ;
#24932 = CIRCLE ( 'NONE', #23357, 32.00000000000000000 ) ;
#24933 = ORIENTED_EDGE ( 'NONE', *, *, #27813, .T. ) ;
#24934 = CARTESIAN_POINT ( 'NONE',  ( -25.50183398199384754, -112.6408924756582053, 2.500000000000000000 ) ) ;
#24935 = ORIENTED_EDGE ( 'NONE', *, *, #37677, .F. ) ;
#24936 = ORIENTED_EDGE ( 'NONE', *, *, #25621, .F. ) ;
#24937 = ORIENTED_EDGE ( 'NONE', *, *, #43111, .F. ) ;
#24938 = CARTESIAN_POINT ( 'NONE',  ( 0.000000000000000000, 10.30890764327382847, 81.34940948281339956 ) ) ;
#24939 = ORIENTED_EDGE ( 'NONE', *, *, #22398, .T. ) ;
#24940 = LINE ( 'NONE', #36443, #37966 ) ;
#24941 = VERTEX_POINT ( 'NONE', #27548 ) ;
#24942 = LINE ( 'NONE', #6355, #4089 ) ;
#24943 = DIRECTION ( 'NONE',  ( 0.000000000000000000, 0.000000000000000000, 1.000000000000000000 ) ) ;
#24944 = LINE ( 'NONE', #18324, #35336 ) ;
#24945 = EDGE_LOOP ( 'NONE', ( #11114, #10802, #16834, #27485 ) ) ;
#24946 = CARTESIAN_POINT ( 'NONE',  ( 10.00000000000000000, -31.46837873495025306, 68.27212725128265447 ) ) ;
#24947 = ORIENTED_EDGE ( 'NONE', *, *, #2230, .T. ) ;
#24948 = DIRECTION ( 'NONE',  ( 0.000000000000000000, -0.2334453638558922628, -0.9723699203976798877 ) ) ;
#24949 = CIRCLE ( 'NONE', #37464, 31.99999999999998934 ) ;
#24950 = DIRECTION ( 'NONE',  ( -1.000000000000000000, 0.000000000000000000, 0.000000000000000000 ) ) ;
#24951 = ORIENTED_EDGE ( 'NONE', *, *, #43851, .T. ) ;
#24952 = ORIENTED_EDGE ( 'NONE', *, *, #18669, .T. ) ;
#24953 = LINE ( 'NONE', #39898, #46344 ) ;
#24954 = LINE ( 'NONE', #31608, #44925 ) ;
#24955 = VERTEX_POINT ( 'NONE', #42476 ) ;
#24956 = ORIENTED_EDGE ( 'NONE', *, *, #19029, .F. ) ;
#24957 = CIRCLE ( 'NONE', #47624, 31.99999999999999289 ) ;
#24958 = DIRECTION ( 'NONE',  ( 0.000000000000000000, 0.000000000000000000, 1.000000000000000000 ) ) ;
#24959 = CARTESIAN_POINT ( 'NONE',  ( 0.000000000000000000, -120.0000000000000000, -2.500000000000000000 ) ) ;
#24960 = CARTESIAN_POINT ( 'NONE',  ( 0.000000000000000000, -55.19960302592029677, -51.03279382321147750 ) ) ;
#24961 = CARTESIAN_POINT ( 'NONE',  ( 0.000000000000000000, 70.52718814184294160, -26.02418014898236720 ) ) ;
#24962 = DIRECTION ( 'NONE',  ( -1.000000000000000000, -0.000000000000000000, -0.000000000000000000 ) ) ;
#24963 = CARTESIAN_POINT ( 'NONE',  ( 0.000000000000000000, 37.22597642581158084, -5.202137450156524068 ) ) ;
#24964 = AXIS2_PLACEMENT_3D ( 'NONE', #28697, #20365, #20138 ) ;
#24965 = CARTESIAN_POINT ( 'NONE',  ( 11.99999999999999822, -50.23322058963393744, 64.81221759200325039 ) ) ;
#24966 = CARTESIAN_POINT ( 'NONE',  ( -10.00000000000000000, 0.000000000000000000, 0.000000000000000000 ) ) ;
#24967 = CARTESIAN_POINT ( 'NONE',  ( -3.000000000000000000, -25.60904388321925396, 6.976881207771172377 ) ) ;
#24968 = CARTESIAN_POINT ( 'NONE',  ( 10.00000000000000000, 36.88895765772642932, -6.736453364083163642 ) ) ;
#24969 = ADVANCED_FACE ( 'NONE', ( #23621 ), #12383, .F. ) ;
#24970 = CYLINDRICAL_SURFACE ( 'NONE', #31213, 16.00000000000000000 ) ;
#24971 = CARTESIAN_POINT ( 'NONE',  ( -3.000000000000000000, 26.50000000000000000, -1.500000000000001332 ) ) ;
#24972 = ORIENTED_EDGE ( 'NONE', *, *, #20654, .F. ) ;
#24973 = EDGE_CURVE ( 'NONE', #3577, #6962, #41757, .T. ) ;
#24974 = ORIENTED_EDGE ( 'NONE', *, *, #37364, .T. ) ;
#24975 = DIRECTION ( 'NONE',  ( 0.000000000000000000, 0.7431448254773862505, -0.6691306063588671194 ) ) ;
#24976 = ADVANCED_FACE ( 'NONE', ( #42003 ), #45663, .T. ) ;
#24977 = CONTEXT_DEPENDENT_SHAPE_REPRESENTATION ( #27584, #18311 ) ;
#24978 = EDGE_CURVE ( 'NONE', #7678, #19681, #19296, .T. ) ;
#24979 = CARTESIAN_POINT ( 'NONE',  ( 0.000000000000000000, -74.65374052328654386, 8.840884882374837161 ) ) ;
#24980 = VERTEX_POINT ( 'NONE', #19692 ) ;
#24981 = ORIENTED_EDGE ( 'NONE', *, *, #4390, .F. ) ;
#24982 = VECTOR ( 'NONE', #21769, 1000.000000000000000 ) ;
#24983 = VECTOR ( 'NONE', #38075, 1000.000000000000000 ) ;
#24984 = DIRECTION ( 'NONE',  ( 0.6516173805718058487, -0.7585478161175724932, 0.000000000000000000 ) ) ;
#24985 = ORIENTED_EDGE ( 'NONE', *, *, #36454, .F. ) ;
#24986 = DIRECTION ( 'NONE',  ( 0.000000000000000000, 0.000000000000000000, 1.000000000000000000 ) ) ;
#24987 = CIRCLE ( 'NONE', #10146, 82.00000000000000000 ) ;
#24988 = EDGE_LOOP ( 'NONE', ( #36233, #41142, #14675, #11644 ) ) ;
#24989 = CARTESIAN_POINT ( 'NONE',  ( 10.00000000000000000, 20.40083707022987625, -72.35432306680462489 ) ) ;
#24990 = VERTEX_POINT ( 'NONE', #19454 ) ;
#24991 = CARTESIAN_POINT ( 'NONE',  ( 0.000000000000000000, 59.75363087400076267, 56.15606465354979093 ) ) ;
#24992 = CIRCLE ( 'NONE', #35939, 77.49899999999999523 ) ;
#24993 = DIRECTION ( 'NONE',  ( 0.000000000000000000, 0.000000000000000000, 1.000000000000000000 ) ) ;
#24994 = ORIENTED_EDGE ( 'NONE', *, *, #9337, .F. ) ;
#24995 = LINE ( 'NONE', #18121, #16071 ) ;
#24996 = ORIENTED_EDGE ( 'NONE', *, *, #2107, .F. ) ;
#24997 = EDGE_LOOP ( 'NONE', ( #23656, #23793, #10655, #39900 ) ) ;
#24998 = DIRECTION ( 'NONE',  ( 0.000000000000000000, 0.8526401643540897357, 0.5224985647159527957 ) ) ;
#24999 = DIRECTION ( 'NONE',  ( 0.000000000000000000, -0.4067366430757897722, -0.9135454576426056406 ) ) ;
#25000 = CARTESIAN_POINT ( 'NONE',  ( 11.99999999999999822, -66.50666863322028632, 39.78640506895582973 ) ) ;
#25002 = ORIENTED_EDGE ( 'NONE', *, *, #37446, .T. ) ;
#25001 = CARTESIAN_POINT ( 'NONE',  ( 11.99999999999999822, -49.70050353004932475, 59.46389618801947563 ) ) ;
#25003 = EDGE_CURVE ( 'NONE', #17728, #42769, #36486, .T. ) ;
#25004 = CARTESIAN_POINT ( 'NONE',  ( 6.377742925735834234, -145.7647898336708181, 5.500000000000000000 ) ) ;
#25005 = ORIENTED_EDGE ( 'NONE', *, *, #21419, .T. ) ;
#25006 = DIRECTION ( 'NONE',  ( 1.000000000000000000, -0.000000000000000000, -0.000000000000000000 ) ) ;
#25007 = ORIENTED_EDGE ( 'NONE', *, *, #2072, .F. ) ;
#25008 = ORIENTED_EDGE ( 'NONE', *, *, #44123, .T. ) ;
#25009 = CARTESIAN_POINT ( 'NONE',  ( 0.000000000000000000, -3.894527615417333610, -81.90746397400393164 ) ) ;
#25010 = LINE ( 'NONE', #24296, #2778 ) ;
#25011 = VERTEX_POINT ( 'NONE', #34384 ) ;
#25012 = EDGE_CURVE ( 'NONE', #16167, #8908, #548, .T. ) ;
#25013 = CYLINDRICAL_SURFACE ( 'NONE', #28560, 77.49899999999999523 ) ;
#25014 = DIRECTION ( 'NONE',  ( -1.000000000000000000, -0.000000000000000000, 0.000000000000000000 ) ) ;
#25015 = CARTESIAN_POINT ( 'NONE',  ( 0.000000000000000000, 0.000000000000000000, 0.000000000000000000 ) ) ;
#25016 = ORIENTED_EDGE ( 'NONE', *, *, #2373, .T. ) ;
#25017 = CARTESIAN_POINT ( 'NONE',  ( 0.000000000000000000, 10.30890764327382136, 81.34940948281339956 ) ) ;
#25018 = EDGE_CURVE ( 'NONE', #41574, #15936, #33910, .T. ) ;
#25019 = DIRECTION ( 'NONE',  ( 0.000000000000000000, -0.9876883405951394357, 0.1564344650402205716 ) ) ;
#25020 = CARTESIAN_POINT ( 'NONE',  ( -5.250000000000000888, -13.95926121303099343, -1.199999999999999956 ) ) ;
#25021 = DIRECTION ( 'NONE',  ( 1.000000000000000000, 0.000000000000000000, -0.000000000000000000 ) ) ;
#25022 = ORIENTED_EDGE ( 'NONE', *, *, #32028, .F. ) ;
#25023 = CIRCLE ( 'NONE', #31268, 16.00000000000000000 ) ;
#25024 = CARTESIAN_POINT ( 'NONE',  ( 10.00000000000000000, -8.830959090342926032, 74.65491531819115778 ) ) ;
#25025 = DIRECTION ( 'NONE',  ( -1.000000000000000000, 0.000000000000000000, 0.000000000000000000 ) ) ;
#25026 = DIRECTION ( 'NONE',  ( -1.000000000000000000, 0.000000000000000000, 0.000000000000000000 ) ) ;
#25027 = LINE ( 'NONE', #21354, #36437 ) ;
#25028 = CIRCLE ( 'NONE', #9377, 31.99999999999998934 ) ;
#25029 = CARTESIAN_POINT ( 'NONE',  ( 12.00000000000000000, 5.835314593368777558, 22.81335362449846471 ) ) ;
#25030 = DIRECTION ( 'NONE',  ( 0.000000000000000000, 0.000000000000000000, 1.000000000000000000 ) ) ;
#25031 = AXIS2_PLACEMENT_3D ( 'NONE', #40023, #14069, #47115 ) ;
#25032 = EDGE_CURVE ( 'NONE', #11145, #1183, #4470, .T. ) ;
#25033 = VERTEX_POINT ( 'NONE', #30268 ) ;
#25034 = ADVANCED_FACE ( 'NONE', ( #8456 ), #30742, .F. ) ;
#25035 = AXIS2_PLACEMENT_3D ( 'NONE', #10148, #43459, #3038 ) ;
#25036 = ORIENTED_EDGE ( 'NONE', *, *, #45031, .F. ) ;
#25037 = FACE_OUTER_BOUND ( 'NONE', #21439, .T. ) ;
#25038 = CIRCLE ( 'NONE', #2351, 82.00000000000000000 ) ;
#25039 = ORIENTED_EDGE ( 'NONE', *, *, #25846, .T. ) ;
#25040 = DIRECTION ( 'NONE',  ( -1.000000000000000000, 0.000000000000000000, 0.000000000000000000 ) ) ;
#25041 = DIRECTION ( 'NONE',  ( -1.000000000000000000, 0.000000000000000000, -0.000000000000000000 ) ) ;
#25042 = ORIENTED_EDGE ( 'NONE', *, *, #18947, .F. ) ;
#25043 = EDGE_CURVE ( 'NONE', #34450, #28702, #30997, .T. ) ;
#25044 = FACE_OUTER_BOUND ( 'NONE', #25326, .T. ) ;
#25045 = ORIENTED_EDGE ( 'NONE', *, *, #47249, .T. ) ;
#25046 = CIRCLE ( 'NONE', #13361, 82.00000000000000000 ) ;
#25047 = FACE_OUTER_BOUND ( 'NONE', #44557, .T. ) ;
#25048 = CIRCLE ( 'NONE', #23479, 77.49899999999999523 ) ;
#25049 = FACE_OUTER_BOUND ( 'NONE', #16697, .T. ) ;
#25050 = CARTESIAN_POINT ( 'NONE',  ( 0.000000000000000000, 0.000000000000000000, 0.000000000000000000 ) ) ;
#25051 = CIRCLE ( 'NONE', #12566, 16.00000000000000000 ) ;
#25052 = AXIS2_PLACEMENT_3D ( 'NONE', #25705, #29142, #21076 ) ;
#25053 = EDGE_LOOP ( 'NONE', ( #44305, #7836, #36584, #19604 ) ) ;
#25054 = LINE ( 'NONE', #18184, #17621 ) ;
#25055 = VERTEX_POINT ( 'NONE', #45916 ) ;
#25056 = CIRCLE ( 'NONE', #28218, 31.99999999999999289 ) ;
#25057 = CARTESIAN_POINT ( 'NONE',  ( 0.000000000000000000, -12.93880638057369659, 76.41127070299266677 ) ) ;
#25058 = FACE_OUTER_BOUND ( 'NONE', #21928, .T. ) ;
#25059 = EDGE_CURVE ( 'NONE', #32991, #17592, #21644, .T. ) ;
#25060 = AXIS2_PLACEMENT_3D ( 'NONE', #8106, #3467, #45080 ) ;
#25061 = DIRECTION ( 'NONE',  ( -1.000000000000000000, 0.000000000000000000, 0.000000000000000000 ) ) ;
#25062 = EDGE_CURVE ( 'NONE', #36250, #42347, #28673, .T. ) ;
#25063 = ORIENTED_EDGE ( 'NONE', *, *, #27496, .T. ) ;
#25064 = STYLED_ITEM ( 'NONE', ( #201 ), #19105 ) ;
#25065 = CARTESIAN_POINT ( 'NONE',  ( 0.000000000000000000, 0.8261519478441983200, -77.49459641780885022 ) ) ;
#25066 = ORIENTED_EDGE ( 'NONE', *, *, #41830, .F. ) ;
#25067 = ORIENTED_EDGE ( 'NONE', *, *, #5543, .F. ) ;
#25068 = APPLICATION_CONTEXT ( 'automotive_design' ) ;
#25069 = CARTESIAN_POINT ( 'NONE',  ( 10.00000000000000000, 29.81001611431009479, 22.74946021919143391 ) ) ;
#25070 = EDGE_CURVE ( 'NONE', #12381, #36640, #45188, .T. ) ;
#25071 = DIRECTION ( 'NONE',  ( -1.000000000000000000, 0.000000000000000000, 0.000000000000000000 ) ) ;
#25072 = DIRECTION ( 'NONE',  ( -1.000000000000000000, -0.000000000000000000, 0.000000000000000000 ) ) ;
#25073 = DIRECTION ( 'NONE',  ( -1.000000000000000000, 0.000000000000000000, 0.000000000000000000 ) ) ;
#25074 = LINE ( 'NONE', #31967, #35467 ) ;
#25075 = EDGE_CURVE ( 'NONE', #15919, #10316, #1366, .T. ) ;
#25076 = CYLINDRICAL_SURFACE ( 'NONE', #7246, 37.49900000000000233 ) ;
#25077 = CARTESIAN_POINT ( 'NONE',  ( -9.937067298023309903, 7.583184918921312523, 52.00000000000002132 ) ) ;
#25078 = DIRECTION ( 'NONE',  ( -1.000000000000000000, 0.000000000000000000, 0.000000000000000000 ) ) ;
#25079 = CARTESIAN_POINT ( 'NONE',  ( -23.30023580412278505, -123.4057321492263384, 5.500000000000000000 ) ) ;
#25080 = CARTESIAN_POINT ( 'NONE',  ( 10.00000000000000000, -37.01155633439053361, -6.555932627142825986 ) ) ;
#25081 = VERTEX_POINT ( 'NONE', #11652 ) ;
#25082 = EDGE_LOOP ( 'NONE', ( #7961, #1811, #27255, #22649, #1394, #31202 ) ) ;
#25083 = DIRECTION ( 'NONE',  ( 0.000000000000000000, 0.000000000000000000, -1.000000000000000000 ) ) ;
#25084 = CARTESIAN_POINT ( 'NONE',  ( 10.00000000000000000, 16.23288003029497162, 33.80338159004289622 ) ) ;
#25085 = DIRECTION ( 'NONE',  ( 0.000000000000000000, 0.000000000000000000, 1.000000000000000000 ) ) ;
#25086 = EDGE_CURVE ( 'NONE', #2861, #5309, #10681, .T. ) ;
#25087 = EDGE_CURVE ( 'NONE', #1468, #7735, #23183, .T. ) ;
#25088 = CARTESIAN_POINT ( 'NONE',  ( 0.000000000000000000, 0.000000000000000000, 0.000000000000000000 ) ) ;
#25089 = VECTOR ( 'NONE', #18643, 1000.000000000000227 ) ;
#25090 = CARTESIAN_POINT ( 'NONE',  ( -3.000000000000002665, 0.000000000000000000, 0.000000000000000000 ) ) ;
#25091 = CARTESIAN_POINT ( 'NONE',  ( 0.000000000000000000, 0.000000000000000000, 0.000000000000000000 ) ) ;
#25092 = VECTOR ( 'NONE', #18255, 1000.000000000000000 ) ;
#25093 = ORIENTED_EDGE ( 'NONE', *, *, #46732, .T. ) ;
#25094 = CARTESIAN_POINT ( 'NONE',  ( 0.000000000000000000, 0.000000000000000000, 0.000000000000000000 ) ) ;
#25095 = CIRCLE ( 'NONE', #1659, 42.00000000000000000 ) ;
#25096 = VECTOR ( 'NONE', #46021, 1000.000000000000000 ) ;
#25097 = CARTESIAN_POINT ( 'NONE',  ( 0.000000000000000000, 40.65526001592713357, -71.21200624218752750 ) ) ;
#25098 = CIRCLE ( 'NONE', #31387, 82.00000000000000000 ) ;
#25099 = VERTEX_POINT ( 'NONE', #1602 ) ;
#25100 = ORIENTED_EDGE ( 'NONE', *, *, #45463, .T. ) ;
#25101 = AXIS2_PLACEMENT_3D ( 'NONE', #39176, #24014, #27205 ) ;
#25102 = EDGE_CURVE ( 'NONE', #33083, #23423, #42964, .T. ) ;
#25103 = VECTOR ( 'NONE', #45425, 1000.000000000000000 ) ;
#25104 = ORIENTED_EDGE ( 'NONE', *, *, #25155, .T. ) ;
#25105 = DIRECTION ( 'NONE',  ( 0.9781476007338070211, 2.546183866652749098E-17, 0.2079116908177526257 ) ) ;
#25106 = VERTEX_POINT ( 'NONE', #46878 ) ;
#25107 = ORIENTED_EDGE ( 'NONE', *, *, #3171, .T. ) ;
#25108 = FACE_OUTER_BOUND ( 'NONE', #19607, .T. ) ;
#25109 = CARTESIAN_POINT ( 'NONE',  ( 10.00000000000000000, -46.21855187248673502, 62.20884554314003623 ) ) ;
#25110 = VERTEX_POINT ( 'NONE', #47106 ) ;
#25111 = CARTESIAN_POINT ( 'NONE',  ( 10.00000000000000000, 24.73286445877703699, 73.44644590900070114 ) ) ;
#25112 = ORIENTED_EDGE ( 'NONE', *, *, #16008, .T. ) ;
#25113 = DIRECTION ( 'NONE',  ( -1.000000000000000000, 0.000000000000000000, 0.000000000000000000 ) ) ;
#25114 = CARTESIAN_POINT ( 'NONE',  ( 0.000000000000000000, 20.40083707022882820, 72.35432306680490910 ) ) ;
#25115 = VECTOR ( 'NONE', #9202, 1000.000000000000000 ) ;
#25116 = DIRECTION ( 'NONE',  ( -1.000000000000000000, 0.000000000000000000, 0.000000000000000000 ) ) ;
#25118 = ORIENTED_EDGE ( 'NONE', *, *, #33797, .F. ) ;
#25117 = VECTOR ( 'NONE', #28034, 1000.000000000000000 ) ;
#25119 = ORIENTED_EDGE ( 'NONE', *, *, #47448, .F. ) ;
#25120 = FACE_OUTER_BOUND ( 'NONE', #9403, .T. ) ;
#25121 = EDGE_LOOP ( 'NONE', ( #48199, #20144, #46008, #43271 ) ) ;
#25122 = CIRCLE ( 'NONE', #27487, 82.00000000000000000 ) ;
#25123 = AXIS2_PLACEMENT_3D ( 'NONE', #39830, #24400, #28318 ) ;
#25124 = CARTESIAN_POINT ( 'NONE',  ( 0.000000000000000000, 0.000000000000000000, -44.99999999999998579 ) ) ;
#25125 = EDGE_CURVE ( 'NONE', #40697, #36269, #38822, .T. ) ;
#25126 = CARTESIAN_POINT ( 'NONE',  ( 0.000000000000000000, 2.663952781846728790, -41.91543099594814947 ) ) ;
#25127 = CARTESIAN_POINT ( 'NONE',  ( 15.00000000000000000, -23.29833615347109088, -3.418703333116486665 ) ) ;
#25128 = CARTESIAN_POINT ( 'NONE',  ( -3.000000000000000000, 14.60985201121729737, -18.46759930825687945 ) ) ;
#25129 = ADVANCED_FACE ( 'NONE', ( #17479 ), #9415, .T. ) ;
#25130 = EDGE_CURVE ( 'NONE', #30369, #40486, #14598, .T. ) ;
#25131 = VECTOR ( 'NONE', #37608, 1000.000000000000000 ) ;
#25132 = DIRECTION ( 'NONE',  ( 1.000000000000000000, 0.000000000000000000, 0.000000000000000000 ) ) ;
#25133 = ADVANCED_FACE ( 'NONE', ( #6242 ), #27804, .T. ) ;
#25134 = LINE ( 'NONE', #17550, #41563 ) ;
#25135 = ORIENTED_EDGE ( 'NONE', *, *, #39034, .F. ) ;
#25136 = EDGE_CURVE ( 'NONE', #42577, #3648, #27113, .T. ) ;
#25137 = DIRECTION ( 'NONE',  ( 0.000000000000000000, -0.5224985647159559043, 0.8526401643540879594 ) ) ;
#25138 = ORIENTED_EDGE ( 'NONE', *, *, #15379, .F. ) ;
#25139 = AXIS2_PLACEMENT_3D ( 'NONE', #44085, #29407, #14225 ) ;
#25140 = CARTESIAN_POINT ( 'NONE',  ( 10.00000000000000000, -75.11764819372145041, -2.946379043147127064 ) ) ;
#25141 = CARTESIAN_POINT ( 'NONE',  ( 0.000000000000000000, 64.81221759200417409, -50.23322058963276504 ) ) ;
#25142 = DIRECTION ( 'NONE',  ( 0.000000000000000000, 0.000000000000000000, 1.000000000000000000 ) ) ;
#25143 = ADVANCED_FACE ( 'NONE', ( #24347, #31728 ), #31472, .F. ) ;
#25144 = CYLINDRICAL_SURFACE ( 'NONE', #11475, 37.49900000000000233 ) ;
#25145 = LINE ( 'NONE', #40090, #27960 ) ;
#25146 = VERTEX_POINT ( 'NONE', #20681 ) ;
#25147 = DIRECTION ( 'NONE',  ( 0.000000000000000000, -0.3090169943749349057, -0.9510565162951576390 ) ) ;
#25148 = CARTESIAN_POINT ( 'NONE',  ( 0.000000000000000000, -41.76937507738831812, 62.50329211542423025 ) ) ;
#25149 = CARTESIAN_POINT ( 'NONE',  ( 11.99999999999999822, 71.91182617369190666, 28.89263327155770966 ) ) ;
#25150 = EDGE_CURVE ( 'NONE', #25783, #25211, #34954, .T. ) ;
#25151 = DIRECTION ( 'NONE',  ( -1.000000000000000000, 0.000000000000000000, 0.000000000000000000 ) ) ;
#25152 = ORIENTED_EDGE ( 'NONE', *, *, #38970, .T. ) ;
#25153 = ORIENTED_EDGE ( 'NONE', *, *, #21438, .T. ) ;
#25154 = VECTOR ( 'NONE', #40032, 1000.000000000000000 ) ;
#25155 = EDGE_CURVE ( 'NONE', #16565, #1521, #1349, .T. ) ;
#25156 = CIRCLE ( 'NONE', #44696, 77.49899999999999523 ) ;
#25157 = DIRECTION ( 'NONE',  ( 0.000000000000000000, -0.5877852522924624790, -0.8090169943749551118 ) ) ;
#25158 = CARTESIAN_POINT ( 'NONE',  ( 0.000000000000000000, 26.79245525562762253, -32.34446384429942611 ) ) ;
#25159 = ORIENTED_EDGE ( 'NONE', *, *, #42558, .T. ) ;
#25160 = AXIS2_PLACEMENT_3D ( 'NONE', #31487, #35376, #17493 ) ;
#25161 = EDGE_CURVE ( 'NONE', #21975, #24320, #7598, .T. ) ;
#25162 = FACE_OUTER_BOUND ( 'NONE', #24056, .T. ) ;
#25163 = ORIENTED_EDGE ( 'NONE', *, *, #27600, .F. ) ;
#25164 = ORIENTED_EDGE ( 'NONE', *, *, #32978, .T. ) ;
#25165 = EDGE_LOOP ( 'NONE', ( #13275, #28736, #14300, #8485 ) ) ;
#25166 = DIRECTION ( 'NONE',  ( -0.000000000000000000, 0.000000000000000000, 1.000000000000000000 ) ) ;
#25167 = ORIENTED_EDGE ( 'NONE', *, *, #23403, .T. ) ;
#25168 = DIRECTION ( 'NONE',  ( -1.000000000000000000, 0.000000000000000000, 0.000000000000000000 ) ) ;
#25169 = VERTEX_POINT ( 'NONE', #32190 ) ;
#25170 = EDGE_CURVE ( 'NONE', #23354, #37827, #28715, .T. ) ;
#25171 = CARTESIAN_POINT ( 'NONE',  ( 5.000000000000002665, -2.543863470247813119, -81.96053171279905314 ) ) ;
#25172 = EDGE_CURVE ( 'NONE', #32258, #34421, #38072, .T. ) ;
#25173 = CARTESIAN_POINT ( 'NONE',  ( 11.99999999999999822, 0.000000000000000000, 0.000000000000000000 ) ) ;
#25174 = DIRECTION ( 'NONE',  ( 1.000000000000000000, -0.000000000000000000, -0.000000000000000000 ) ) ;
#25175 = ADVANCED_FACE ( 'NONE', ( #47362 ), #28517, .F. ) ;
#25176 = DIRECTION ( 'NONE',  ( 1.000000000000000000, 0.000000000000000000, 0.000000000000000000 ) ) ;
#25177 = ORIENTED_EDGE ( 'NONE', *, *, #17515, .T. ) ;
#25178 = VECTOR ( 'NONE', #17198, 1000.000000000000000 ) ;
#25179 = CARTESIAN_POINT ( 'NONE',  ( 0.000000000000000000, 0.000000000000000000, 0.000000000000000000 ) ) ;
#25180 = CYLINDRICAL_SURFACE ( 'NONE', #19602, 77.49899999999999523 ) ;
#25181 = ORIENTED_EDGE ( 'NONE', *, *, #3861, .F. ) ;
#25182 = ORIENTED_EDGE ( 'NONE', *, *, #471, .F. ) ;
#25183 = EDGE_CURVE ( 'NONE', #30137, #12997, #31961, .T. ) ;
#25184 = CARTESIAN_POINT ( 'NONE',  ( -10.00000000000000000, 0.000000000000000000, 0.000000000000000000 ) ) ;
#25185 = DIRECTION ( 'NONE',  ( 1.000000000000000000, 0.000000000000000000, 0.000000000000000000 ) ) ;
#25186 = ORIENTED_EDGE ( 'NONE', *, *, #32174, .T. ) ;
#25187 = AXIS2_PLACEMENT_3D ( 'NONE', #16178, #16646, #46031 ) ;
#25188 = ORIENTED_EDGE ( 'NONE', *, *, #45108, .F. ) ;
#25189 = DIRECTION ( 'NONE',  ( -0.7585478161175716050, -0.6516173805718067369, 0.000000000000000000 ) ) ;
#25190 = DIRECTION ( 'NONE',  ( 0.000000000000000000, 0.1564344650402311743, -0.9876883405951376593 ) ) ;
#25191 = CARTESIAN_POINT ( 'NONE',  ( 0.000000000000000000, -40.65526001592663619, 71.21200624218782593 ) ) ;
#25192 = LINE ( 'NONE', #10768, #2345 ) ;
#25193 = AXIS2_PLACEMENT_3D ( 'NONE', #33509, #7081, #11733 ) ;
#25194 = DIRECTION ( 'NONE',  ( 0.000000000000000000, 0.000000000000000000, 1.000000000000000000 ) ) ;
#25195 = DIRECTION ( 'NONE',  ( -1.000000000000000000, -0.000000000000000000, 0.000000000000000000 ) ) ;
#25196 = FACE_OUTER_BOUND ( 'NONE', #30797, .T. ) ;
#25197 = AXIS2_PLACEMENT_3D ( 'NONE', #32919, #17756, #36832 ) ;
#25198 = FACE_OUTER_BOUND ( 'NONE', #40903, .T. ) ;
#25199 = CARTESIAN_POINT ( 'NONE',  ( 0.000000000000000000, -49.70050353004932475, 59.46389618801944721 ) ) ;
#25200 = CARTESIAN_POINT ( 'NONE',  ( 0.000000000000000000, 39.04073710021366139, -15.48615015657542315 ) ) ;
#25201 = DIRECTION ( 'NONE',  ( -0.2306669878475648139, -0.9730327541852491491, 0.000000000000000000 ) ) ;
#25202 = ORIENTED_EDGE ( 'NONE', *, *, #14706, .T. ) ;
#25203 = ORIENTED_EDGE ( 'NONE', *, *, #20389, .F. ) ;
#25204 = CARTESIAN_POINT ( 'NONE',  ( 11.99999999999999822, -41.76106447765443619, -62.50884508063471401 ) ) ;
#25205 = AXIS2_PLACEMENT_3D ( 'NONE', #36687, #3152, #18080 ) ;
#25206 = LINE ( 'NONE', #43827, #44855 ) ;
#25207 = ORIENTED_EDGE ( 'NONE', *, *, #27163, .F. ) ;
#25208 = AXIS2_PLACEMENT_3D ( 'NONE', #21115, #32396, #36051 ) ;
#25209 = DIRECTION ( 'NONE',  ( -1.000000000000000000, -0.000000000000000000, -0.000000000000000000 ) ) ;
#25210 = VECTOR ( 'NONE', #1666, 1000.000000000000000 ) ;
#25211 = VERTEX_POINT ( 'NONE', #28264 ) ;
#25212 = CARTESIAN_POINT ( 'NONE',  ( 0.000000000000000000, -40.68715046381937128, 10.41901085202062660 ) ) ;
#25213 = VERTEX_POINT ( 'NONE', #43678 ) ;
#25214 = SURFACE_STYLE_FILL_AREA ( #6165 ) ;
#25215 = VECTOR ( 'NONE', #26604, 1000.000000000000000 ) ;
#25216 = EDGE_CURVE ( 'NONE', #28563, #9076, #44318, .T. ) ;
#25217 = ORIENTED_EDGE ( 'NONE', *, *, #9125, .F. ) ;
#25218 = CYLINDRICAL_SURFACE ( 'NONE', #24267, 31.99999999999998579 ) ;
#25219 = AXIS2_PLACEMENT_3D ( 'NONE', #815, #15757, #45610 ) ;
#25220 = CARTESIAN_POINT ( 'NONE',  ( 11.99999999999999822, 17.28742895386189460, -75.54627589209927407 ) ) ;
#25221 = VERTEX_POINT ( 'NONE', #48071 ) ;
#25222 = EDGE_CURVE ( 'NONE', #27986, #8792, #18195, .T. ) ;
#25223 = CARTESIAN_POINT ( 'NONE',  ( 15.00000000000000000, -13.04903810567646971, 19.60159698893442481 ) ) ;
#25224 = CIRCLE ( 'NONE', #42448, 11.59999999999999787 ) ;
#25225 = ORIENTED_EDGE ( 'NONE', *, *, #13544, .F. ) ;
#25226 = CYLINDRICAL_SURFACE ( 'NONE', #11363, 82.00000000000000000 ) ;
#25227 = VERTEX_POINT ( 'NONE', #44162 ) ;
#25228 = EDGE_CURVE ( 'NONE', #20542, #17607, #82, .T. ) ;
#25229 = CARTESIAN_POINT ( 'NONE',  ( -89.17737905728745318, -39.70432723693717492, -5.500000000000000000 ) ) ;
#25230 = CARTESIAN_POINT ( 'NONE',  ( 0.000000000000000000, -41.19522573413687638, -65.64334221924953283 ) ) ;
#25231 = LINE ( 'NONE', #40435, #20832 ) ;
#25233 = ORIENTED_EDGE ( 'NONE', *, *, #45048, .T. ) ;
#25232 = FACE_OUTER_BOUND ( 'NONE', #43491, .T. ) ;
#25234 = DIRECTION ( 'NONE',  ( 0.000000000000000000, 0.000000000000000000, 1.000000000000000000 ) ) ;
#25235 = ORIENTED_EDGE ( 'NONE', *, *, #8275, .T. ) ;
#25236 = CARTESIAN_POINT ( 'NONE',  ( -3.000000000000000000, 23.50000000000000000, -1.500000000000001332 ) ) ;
#25237 = ORIENTED_EDGE ( 'NONE', *, *, #10493, .T. ) ;
#25238 = ORIENTED_EDGE ( 'NONE', *, *, #31456, .F. ) ;
#25239 = ADVANCED_FACE ( 'NONE', ( #29230 ), #6475, .F. ) ;
#25240 = DIRECTION ( 'NONE',  ( 0.000000000000000000, 0.000000000000000000, 1.000000000000000000 ) ) ;
#25241 = CYLINDRICAL_SURFACE ( 'NONE', #37904, 31.99999999999999289 ) ;
#25242 = DIRECTION ( 'NONE',  ( 0.000000000000000000, 0.000000000000000000, -1.000000000000000000 ) ) ;
#25243 = EDGE_CURVE ( 'NONE', #9989, #28782, #36332, .T. ) ;
#25244 = CARTESIAN_POINT ( 'NONE',  ( 11.99999999999999822, -81.34940948281328588, -10.30890764327469356 ) ) ;
#25245 = DIRECTION ( 'NONE',  ( -0.7585478161175723821, -0.6516173805718057377, 0.000000000000000000 ) ) ;
#25246 = ORIENTED_EDGE ( 'NONE', *, *, #11785, .T. ) ;
#25247 = CIRCLE ( 'NONE', #4167, 77.49899999999999523 ) ;
#25248 = CARTESIAN_POINT ( 'NONE',  ( 0.000000000000000000, 77.32052557432841411, 5.256550761633138613 ) ) ;
#25249 = CARTESIAN_POINT ( 'NONE',  ( -10.00000000000000000, 0.000000000000000000, 0.000000000000000000 ) ) ;
#25250 = VECTOR ( 'NONE', #35985, 1000.000000000000000 ) ;
#25251 = CARTESIAN_POINT ( 'NONE',  ( 0.000000000000000000, -120.0000000000000000, 125.0000000000000000 ) ) ;
#25252 = ORIENTED_EDGE ( 'NONE', *, *, #35231, .T. ) ;
#25253 = CARTESIAN_POINT ( 'NONE',  ( 11.99999999999999822, 50.23322058963348979, 64.81221759200361987 ) ) ;
#25254 = LINE ( 'NONE', #14511, #42001 ) ;
#25255 = DIRECTION ( 'NONE',  ( -1.000000000000000000, 0.000000000000000000, -0.000000000000000000 ) ) ;
#25256 = VECTOR ( 'NONE', #10935, 1000.000000000000114 ) ;
#25257 = AXIS2_PLACEMENT_3D ( 'NONE', #2153, #39839, #43742 ) ;
#25258 = AXIS2_PLACEMENT_3D ( 'NONE', #33446, #45192, #45418 ) ;
#25259 = DIRECTION ( 'NONE',  ( 0.000000000000000000, 0.000000000000000000, 1.000000000000000000 ) ) ;
#25260 = CARTESIAN_POINT ( 'NONE',  ( 0.000000000000000000, 0.000000000000000000, 0.000000000000000000 ) ) ;
#25261 = DIRECTION ( 'NONE',  ( 0.000000000000000000, 0.000000000000000000, 1.000000000000000000 ) ) ;
#25262 = DIRECTION ( 'NONE',  ( 0.000000000000000000, -0.4539904997395352027, -0.8910065241883737830 ) ) ;
#25263 = AXIS2_PLACEMENT_3D ( 'NONE', #34180, #5300, #4808 ) ;
#25264 = VERTEX_POINT ( 'NONE', #18453 ) ;
#25266 = DIRECTION ( 'NONE',  ( -1.000000000000000000, -0.000000000000000000, 0.000000000000000000 ) ) ;
#25265 = CIRCLE ( 'NONE', #38684, 31.99999999999998934 ) ;
#25267 = CIRCLE ( 'NONE', #15920, 31.99999999999998934 ) ;
#25268 = ORIENTED_EDGE ( 'NONE', *, *, #21048, .T. ) ;
#25269 = AXIS2_PLACEMENT_3D ( 'NONE', #532, #45081, #755 ) ;
#25270 = DIRECTION ( 'NONE',  ( 0.000000000000000000, 0.000000000000000000, 1.000000000000000000 ) ) ;
#25271 = AXIS2_PLACEMENT_3D ( 'NONE', #39206, #43366, #46305 ) ;
#25272 = CARTESIAN_POINT ( 'NONE',  ( 11.99999999999999822, -8.830959090342926032, 74.65491531819115778 ) ) ;
#25273 = CIRCLE ( 'NONE', #21368, 15.99999999999999822 ) ;
#25274 = EDGE_LOOP ( 'NONE', ( #18792, #44988, #23441, #9161 ) ) ;
#25275 = EDGE_CURVE ( 'NONE', #2410, #46211, #10142, .T. ) ;
#25276 = ADVANCED_FACE ( 'NONE', ( #29472 ), #25547, .T. ) ;
#25277 = DIRECTION ( 'NONE',  ( 0.000000000000000000, 0.3826834323650904479, -0.9238795325112865164 ) ) ;
#25278 = VERTEX_POINT ( 'NONE', #40495 ) ;
#25279 = EDGE_CURVE ( 'NONE', #22205, #37953, #36525, .T. ) ;
#25280 = VERTEX_POINT ( 'NONE', #7444 ) ;
#25281 = CIRCLE ( 'NONE', #1040, 42.00000000000000000 ) ;
#25282 = CARTESIAN_POINT ( 'NONE',  ( 8.700667342345820288, -98.11853780484867116, 5.500000000000000000 ) ) ;
#25283 = ORIENTED_EDGE ( 'NONE', *, *, #33825, .F. ) ;
#25284 = DIRECTION ( 'NONE',  ( -1.000000000000000000, 0.000000000000000000, -0.000000000000000000 ) ) ;
#25285 = VECTOR ( 'NONE', #15516, 1000.000000000000227 ) ;
#25286 = CIRCLE ( 'NONE', #29988, 31.99999999999998579 ) ;
#25287 = DIRECTION ( 'NONE',  ( -1.000000000000000000, 0.000000000000000000, 0.000000000000000000 ) ) ;
#25288 = AXIS2_PLACEMENT_3D ( 'NONE', #18296, #14395, #37388 ) ;
#25289 = EDGE_LOOP ( 'NONE', ( #30865, #32819, #30851, #43147 ) ) ;
#25290 = DIRECTION ( 'NONE',  ( 0.000000000000000000, 0.000000000000000000, 1.000000000000000000 ) ) ;
#25291 = EDGE_CURVE ( 'NONE', #1684, #5172, #29469, .T. ) ;
#25292 = ORIENTED_EDGE ( 'NONE', *, *, #4041, .F. ) ;
#25293 = EDGE_CURVE ( 'NONE', #6451, #46491, #5266, .T. ) ;
#25294 = EDGE_CURVE ( 'NONE', #18715, #40885, #13087, .T. ) ;
#25295 = PLANE ( 'NONE',  #35832 ) ;
#25296 = CARTESIAN_POINT ( 'NONE',  ( 0.000000000000000000, -33.80338159004296017, 16.23288003029484727 ) ) ;
#25297 = DIRECTION ( 'NONE',  ( -1.000000000000000000, 0.000000000000000000, 0.000000000000000000 ) ) ;
#25298 = VECTOR ( 'NONE', #27966, 1000.000000000000000 ) ;
#25299 = VECTOR ( 'NONE', #17199, 1000.000000000000000 ) ;
#25300 = ORIENTED_EDGE ( 'NONE', *, *, #7529, .T. ) ;
#25301 = DIRECTION ( 'NONE',  ( -1.000000000000000000, 0.000000000000000000, 0.000000000000000000 ) ) ;
#25302 = VERTEX_POINT ( 'NONE', #17726 ) ;
#25303 = VERTEX_POINT ( 'NONE', #6720 ) ;
#25304 = CIRCLE ( 'NONE', #24564, 31.99999999999998579 ) ;
#25305 = DIRECTION ( 'NONE',  ( 0.000000000000000000, 0.9510565162951544194, -0.3090169943749446757 ) ) ;
#25306 = VECTOR ( 'NONE', #21562, 1000.000000000000114 ) ;
#25307 = DIRECTION ( 'NONE',  ( 0.000000000000000000, 0.000000000000000000, 1.000000000000000000 ) ) ;
#25308 = CARTESIAN_POINT ( 'NONE',  ( 10.00000000000000000, -17.67226234102801286, -33.17418723428327354 ) ) ;
#25309 = DIRECTION ( 'NONE',  ( 0.000000000000000000, 0.000000000000000000, 1.000000000000000000 ) ) ;
#25310 = ORIENTED_EDGE ( 'NONE', *, *, #21619, .F. ) ;
#25311 = DIRECTION ( 'NONE',  ( -1.000000000000000000, -0.000000000000000000, -0.000000000000000000 ) ) ;
#25312 = AXIS2_PLACEMENT_3D ( 'NONE', #29932, #23077, #45337 ) ;
#25313 = DIRECTION ( 'NONE',  ( -1.000000000000000000, 0.000000000000000000, 0.000000000000000000 ) ) ;
#25314 = CARTESIAN_POINT ( 'NONE',  ( -12.49999999999999645, 0.000000000000000000, 125.0000000000000000 ) ) ;
#25315 = LINE ( 'NONE', #18466, #32992 ) ;
#25316 = CARTESIAN_POINT ( 'NONE',  ( 0.000000000000000000, -21.32104025579135964, 30.84782396557210760 ) ) ;
#25317 = ORIENTED_EDGE ( 'NONE', *, *, #9765, .F. ) ;
#25318 = CYLINDRICAL_SURFACE ( 'NONE', #45121, 31.99999999999999289 ) ;
#25319 = CARTESIAN_POINT ( 'NONE',  ( 0.000000000000000000, -120.0000000000000000, 5.500000000000000000 ) ) ;
#25320 = DIRECTION ( 'NONE',  ( -1.000000000000000000, 0.000000000000000000, 0.000000000000000000 ) ) ;
#25321 = CARTESIAN_POINT ( 'NONE',  ( 11.99999999999999822, 75.11725578898467859, 2.956366410620910656 ) ) ;
#25322 = CIRCLE ( 'NONE', #41728, 31.99999999999999289 ) ;
#25323 = CIRCLE ( 'NONE', #15183, 31.99999999999998579 ) ;
#25324 = CARTESIAN_POINT ( 'NONE',  ( 11.99999999999999822, -74.65491531819111515, -8.830959090343204920 ) ) ;
#25325 = DIRECTION ( 'NONE',  ( 0.000000000000000000, 0.000000000000000000, 1.000000000000000000 ) ) ;
#25326 = EDGE_LOOP ( 'NONE', ( #30620, #33352, #10665, #31162 ) ) ;
#25327 = AXIS2_PLACEMENT_3D ( 'NONE', #11000, #48200, #2502 ) ;
#25328 = CARTESIAN_POINT ( 'NONE',  ( 70.53423027509757048, -217.0820393249931044, 5.500000000000000000 ) ) ;
#25329 = AXIS2_PLACEMENT_3D ( 'NONE', #43477, #8969, #38847 ) ;
#25330 = CARTESIAN_POINT ( 'NONE',  ( 10.00000000000000000, 15.33399622253481276, 80.55351364060595643 ) ) ;
#25331 = VERTEX_POINT ( 'NONE', #22119 ) ;
#25332 = ORIENTED_EDGE ( 'NONE', *, *, #8820, .T. ) ;
#25333 = EDGE_CURVE ( 'NONE', #47293, #35990, #21874, .T. ) ;
#25334 = EDGE_CURVE ( 'NONE', #25666, #3261, #33384, .T. ) ;
#25335 = CIRCLE ( 'NONE', #47221, 37.49900000000000944 ) ;
#25336 = AXIS2_PLACEMENT_3D ( 'NONE', #23775, #27953, #42871 ) ;
#25337 = ORIENTED_EDGE ( 'NONE', *, *, #32982, .T. ) ;
#25338 = CIRCLE ( 'NONE', #6589, 16.00000000000000000 ) ;
#25339 = VECTOR ( 'NONE', #34733, 1000.000000000000000 ) ;
#25340 = EDGE_CURVE ( 'NONE', #4586, #39044, #22375, .T. ) ;
#25341 = DIRECTION ( 'NONE',  ( 0.000000000000000000, -0.8090169943749403458, -0.5877852522924830181 ) ) ;
#25342 = ORIENTED_EDGE ( 'NONE', *, *, #29629, .F. ) ;
#25343 = EDGE_CURVE ( 'NONE', #42347, #15440, #12302, .T. ) ;
#25344 = VECTOR ( 'NONE', #8230, 1000.000000000000114 ) ;
#25345 = ORIENTED_EDGE ( 'NONE', *, *, #6629, .T. ) ;
#25346 = LINE ( 'NONE', #17766, #38673 ) ;
#25347 = CYLINDRICAL_SURFACE ( 'NONE', #32769, 31.99999999999999289 ) ;
#25348 = DIRECTION ( 'NONE',  ( 0.7585478161175706058, 0.6516173805718080692, -0.000000000000000000 ) ) ;
#25349 = ORIENTED_EDGE ( 'NONE', *, *, #23974, .T. ) ;
#25350 = CARTESIAN_POINT ( 'NONE',  ( -1.233757462863590115, -120.8531368722710795, -2.500000000000000000 ) ) ;
#25351 = EDGE_LOOP ( 'NONE', ( #21254, #46851, #36333, #16377 ) ) ;
#25352 = ORIENTED_EDGE ( 'NONE', *, *, #30386, .T. ) ;
#25353 = ORIENTED_EDGE ( 'NONE', *, *, #16352, .T. ) ;
#25354 = EDGE_CURVE ( 'NONE', #13186, #1317, #2126, .T. ) ;
#25355 = ADVANCED_FACE ( 'NONE', ( #33613 ), #15028, .T. ) ;
#25356 = CARTESIAN_POINT ( 'NONE',  ( 11.99999999999999822, 0.000000000000000000, 0.000000000000000000 ) ) ;
#25358 = ORIENTED_EDGE ( 'NONE', *, *, #35405, .T. ) ;
#25357 = CARTESIAN_POINT ( 'NONE',  ( 10.00000000000000000, -81.50828551894220197, -8.966570791701579779 ) ) ;
#25360 = LINE ( 'NONE', #40319, #41534 ) ;
#25359 = AXIS2_PLACEMENT_3D ( 'NONE', #28646, #40389, #10033 ) ;
#25361 = ORIENTED_EDGE ( 'NONE', *, *, #23473, .F. ) ;
#25362 = VERTEX_POINT ( 'NONE', #25065 ) ;
#25363 = ORIENTED_EDGE ( 'NONE', *, *, #6543, .T. ) ;
#25364 = CARTESIAN_POINT ( 'NONE',  ( 10.00000000000000000, -28.89263327155797967, 71.91182617369179297 ) ) ;
#25365 = ORIENTED_EDGE ( 'NONE', *, *, #31985, .F. ) ;
#25366 = VECTOR ( 'NONE', #10910, 1000.000000000000000 ) ;
#25367 = DIRECTION ( 'NONE',  ( 0.000000000000000000, 0.000000000000000000, 1.000000000000000000 ) ) ;
#25368 = VECTOR ( 'NONE', #37805, 1000.000000000000000 ) ;
#25369 = CARTESIAN_POINT ( 'NONE',  ( 10.00000000000000000, 41.76937507738788469, 62.50329211542452157 ) ) ;
#25370 = DIRECTION ( 'NONE',  ( -1.000000000000000000, 0.000000000000000000, -0.000000000000000000 ) ) ;
#25371 = DIRECTION ( 'NONE',  ( -1.000000000000000000, 0.000000000000000000, 0.000000000000000000 ) ) ;
#25372 = DIRECTION ( 'NONE',  ( 0.000000000000000000, 0.9876883405951381034, -0.1564344650402276216 ) ) ;
#25373 = CARTESIAN_POINT ( 'NONE',  ( 10.00000000000000000, -37.48860685352291711, 0.8828120875899322373 ) ) ;
#25374 = FACE_OUTER_BOUND ( 'NONE', #8842, .T. ) ;
#25375 = EDGE_CURVE ( 'NONE', #31941, #48222, #40013, .T. ) ;
#25376 = CARTESIAN_POINT ( 'NONE',  ( 10.00000000000000000, -41.81611651403864727, 3.925862922256025289 ) ) ;
#25377 = VECTOR ( 'NONE', #1352, 1000.000000000000000 ) ;
#25378 = AXIS2_PLACEMENT_3D ( 'NONE', #12899, #3908, #5540 ) ;
#25379 = VERTEX_POINT ( 'NONE', #1309 ) ;
#25380 = AXIS2_PLACEMENT_3D ( 'NONE', #43164, #31251, #42023 ) ;
#25381 = CARTESIAN_POINT ( 'NONE',  ( -3.000000000000000000, -19.89357724624987256, -12.59942793731086041 ) ) ;
#25382 = VECTOR ( 'NONE', #39260, 1000.000000000000000 ) ;
#25383 = VECTOR ( 'NONE', #2741, 1000.000000000000000 ) ;
#25384 = CARTESIAN_POINT ( 'NONE',  ( 10.00000000000000000, 17.67226234102874116, -33.17418723428288274 ) ) ;
#25385 = DIRECTION ( 'NONE',  ( -1.000000000000000000, -0.000000000000000000, -0.000000000000000000 ) ) ;
#25386 = DIRECTION ( 'NONE',  ( -1.000000000000000000, -0.000000000000000000, 0.000000000000000000 ) ) ;
#25387 = AXIS2_PLACEMENT_3D ( 'NONE', #42489, #27560, #34642 ) ;
#25388 = FACE_OUTER_BOUND ( 'NONE', #12373, .T. ) ;
#25389 = CARTESIAN_POINT ( 'NONE',  ( 15.00000000000000000, 6.762365576493647445, 25.66652317338391498 ) ) ;
#25390 = CARTESIAN_POINT ( 'NONE',  ( 22.94323693612312809, -114.6983135802921083, 5.500000000000000000 ) ) ;
#25391 = LINE ( 'NONE', #33701, #22212 ) ;
#25392 = VERTEX_POINT ( 'NONE', #8627 ) ;
#25393 = CARTESIAN_POINT ( 'NONE',  ( 10.00000000000000000, 75.11764819372149304, -2.946379043146603482 ) ) ;
#25394 = ORIENTED_EDGE ( 'NONE', *, *, #661, .F. ) ;
#25395 = ORIENTED_EDGE ( 'NONE', *, *, #36151, .F. ) ;
#25396 = EDGE_LOOP ( 'NONE', ( #26042, #29060, #11281, #48277 ) ) ;
#25397 = ORIENTED_EDGE ( 'NONE', *, *, #38472, .F. ) ;
#25398 = EDGE_CURVE ( 'NONE', #31758, #42670, #15433, .T. ) ;
#25399 = DIRECTION ( 'NONE',  ( 0.000000000000000000, 0.000000000000000000, 1.000000000000000000 ) ) ;
#25400 = CARTESIAN_POINT ( 'NONE',  ( 5.000000000000000000, 64.81221759200417409, -50.23322058963276504 ) ) ;
#25401 = ORIENTED_EDGE ( 'NONE', *, *, #46087, .T. ) ;
#25402 = ADVANCED_FACE ( 'NONE', ( #8401 ), #19887, .T. ) ;
#25403 = CIRCLE ( 'NONE', #1168, 82.00000000000000000 ) ;
#25404 = CIRCLE ( 'NONE', #27821, 31.99999999999999289 ) ;
#25405 = EDGE_CURVE ( 'NONE', #43819, #41954, #30438, .T. ) ;
#25406 = CARTESIAN_POINT ( 'NONE',  ( 10.00000000000000000, 0.000000000000000000, 0.000000000000000000 ) ) ;
#25407 = ORIENTED_EDGE ( 'NONE', *, *, #29006, .F. ) ;
#25408 = AXIS2_PLACEMENT_3D ( 'NONE', #46407, #8470, #19469 ) ;
#25409 = ORIENTED_EDGE ( 'NONE', *, *, #43590, .F. ) ;
#25410 = VECTOR ( 'NONE', #25785, 1000.000000000000000 ) ;
#25411 = AXIS2_PLACEMENT_3D ( 'NONE', #28854, #7306, #21750 ) ;
#25412 = EDGE_CURVE ( 'NONE', #19576, #461, #26525, .T. ) ;
#25413 = DIRECTION ( 'NONE',  ( 0.000000000000000000, 0.5877852522924741363, -0.8090169943749465631 ) ) ;
#25414 = AXIS2_PLACEMENT_3D ( 'NONE', #20891, #39742, #48024 ) ;
#25415 = VERTEX_POINT ( 'NONE', #44882 ) ;
#25416 = CARTESIAN_POINT ( 'NONE',  ( 11.99999999999999822, 0.000000000000000000, 0.000000000000000000 ) ) ;
#25417 = EDGE_CURVE ( 'NONE', #48416, #44214, #41223, .T. ) ;
#25418 = LINE ( 'NONE', #43558, #10323 ) ;
#25419 = AXIS2_PLACEMENT_3D ( 'NONE', #45755, #46485, #20519 ) ;
#25420 = DIRECTION ( 'NONE',  ( 0.000000000000000000, -0.3090169943749349613, -0.9510565162951576390 ) ) ;
#25421 = CARTESIAN_POINT ( 'NONE',  ( -7.469491406282117829, 4.756046723998917258, -64.01812422950395387 ) ) ;
#25422 = VERTEX_POINT ( 'NONE', #11370 ) ;
#25423 = ORIENTED_EDGE ( 'NONE', *, *, #30862, .T. ) ;
#25424 = CARTESIAN_POINT ( 'NONE',  ( 10.00000000000000000, 68.27212725128275395, 31.46837873495001503 ) ) ;
#25425 = ADVANCED_FACE ( 'NONE', ( #38263 ), #578, .F. ) ;
#25426 = FACE_OUTER_BOUND ( 'NONE', #4629, .T. ) ;
#25427 = ORIENTED_EDGE ( 'NONE', *, *, #38803, .T. ) ;
#25428 = ORIENTED_EDGE ( 'NONE', *, *, #453, .T. ) ;
#25429 = FACE_OUTER_BOUND ( 'NONE', #24765, .T. ) ;
#25430 = DIRECTION ( 'NONE',  ( -1.000000000000000000, -0.000000000000000000, -0.000000000000000000 ) ) ;
#25431 = ORIENTED_EDGE ( 'NONE', *, *, #16869, .F. ) ;
#25432 = ORIENTED_EDGE ( 'NONE', *, *, #10008, .F. ) ;
#25433 = LINE ( 'NONE', #29364, #33953 ) ;
#25434 = DIRECTION ( 'NONE',  ( 0.000000000000000000, 0.000000000000000000, 1.000000000000000000 ) ) ;
#25435 = DIRECTION ( 'NONE',  ( 0.000000000000000000, 0.000000000000000000, 1.000000000000000000 ) ) ;
#25436 = ORIENTED_EDGE ( 'NONE', *, *, #39233, .F. ) ;
#25437 = LINE ( 'NONE', #47703, #29699 ) ;
#25438 = DIRECTION ( 'NONE',  ( 0.000000000000000000, 1.000000000000000000, -0.000000000000000000 ) ) ;
#25439 = EDGE_CURVE ( 'NONE', #25379, #16993, #15280, .T. ) ;
#25440 = EDGE_LOOP ( 'NONE', ( #26006, #39086, #20617, #43766 ) ) ;
#25441 = AXIS2_PLACEMENT_3D ( 'NONE', #38750, #27486, #28194 ) ;
#25442 = CIRCLE ( 'NONE', #34077, 16.00000000000000000 ) ;
#25443 = CARTESIAN_POINT ( 'NONE',  ( -10.00000000000000000, 0.000000000000000000, 0.000000000000000000 ) ) ;
#25444 = DIRECTION ( 'NONE',  ( -1.000000000000000000, 0.000000000000000000, 0.000000000000000000 ) ) ;
#25445 = AXIS2_PLACEMENT_3D ( 'NONE', #18696, #45371, #25560 ) ;
#25446 = LINE ( 'NONE', #37678, #1797 ) ;
#25447 = FACE_OUTER_BOUND ( 'NONE', #9589, .T. ) ;
#25448 = CIRCLE ( 'NONE', #34053, 16.00000000000000000 ) ;
#25449 = CARTESIAN_POINT ( 'NONE',  ( -10.00000000000000000, 0.000000000000000000, 0.000000000000000000 ) ) ;
#25450 = VERTEX_POINT ( 'NONE', #26288 ) ;
#25451 = ORIENTED_EDGE ( 'NONE', *, *, #29832, .F. ) ;
#25452 = VERTEX_POINT ( 'NONE', #37533 ) ;
#25453 = EDGE_CURVE ( 'NONE', #39100, #17495, #35721, .T. ) ;
#25454 = CARTESIAN_POINT ( 'NONE',  ( -10.00000000000000000, 0.000000000000000000, 0.000000000000000000 ) ) ;
#25455 = EDGE_CURVE ( 'NONE', #31088, #39870, #45595, .T. ) ;
#25456 = ORIENTED_EDGE ( 'NONE', *, *, #33085, .F. ) ;
#25457 = AXIS2_PLACEMENT_3D ( 'NONE', #40010, #17721, #32884 ) ;
#25458 = VECTOR ( 'NONE', #22399, 1000.000000000000000 ) ;
#25459 = DIRECTION ( 'NONE',  ( 0.000000000000000000, 0.000000000000000000, -1.000000000000000000 ) ) ;
#25460 = ORIENTED_EDGE ( 'NONE', *, *, #28049, .T. ) ;
#25461 = EDGE_CURVE ( 'NONE', #30912, #9341, #37296, .T. ) ;
#25462 = AXIS2_PLACEMENT_3D ( 'NONE', #21608, #14016, #44360 ) ;
#25463 = ORIENTED_EDGE ( 'NONE', *, *, #31867, .T. ) ;
#25464 = EDGE_CURVE ( 'NONE', #13511, #47663, #15508, .T. ) ;
#25465 = ADVANCED_FACE ( 'NONE', ( #34566 ), #33851, .F. ) ;
#25466 = CARTESIAN_POINT ( 'NONE',  ( 11.99999999999999822, 74.74816331893477184, -33.71516098798660011 ) ) ;
#25467 = EDGE_LOOP ( 'NONE', ( #9887, #20406 ) ) ;
#25468 = CARTESIAN_POINT ( 'NONE',  ( 10.00000000000000000, -73.44644590900078640, 24.73286445877676343 ) ) ;
#25469 = ORIENTED_EDGE ( 'NONE', *, *, #5688, .T. ) ;
#25470 = ORIENTED_EDGE ( 'NONE', *, *, #15948, .F. ) ;
#25471 = LINE ( 'NONE', #36251, #9447 ) ;
#25472 = VECTOR ( 'NONE', #12400, 1000.000000000000000 ) ;
#25473 = CIRCLE ( 'NONE', #42724, 31.99999999999998579 ) ;
#25474 = CARTESIAN_POINT ( 'NONE',  ( 15.00000000000000000, 18.84667830672579569, -18.68964196561269375 ) ) ;
#25475 = CARTESIAN_POINT ( 'NONE',  ( 0.000000000000000000, 0.000000000000000000, 0.000000000000000000 ) ) ;
#25476 = ORIENTED_EDGE ( 'NONE', *, *, #25043, .T. ) ;
#25477 = DIRECTION ( 'NONE',  ( 0.000000000000000000, 0.000000000000000000, 1.000000000000000000 ) ) ;
#25478 = VERTEX_POINT ( 'NONE', #41691 ) ;
#25479 = AXIS2_PLACEMENT_3D ( 'NONE', #24310, #20886, #39243 ) ;
#25480 = DIRECTION ( 'NONE',  ( -1.000000000000000000, 0.000000000000000000, 0.000000000000000000 ) ) ;
#25481 = DIRECTION ( 'NONE',  ( -1.000000000000000000, -0.000000000000000000, 0.000000000000000000 ) ) ;
#25482 = ORIENTED_EDGE ( 'NONE', *, *, #23760, .F. ) ;
#25483 = DIRECTION ( 'NONE',  ( 0.000000000000000000, -0.4999999999999912847, -0.8660254037844435926 ) ) ;
#25484 = DIRECTION ( 'NONE',  ( 0.000000000000000000, 0.4539904997395414754, 0.8910065241883706744 ) ) ;
#25486 = ORIENTED_EDGE ( 'NONE', *, *, #3815, .T. ) ;
#25485 = CARTESIAN_POINT ( 'NONE',  ( 8.700667342345820288, -98.11853780484867116, 5.500000000000000000 ) ) ;
#25487 = EDGE_CURVE ( 'NONE', #29919, #29511, #48226, .T. ) ;
#25488 = DIRECTION ( 'NONE',  ( -1.000000000000000000, -0.000000000000000000, -0.000000000000000000 ) ) ;
#25489 = ORIENTED_EDGE ( 'NONE', *, *, #7714, .F. ) ;
#25490 = CLOSED_SHELL ( 'NONE', ( #22584, #16169, #7547, #40713, #30442, #8840, #31133, #22641, #38174, #36806, #47135, #13147, #32394, #2222, #8432, #16203, #19214, #22379, #19169, #11766, #23525, #17302, #24926, #26655, #15000, #33165, #46144, #5012, #15321, #18341, #5861, #1849, #48392, #25585, #42103, #24373, #13665, #35974, #5608, #30735, #26368, #37894, #14252, #7065, #43014, #27707, #47572, #23884, #38074, #292, #47450, #23095, #24156, #5831, #13008, #15546, #28416, #7644, #31772, #23050, #11444, #8397, #21293, #11826, #19797, #31208, #34404, #6902, #5809, #41374, #16216, #13277, #30494, #36401, #7726, #11946, #23924, #41136, #19862, #22088, #29974, #23112, #45309, #43045, #6154, #48062, #44268, #28122, #35185, #38498, #5045, #37744, #7047, #39702, #17501, #17558, #2851, #10563, #24097, #31396, #1954, #17182, #24121, #43113, #13532, #29210, #20111, #31028, #21315, #44622, #47538, #47334, #12167, #37195, #14309, #20218, #19605, #45396, #14934, #19075, #31281, #8884, #44395, #1964, #28179, #18619, #8718, #26519, #13667, #32676, #39359, #22947, #26854, #20057, #39998, #12503, #23255, #7349, #6440, #22443, #18665, #42167, #35090, #9020, #2576, #43511, #45875, #10676, #8007, #2587, #38955, #4874, #26026, #29071, #9231, #40879, #1465, #30953, #48339, #47301, #20338, #40184, #29998, #17821, #19433, #33594, #47341, #23754, #2025, #12660, #37808, #20550, #44466, #8890, #1346, #28678, #15234, #27402, #2433, #29495, #40467, #26771, #35707, #44432, #44921, #42184, #22826, #17827, #41194, #13822, #26510, #21749, #35241, #3411, #42822, #38796, #39368, #20230, #32711, #7915, #32933, #42596, #46370, #34676, #19271, #39179, #6659, #19881, #48219, #972, #25355, #22452, #11677, #36697, #20912, #35744, #2323, #8726, #42251, #47517, #20070, #21516, #17938, #9952, #29063, #46826, #37564, #23406, #25574, #13888, #37629, #4480, #23578, #25784, #33043, #46097, #45229, #38534, #44589, #24664, #31142, #11572, #34290, #24976, #4712, #5877, #32918, #38029, #34192, #22276, #37027, #44421, #36753, #12448, #8508, #1247, #20588, #34342, #16370, #16467, #31683, #28939, #37516, #37840, #17355, #7522, #11042, #43868, #39460, #20371, #29906, #26361, #2865, #14930, #7688, #18116, #35040, #1163, #12735, #22487, #28999, #41, #22272, #8524, #8254, #10619, #8067, #20282, #27136, #22785, #34748, #32222, #18672, #2239, #5061, #19131, #53, #24100, #5762, #43764, #26013, #20994, #17783, #46057, #26322, #42393, #34551, #30816, #4420, #47203, #26922, #29621, #1995, #21426, #28497, #45941, #28996, #8393, #27314, #38468, #42865, #39912, #42719, #17117, #7883, #11829, #26913, #4662, #35180, #5154, #8661, #991, #46258 ) ) ;
#25491 = DIRECTION ( 'NONE',  ( -1.000000000000000000, -0.000000000000000000, 0.000000000000000000 ) ) ;
#25492 = VERTEX_POINT ( 'NONE', #1044 ) ;
#25493 = VERTEX_POINT ( 'NONE', #41453 ) ;
#25494 = FACE_OUTER_BOUND ( 'NONE', #3155, .T. ) ;
#25495 = CARTESIAN_POINT ( 'NONE',  ( 11.99999999999999822, -20.40083707022935400, 72.35432306680478121 ) ) ;
#25496 = EDGE_LOOP ( 'NONE', ( #45017, #9051, #30188, #32686 ) ) ;
#25497 = DIRECTION ( 'NONE',  ( -1.000000000000000000, 0.000000000000000000, 0.000000000000000000 ) ) ;
#25498 = CIRCLE ( 'NONE', #27054, 77.49900000000000944 ) ;
#25499 = DIRECTION ( 'NONE',  ( -1.000000000000000000, 0.000000000000000000, 0.000000000000000000 ) ) ;
#25500 = LINE ( 'NONE', #43866, #39923 ) ;
#25501 = ORIENTED_EDGE ( 'NONE', *, *, #22969, .F. ) ;
#25502 = EDGE_CURVE ( 'NONE', #6185, #32005, #39656, .T. ) ;
#25503 = AXIS2_PLACEMENT_3D ( 'NONE', #34822, #15988, #1305 ) ;
#25504 = DIRECTION ( 'NONE',  ( -1.000000000000000000, 0.000000000000000000, -0.000000000000000000 ) ) ;
#25505 = LINE ( 'NONE', #40928, #39182 ) ;
#25506 = CIRCLE ( 'NONE', #27882, 35.50000000000000711 ) ;
#25507 = CARTESIAN_POINT ( 'NONE',  ( 13.83832728059186046, -142.6495187161941089, 5.500000000000000000 ) ) ;
#25508 = LINE ( 'NONE', #3224, #463 ) ;
#25509 = DIRECTION ( 'NONE',  ( 0.000000000000000000, 0.000000000000000000, 1.000000000000000000 ) ) ;
#25510 = DIRECTION ( 'NONE',  ( -1.000000000000000000, 0.000000000000000000, 0.000000000000000000 ) ) ;
#25511 = LINE ( 'NONE', #21110, #23171 ) ;
#25512 = FACE_OUTER_BOUND ( 'NONE', #21153, .T. ) ;
#25513 = CARTESIAN_POINT ( 'NONE',  ( 10.00000000000000000, 46.54456581323888997, -59.03342792756214408 ) ) ;
#25514 = CARTESIAN_POINT ( 'NONE',  ( 2.047646702416564768, -96.54137380445985173, 5.500000000000000000 ) ) ;
#25515 = CARTESIAN_POINT ( 'NONE',  ( 12.00000000000000000, 23.49999999999999645, 1.499999999999995337 ) ) ;
#25516 = ORIENTED_EDGE ( 'NONE', *, *, #31861, .F. ) ;
#25517 = CYLINDRICAL_SURFACE ( 'NONE', #11315, 31.99999999999998579 ) ;
#25518 = ORIENTED_EDGE ( 'NONE', *, *, #47506, .T. ) ;
#25519 = ADVANCED_FACE ( 'NONE', ( #12328 ), #7911, .T. ) ;
#25520 = DIRECTION ( 'NONE',  ( 1.000000000000000000, 0.000000000000000000, 0.000000000000000000 ) ) ;
#25521 = DIRECTION ( 'NONE',  ( 0.7533909544171997208, 0.6575728627325956310, 9.860761315262647568E-31 ) ) ;
#25522 = EDGE_CURVE ( 'NONE', #36119, #11835, #24798, .T. ) ;
#25523 = CARTESIAN_POINT ( 'NONE',  ( 0.000000000000000000, -71.21200624218825226, 40.65526001592589722 ) ) ;
#25524 = VERTEX_POINT ( 'NONE', #5955 ) ;
#25525 = AXIS2_PLACEMENT_3D ( 'NONE', #3780, #45149, #41970 ) ;
#25526 = EDGE_CURVE ( 'NONE', #29354, #46298, #24293, .T. ) ;
#25527 = CARTESIAN_POINT ( 'NONE',  ( 10.00000000000000000, -55.16347631943084195, 60.67117009219116852 ) ) ;
#25529 = EDGE_CURVE ( 'NONE', #8125, #7607, #21090, .T. ) ;
#25528 = EDGE_LOOP ( 'NONE', ( #12382, #16903, #33338, #9022 ) ) ;
#25530 = CIRCLE ( 'NONE', #12284, 82.00000000000000000 ) ;
#25531 = VECTOR ( 'NONE', #21003, 1000.000000000000000 ) ;
#25532 = DIRECTION ( 'NONE',  ( 1.000000000000000000, 0.000000000000000000, 0.000000000000000000 ) ) ;
#25533 = EDGE_LOOP ( 'NONE', ( #31900, #31847, #22448, #24879 ) ) ;
#25534 = CARTESIAN_POINT ( 'NONE',  ( 11.99999999999999822, -23.16143007188376757, -73.95703589263997912 ) ) ;
#25536 = VERTEX_POINT ( 'NONE', #6183 ) ;
#25535 = LINE ( 'NONE', #6944, #32454 ) ;
#25537 = ORIENTED_EDGE ( 'NONE', *, *, #44470, .T. ) ;
#25538 = DIRECTION ( 'NONE',  ( 0.000000000000000000, -0.2334453638559125521, 0.9723699203976750027 ) ) ;
#25539 = ORIENTED_EDGE ( 'NONE', *, *, #26136, .T. ) ;
#25540 = VECTOR ( 'NONE', #19192, 1000.000000000000114 ) ;
#25541 = DIRECTION ( 'NONE',  ( -1.000000000000000000, 0.000000000000000000, 0.000000000000000000 ) ) ;
#25542 = DIRECTION ( 'NONE',  ( -1.000000000000000000, -0.000000000000000000, -0.000000000000000000 ) ) ;
#25543 = CARTESIAN_POINT ( 'NONE',  ( 10.00000000000000000, -10.96151621346514382, 35.95386929396252640 ) ) ;
#25544 = ORIENTED_EDGE ( 'NONE', *, *, #37455, .F. ) ;
#25545 = AXIS2_PLACEMENT_3D ( 'NONE', #33670, #33442, #29762 ) ;
#25546 = ORIENTED_EDGE ( 'NONE', *, *, #33559, .T. ) ;
#25547 = CYLINDRICAL_SURFACE ( 'NONE', #24035, 16.00000000000000000 ) ;
#25548 = VERTEX_POINT ( 'NONE', #5454 ) ;
#25549 = ORIENTED_EDGE ( 'NONE', *, *, #1337, .F. ) ;
#25550 = DIRECTION ( 'NONE',  ( 0.000000000000000000, 0.5877852522924685852, 0.8090169943749507819 ) ) ;
#25551 = VECTOR ( 'NONE', #46000, 1000.000000000000000 ) ;
#25552 = DIRECTION ( 'NONE',  ( 0.000000000000000000, 0.000000000000000000, 1.000000000000000000 ) ) ;
#25553 = CYLINDRICAL_SURFACE ( 'NONE', #25035, 37.49900000000000233 ) ;
#25554 = CARTESIAN_POINT ( 'NONE',  ( 10.00000000000000000, 68.27212725128275395, 31.46837873495001503 ) ) ;
#25555 = ORIENTED_EDGE ( 'NONE', *, *, #13677, .T. ) ;
#25556 = CARTESIAN_POINT ( 'NONE',  ( 11.99999999999999822, -15.33399622253425321, -80.55351364060605590 ) ) ;
#25557 = DIRECTION ( 'NONE',  ( 0.000000000000000000, -0.5877852522924802425, 0.8090169943749422332 ) ) ;
#25558 = DIRECTION ( 'NONE',  ( -1.000000000000000000, -0.000000000000000000, -0.000000000000000000 ) ) ;
#25559 = DIRECTION ( 'NONE',  ( -0.5687579148473765889, 0.8225049752423776450, 0.000000000000000000 ) ) ;
#25560 = DIRECTION ( 'NONE',  ( 0.000000000000000000, -0.5224985647159559043, 0.8526401643540879594 ) ) ;
#25561 = VERTEX_POINT ( 'NONE', #16470 ) ;
#25562 = AXIS2_PLACEMENT_3D ( 'NONE', #347, #26054, #19418 ) ;
#25563 = CARTESIAN_POINT ( 'NONE',  ( 0.000000000000000000, -14.66109333815513160, 73.73191006444567108 ) ) ;
#25564 = EDGE_CURVE ( 'NONE', #35109, #22226, #24820, .T. ) ;
#25565 = DIRECTION ( 'NONE',  ( 0.000000000000000000, 0.7604059656000276002, 0.6494480483301877660 ) ) ;
#25566 = DIRECTION ( 'NONE',  ( -1.000000000000000000, 0.000000000000000000, -0.000000000000000000 ) ) ;
#25567 = DIRECTION ( 'NONE',  ( -1.000000000000000000, -0.000000000000000000, -0.000000000000000000 ) ) ;
#25568 = AXIS2_PLACEMENT_3D ( 'NONE', #2115, #27335, #42031 ) ;
#25569 = ORIENTED_EDGE ( 'NONE', *, *, #6196, .T. ) ;
#25570 = DIRECTION ( 'NONE',  ( -1.000000000000000000, 0.000000000000000000, 0.000000000000000000 ) ) ;
#25571 = CARTESIAN_POINT ( 'NONE',  ( 10.00000000000000000, -40.65526001592664329, 71.21200624218782593 ) ) ;
#25572 = ORIENTED_EDGE ( 'NONE', *, *, #28028, .F. ) ;
#25573 = CYLINDRICAL_SURFACE ( 'NONE', #16072, 32.50000000000000000 ) ;
#25574 = ADVANCED_FACE ( 'NONE', ( #36025 ), #39724, .T. ) ;
#25575 = DIRECTION ( 'NONE',  ( -0.000000000000000000, -0.000000000000000000, -1.000000000000000000 ) ) ;
#25576 = EDGE_CURVE ( 'NONE', #526, #29716, #24063, .T. ) ;
#25577 = EDGE_CURVE ( 'NONE', #17516, #42227, #42908, .T. ) ;
#25578 = VERTEX_POINT ( 'NONE', #31421 ) ;
#25579 = ORIENTED_EDGE ( 'NONE', *, *, #37524, .F. ) ;
#25580 = AXIS2_PLACEMENT_3D ( 'NONE', #47576, #36803, #14556 ) ;
#25581 = ORIENTED_EDGE ( 'NONE', *, *, #20730, .T. ) ;
#25582 = ADVANCED_FACE ( 'NONE', ( #39483 ), #13519, .F. ) ;
#25583 = ORIENTED_EDGE ( 'NONE', *, *, #22706, .T. ) ;
#25584 = CIRCLE ( 'NONE', #4501, 15.99999999999999822 ) ;
#25585 = ADVANCED_FACE ( 'NONE', ( #16953 ), #35794, .T. ) ;
#25586 = DIRECTION ( 'NONE',  ( -0.8541291221503275466, 0.5200609990132993854, 0.000000000000000000 ) ) ;
#25587 = VERTEX_POINT ( 'NONE', #35307 ) ;
#25588 = EDGE_LOOP ( 'NONE', ( #38604, #30803, #31835, #8497 ) ) ;
#25589 = VECTOR ( 'NONE', #15952, 1000.000000000000000 ) ;
#25590 = LINE ( 'NONE', #40532, #40238 ) ;
#25591 = CARTESIAN_POINT ( 'NONE',  ( 11.99999999999999822, -65.64334221924937651, 41.19522573413711797 ) ) ;
#25593 = ORIENTED_EDGE ( 'NONE', *, *, #14426, .T. ) ;
#25592 = DIRECTION ( 'NONE',  ( -1.000000000000000000, 0.000000000000000000, 0.000000000000000000 ) ) ;
#25594 = ORIENTED_EDGE ( 'NONE', *, *, #16087, .F. ) ;
#25595 = CARTESIAN_POINT ( 'NONE',  ( 0.000000000000000000, 0.000000000000000000, 0.000000000000000000 ) ) ;
#25596 = ORIENTED_EDGE ( 'NONE', *, *, #43560, .T. ) ;
#25597 = ORIENTED_EDGE ( 'NONE', *, *, #37577, .F. ) ;
#25598 = VERTEX_POINT ( 'NONE', #13284 ) ;
#25599 = FACE_OUTER_BOUND ( 'NONE', #5481, .T. ) ;
#25600 = PLANE ( 'NONE',  #64 ) ;
#25601 = VECTOR ( 'NONE', #354, 1000.000000000000000 ) ;
#25602 = DIRECTION ( 'NONE',  ( 0.000000000000000000, 0.000000000000000000, 1.000000000000000000 ) ) ;
#25603 = ORIENTED_EDGE ( 'NONE', *, *, #30051, .F. ) ;
#25604 = EDGE_LOOP ( 'NONE', ( #26997, #29294, #35951, #17956 ) ) ;
#25605 = CARTESIAN_POINT ( 'NONE',  ( -23.25244084006223133, -132.7111759872722416, -2.500000000000000000 ) ) ;
#25606 = ORIENTED_EDGE ( 'NONE', *, *, #28954, .T. ) ;
#25607 = LINE ( 'NONE', #37597, #33979 ) ;
#25608 = DIRECTION ( 'NONE',  ( 0.6862798483830533369, 0.7273375899149812085, 0.000000000000000000 ) ) ;
#25609 = DIRECTION ( 'NONE',  ( 0.000000000000000000, 0.000000000000000000, 1.000000000000000000 ) ) ;
#25610 = ORIENTED_EDGE ( 'NONE', *, *, #30116, .F. ) ;
#25611 = DIRECTION ( 'NONE',  ( 0.000000000000000000, 0.000000000000000000, 1.000000000000000000 ) ) ;
#25612 = DIRECTION ( 'NONE',  ( 1.000000000000000000, 0.000000000000000000, 0.000000000000000000 ) ) ;
#25613 = CARTESIAN_POINT ( 'NONE',  ( -10.00000000000000000, 0.000000000000000000, 0.000000000000000000 ) ) ;
#25614 = EDGE_CURVE ( 'NONE', #32530, #43867, #28206, .T. ) ;
#25615 = CARTESIAN_POINT ( 'NONE',  ( 0.000000000000000000, -32.34446384429989507, 26.79245525562703278 ) ) ;
#25616 = LINE ( 'NONE', #37121, #21214 ) ;
#25617 = VECTOR ( 'NONE', #22319, 1000.000000000000114 ) ;
#25618 = ADVANCED_FACE ( 'NONE', ( #24784 ), #16716, .T. ) ;
#25619 = ORIENTED_EDGE ( 'NONE', *, *, #11402, .F. ) ;
#25620 = DIRECTION ( 'NONE',  ( -1.000000000000000000, 0.000000000000000000, 0.000000000000000000 ) ) ;
#25621 = EDGE_CURVE ( 'NONE', #9834, #34570, #34208, .T. ) ;
#25622 = VECTOR ( 'NONE', #41420, 1000.000000000000000 ) ;
#25623 = CARTESIAN_POINT ( 'NONE',  ( 10.00000000000000000, -37.58145647212455032, 16.68533520207890319 ) ) ;
#25624 = CARTESIAN_POINT ( 'NONE',  ( 0.000000000000000000, -68.27212725128298132, 31.46837873494953541 ) ) ;
#25625 = DIRECTION ( 'NONE',  ( 0.000000000000000000, 0.000000000000000000, -1.000000000000000000 ) ) ;
#25626 = AXIS2_PLACEMENT_3D ( 'NONE', #43500, #44450, #40315 ) ;
#25627 = EDGE_CURVE ( 'NONE', #31834, #16291, #32135, .T. ) ;
#25628 = CARTESIAN_POINT ( 'NONE',  ( 0.000000000000000000, -26.79245525562738095, 32.34446384429961796 ) ) ;
#25629 = FACE_OUTER_BOUND ( 'NONE', #30282, .T. ) ;
#25630 = LINE ( 'NONE', #40571, #31829 ) ;
#25631 = CARTESIAN_POINT ( 'NONE',  ( 10.00000000000000000, 12.93880638057426502, -76.41127070299258150 ) ) ;
#25632 = DIRECTION ( 'NONE',  ( 0.000000000000000000, -0.7071067811865389130, -0.7071067811865561215 ) ) ;
#25633 = FILL_AREA_STYLE ('',( #33234 ) ) ;
#25634 = DIRECTION ( 'NONE',  ( 0.000000000000000000, -0.9781476007338070211, 0.2079116908177532363 ) ) ;
#25635 = ADVANCED_FACE ( 'NONE', ( #20616 ), #20140, .F. ) ;
#25636 = EDGE_CURVE ( 'NONE', #9618, #26872, #12803, .T. ) ;
#25637 = ORIENTED_EDGE ( 'NONE', *, *, #7410, .F. ) ;
#25638 = CIRCLE ( 'NONE', #48320, 31.99999999999999289 ) ;
#25639 = ORIENTED_EDGE ( 'NONE', *, *, #16357, .T. ) ;
#25640 = DIRECTION ( 'NONE',  ( 0.000000000000000000, 0.000000000000000000, -1.000000000000000000 ) ) ;
#25641 = CARTESIAN_POINT ( 'NONE',  ( 0.000000000000000000, 0.000000000000000000, 52.00000000000002132 ) ) ;
#25642 = ORIENTED_EDGE ( 'NONE', *, *, #26979, .T. ) ;
#25643 = ADVANCED_FACE ( 'NONE', ( #24066 ), #38994, .T. ) ;
#25644 = DIRECTION ( 'NONE',  ( 0.7585478161175723821, 0.6516173805718057377, -0.000000000000000000 ) ) ;
#25645 = ORIENTED_EDGE ( 'NONE', *, *, #44315, .F. ) ;
#25646 = EDGE_LOOP ( 'NONE', ( #15754, #26233 ) ) ;
#25647 = CIRCLE ( 'NONE', #24137, 32.00000000000000000 ) ;
#25648 = CYLINDRICAL_SURFACE ( 'NONE', #840, 82.00000000000000000 ) ;
#25649 = EDGE_LOOP ( 'NONE', ( #6504, #21459, #32432, #9099 ) ) ;
#25650 = CARTESIAN_POINT ( 'NONE',  ( 11.99999999999999822, -74.65374052328644439, -8.840884882375878107 ) ) ;
#25651 = VERTEX_POINT ( 'NONE', #44343 ) ;
#25652 = CARTESIAN_POINT ( 'NONE',  ( 50.00005079999999680, 2.571758278209441661E-15, -21.00000000000000000 ) ) ;
#25653 = CARTESIAN_POINT ( 'NONE',  ( 11.99999999999999822, 51.02545421589402252, -55.20638768913705263 ) ) ;
#25654 = AXIS2_PLACEMENT_3D ( 'NONE', #40475, #3988, #37272 ) ;
#25655 = DIRECTION ( 'NONE',  ( 0.000000000000000000, 0.000000000000000000, 1.000000000000000000 ) ) ;
#25656 = ORIENTED_EDGE ( 'NONE', *, *, #15695, .T. ) ;
#25657 = ORIENTED_EDGE ( 'NONE', *, *, #10219, .T. ) ;
#25658 = CIRCLE ( 'NONE', #6159, 15.99999999999999822 ) ;
#25659 = DIRECTION ( 'NONE',  ( 0.000000000000000000, -0.4539904997395541875, 0.8910065241883641241 ) ) ;
#25660 = CARTESIAN_POINT ( 'NONE',  ( -23.54415474984308787, -120.4156646670583086, 5.500000000000000000 ) ) ;
#25661 = EDGE_CURVE ( 'NONE', #31364, #40697, #25722, .T. ) ;
#25662 = ORIENTED_EDGE ( 'NONE', *, *, #37638, .T. ) ;
#25663 = VERTEX_POINT ( 'NONE', #48001 ) ;
#25664 = DIRECTION ( 'NONE',  ( 0.000000000000000000, 0.000000000000000000, 1.000000000000000000 ) ) ;
#25665 = DIRECTION ( 'NONE',  ( 0.000000000000000000, 0.9510565162951544194, -0.3090169943749446757 ) ) ;
#25666 = VERTEX_POINT ( 'NONE', #47525 ) ;
#25667 = ORIENTED_EDGE ( 'NONE', *, *, #3692, .T. ) ;
#25668 = EDGE_CURVE ( 'NONE', #3891, #17338, #33418, .T. ) ;
#25669 = CARTESIAN_POINT ( 'NONE',  ( 5.000000000000000000, -15.48615015657610705, 39.04073710021338428 ) ) ;
#25670 = DIRECTION ( 'NONE',  ( -1.000000000000000000, -0.000000000000000000, -0.000000000000000000 ) ) ;
#25671 = DIRECTION ( 'NONE',  ( -0.000000000000000000, -0.000000000000000000, -1.000000000000000000 ) ) ;
#25672 = DIRECTION ( 'NONE',  ( 0.000000000000000000, -0.7431448254773954654, 0.6691306063588569053 ) ) ;
#25673 = CARTESIAN_POINT ( 'NONE',  ( 0.000000000000000000, -81.96053171279903893, 2.543863470248101333 ) ) ;
#25674 = EDGE_CURVE ( 'NONE', #38938, #44456, #3458, .T. ) ;
#25675 = DIRECTION ( 'NONE',  ( 0.000000000000000000, 0.1564344650402312020, -0.9876883405951376593 ) ) ;
#25676 = DIRECTION ( 'NONE',  ( 0.000000000000000000, -1.000000000000000000, -0.000000000000000000 ) ) ;
#25677 = CARTESIAN_POINT ( 'NONE',  ( 0.000000000000000000, 35.92658777277525672, -10.74501242461245809 ) ) ;
#25678 = ORIENTED_EDGE ( 'NONE', *, *, #24048, .T. ) ;
#25679 = AXIS2_PLACEMENT_3D ( 'NONE', #29296, #40071, #36396 ) ;
#25680 = DIRECTION ( 'NONE',  ( -1.000000000000000000, -0.000000000000000000, -0.000000000000000000 ) ) ;
#25681 = CARTESIAN_POINT ( 'NONE',  ( 11.99999999999999822, -28.89263327155693517, -71.91182617369219088 ) ) ;
#25682 = AXIS2_PLACEMENT_3D ( 'NONE', #4838, #44999, #4119 ) ;
#25683 = FACE_OUTER_BOUND ( 'NONE', #38927, .T. ) ;
#25684 = ORIENTED_EDGE ( 'NONE', *, *, #9433, .F. ) ;
#25685 = ADVANCED_FACE ( 'NONE', ( #44097, #18132 ), #7135, .F. ) ;
#25686 = ADVANCED_FACE ( 'NONE', ( #28918 ), #36985, .F. ) ;
#25687 = EDGE_LOOP ( 'NONE', ( #1911, #37909, #41316, #30684 ) ) ;
#25688 = ORIENTED_EDGE ( 'NONE', *, *, #37922, .F. ) ;
#25689 = EDGE_CURVE ( 'NONE', #40958, #24649, #18394, .T. ) ;
#25690 = UNCERTAINTY_MEASURE_WITH_UNIT (LENGTH_MEASURE( 1.000000000000000082E-05 ), #19970, 'distance_accuracy_value', 'NONE');
#25691 = DIRECTION ( 'NONE',  ( 0.000000000000000000, 0.07845909572783797692, 0.9969173337331285190 ) ) ;
#25692 = DIRECTION ( 'NONE',  ( -1.000000000000000000, 0.000000000000000000, 0.000000000000000000 ) ) ;
#25693 = ORIENTED_EDGE ( 'NONE', *, *, #44712, .F. ) ;
#25694 = ADVANCED_FACE ( 'NONE', ( #33074 ), #6896, .T. ) ;
#25695 = ORIENTED_EDGE ( 'NONE', *, *, #6695, .T. ) ;
#25696 = APPLICATION_CONTEXT ( 'automotive_design' ) ;
#25697 = LINE ( 'NONE', #40174, #33513 ) ;
#25698 = VERTEX_POINT ( 'NONE', #44577 ) ;
#25699 = LINE ( 'NONE', #18114, #4987 ) ;
#25700 = VERTEX_POINT ( 'NONE', #43855 ) ;
#25701 = EDGE_LOOP ( 'NONE', ( #44543, #24772, #2914, #12135 ) ) ;
#25702 = ORIENTED_EDGE ( 'NONE', *, *, #21819, .F. ) ;
#25703 = FACE_OUTER_BOUND ( 'NONE', #6421, .T. ) ;
#25704 = VERTEX_POINT ( 'NONE', #21335 ) ;
#25705 = CARTESIAN_POINT ( 'NONE',  ( 11.99999999999999822, 70.52718814184260054, 26.02418014898334420 ) ) ;
#25706 = CIRCLE ( 'NONE', #14802, 31.99999999999998579 ) ;
#25707 = EDGE_LOOP ( 'NONE', ( #29543, #9165, #948, #34452 ) ) ;
#25708 = CARTESIAN_POINT ( 'NONE',  ( -17.09243336300205129, -103.8724235629982502, 2.500000000000000000 ) ) ;
#25709 = VERTEX_POINT ( 'NONE', #11052 ) ;
#25710 = AXIS2_PLACEMENT_3D ( 'NONE', #30784, #37881, #670 ) ;
#25711 = CARTESIAN_POINT ( 'NONE',  ( 10.00000000000000000, -39.04073710021356192, 15.48615015657568250 ) ) ;
#25712 = CIRCLE ( 'NONE', #30323, 31.99999999999998579 ) ;
#25713 = CARTESIAN_POINT ( 'NONE',  ( 15.00000000000000000, 24.81905959214260804, -9.408202855044828894 ) ) ;
#25714 = ORIENTED_EDGE ( 'NONE', *, *, #17224, .F. ) ;
#25715 = DIRECTION ( 'NONE',  ( 0.000000000000000000, 0.000000000000000000, 1.000000000000000000 ) ) ;
#25716 = CARTESIAN_POINT ( 'NONE',  ( 0.000000000000000000, 0.000000000000000000, 0.000000000000000000 ) ) ;
#25717 = ORIENTED_EDGE ( 'NONE', *, *, #45460, .T. ) ;
#25719 = EDGE_LOOP ( 'NONE', ( #27742, #11707 ) ) ;
#25718 = LINE ( 'NONE', #21587, #43007 ) ;
#25720 = DIRECTION ( 'NONE',  ( 1.000000000000000000, 0.000000000000000000, 0.000000000000000000 ) ) ;
#25721 = ORIENTED_EDGE ( 'NONE', *, *, #26550, .F. ) ;
#25722 = LINE ( 'NONE', #17668, #29505 ) ;
#25723 = ORIENTED_EDGE ( 'NONE', *, *, #255, .F. ) ;
#25724 = EDGE_LOOP ( 'NONE', ( #6130, #40198, #204, #33120 ) ) ;
#25725 = DIRECTION ( 'NONE',  ( 0.000000000000000000, 0.000000000000000000, 1.000000000000000000 ) ) ;
#25726 = DIRECTION ( 'NONE',  ( -1.000000000000000000, 0.000000000000000000, 0.000000000000000000 ) ) ;
#25727 = ORIENTED_EDGE ( 'NONE', *, *, #9455, .T. ) ;
#25728 = EDGE_CURVE ( 'NONE', #19113, #6225, #25971, .T. ) ;
#25729 = CARTESIAN_POINT ( 'NONE',  ( 11.99999999999999822, -0.8261519478425843888, -77.49459641780887864 ) ) ;
#25730 = ORIENTED_EDGE ( 'NONE', *, *, #5428, .T. ) ;
#25731 = CARTESIAN_POINT ( 'NONE',  ( 0.000000000000000000, 0.000000000000000000, 0.000000000000000000 ) ) ;
#25732 = CARTESIAN_POINT ( 'NONE',  ( -14.87942725330654348, -141.9795960975983178, 5.500000000000000000 ) ) ;
#25733 = ORIENTED_EDGE ( 'NONE', *, *, #17838, .F. ) ;
#25734 = EDGE_CURVE ( 'NONE', #16268, #36912, #37238, .T. ) ;
#25735 = DIRECTION ( 'NONE',  ( 1.000000000000000000, 0.000000000000000000, 0.000000000000000000 ) ) ;
#25736 = ADVANCED_FACE ( 'NONE', ( #32372 ), #40441, .T. ) ;
#25737 = FACE_OUTER_BOUND ( 'NONE', #42604, .T. ) ;
#25738 = MECHANICAL_DESIGN_GEOMETRIC_PRESENTATION_REPRESENTATION (  '', ( #13251 ), #42946 ) ;
#25739 = DIRECTION ( 'NONE',  ( -1.000000000000000000, 0.000000000000000000, 0.000000000000000000 ) ) ;
#25740 = ORIENTED_EDGE ( 'NONE', *, *, #43456, .T. ) ;
#25741 = CARTESIAN_POINT ( 'NONE',  ( 0.000000000000000000, -3.894527615417340272, -81.90746397400393164 ) ) ;
#25743 = EDGE_CURVE ( 'NONE', #15551, #22551, #13773, .T. ) ;
#25742 = DIRECTION ( 'NONE',  ( -1.000000000000000000, -0.000000000000000000, 0.000000000000000000 ) ) ;
#25744 = CARTESIAN_POINT ( 'NONE',  ( 11.99999999999999822, -69.42325613327466272, 34.44570377933573724 ) ) ;
#25745 = CARTESIAN_POINT ( 'NONE',  ( 0.000000000000000000, -29.01471420065616513, 76.69515212746007649 ) ) ;
#25746 = CARTESIAN_POINT ( 'NONE',  ( 4.348517481000897078, -143.0941636721797465, 2.500000000000000000 ) ) ;
#25747 = CARTESIAN_POINT ( 'NONE',  ( 5.000000000000002665, -3.894527615418464705, 81.90746397400387480 ) ) ;
#25748 = CARTESIAN_POINT ( 'NONE',  ( -26.53422223201112828, -120.6595836127786043, 5.500000000000000000 ) ) ;
#25749 = FACE_OUTER_BOUND ( 'NONE', #1599, .T. ) ;
#25750 = ORIENTED_EDGE ( 'NONE', *, *, #5599, .F. ) ;
#25751 = EDGE_CURVE ( 'NONE', #28131, #16520, #43622, .T. ) ;
#25752 = VERTEX_POINT ( 'NONE', #39956 ) ;
#25753 = VECTOR ( 'NONE', #8355, 1000.000000000000000 ) ;
#25754 = LINE ( 'NONE', #40229, #33173 ) ;
#25755 = AXIS2_PLACEMENT_3D ( 'NONE', #43493, #36128, #24876 ) ;
#25756 = EDGE_LOOP ( 'NONE', ( #3918, #20911, #23855, #36375 ) ) ;
#25757 = EDGE_CURVE ( 'NONE', #12132, #4179, #6419, .T. ) ;
#25758 = DIRECTION ( 'NONE',  ( 0.5687579148473752566, -0.8225049752423786442, 0.000000000000000000 ) ) ;
#25759 = CARTESIAN_POINT ( 'NONE',  ( 0.2222846562986464380, 0.7996808935908076288, 53.20000000000001705 ) ) ;
#25760 = CARTESIAN_POINT ( 'NONE',  ( 0.000000000000000000, -35.47612816024506088, -22.48208911017539435 ) ) ;
#25761 = EDGE_LOOP ( 'NONE', ( #1956, #26860 ) ) ;
#25762 = ADVANCED_FACE ( 'NONE', ( #17902 ), #32827, .T. ) ;
#25763 = CIRCLE ( 'NONE', #18708, 42.00000000000000000 ) ;
#25764 = DIRECTION ( 'NONE',  ( 0.000000000000000000, -0.9781476007338040235, -0.2079116908177671419 ) ) ;
#25765 = VERTEX_POINT ( 'NONE', #988 ) ;
#25766 = ORIENTED_EDGE ( 'NONE', *, *, #34535, .F. ) ;
#25767 = EDGE_CURVE ( 'NONE', #42694, #43248, #26231, .T. ) ;
#25768 = CARTESIAN_POINT ( 'NONE',  ( 10.00000000000000000, -73.73191006444582740, 14.66109333815435889 ) ) ;
#25769 = FACE_OUTER_BOUND ( 'NONE', #3512, .T. ) ;
#25770 = DIRECTION ( 'NONE',  ( -1.000000000000000000, 0.000000000000000000, 0.000000000000000000 ) ) ;
#25771 = ORIENTED_EDGE ( 'NONE', *, *, #48173, .T. ) ;
#25772 = DIRECTION ( 'NONE',  ( 0.000000000000000000, 0.000000000000000000, -1.000000000000000000 ) ) ;
#25773 = CARTESIAN_POINT ( 'NONE',  ( 0.000000000000000000, 27.13269053701132094, -25.88420570971372570 ) ) ;
#25774 = CYLINDRICAL_SURFACE ( 'NONE', #9313, 16.00000000000000000 ) ;
#25775 = CARTESIAN_POINT ( 'NONE',  ( 0.000000000000000000, 62.20884554314086046, -46.21855187248561236 ) ) ;
#25776 = EDGE_CURVE ( 'NONE', #5074, #25422, #12325, .T. ) ;
#25777 = AXIS2_PLACEMENT_3D ( 'NONE', #3900, #18813, #11501 ) ;
#25778 = DIRECTION ( 'NONE',  ( 0.000000000000000000, 0.1564344650402244019, 0.9876883405951387696 ) ) ;
#25779 = EDGE_LOOP ( 'NONE', ( #8472, #26507 ) ) ;
#25780 = AXIS2_PLACEMENT_3D ( 'NONE', #5017, #19935, #35104 ) ;
#25781 = DIRECTION ( 'NONE',  ( 0.000000000000000000, 0.000000000000000000, -1.000000000000000000 ) ) ;
#25782 = ORIENTED_EDGE ( 'NONE', *, *, #24636, .F. ) ;
#25783 = VERTEX_POINT ( 'NONE', #22552 ) ;
#25784 = ADVANCED_FACE ( 'NONE', ( #15223 ), #4199, .T. ) ;
#25785 = DIRECTION ( 'NONE',  ( 0.9730327541852497042, -0.2306669878475623159, 0.000000000000000000 ) ) ;
#25786 = VECTOR ( 'NONE', #19087, 1000.000000000000000 ) ;
#25787 = CARTESIAN_POINT ( 'NONE',  ( 0.000000000000000000, -120.0000000000000000, -5.500000000000000000 ) ) ;
#25788 = CYLINDRICAL_SURFACE ( 'NONE', #21118, 31.99999999999998579 ) ;
#25789 = DIRECTION ( 'NONE',  ( 0.000000000000000000, 0.000000000000000000, 1.000000000000000000 ) ) ;
#25790 = ORIENTED_EDGE ( 'NONE', *, *, #46609, .T. ) ;
#25791 = CARTESIAN_POINT ( 'NONE',  ( 11.99999999999999822, 68.26794271651307611, -31.47745569255064169 ) ) ;
#25792 = LINE ( 'NONE', #3042, #10359 ) ;
#25793 = EDGE_CURVE ( 'NONE', #20850, #38904, #12274, .T. ) ;
#25794 = LINE ( 'NONE', #40737, #17254 ) ;
#25795 = AXIS2_PLACEMENT_3D ( 'NONE', #8635, #19645, #38511 ) ;
#25796 = CARTESIAN_POINT ( 'NONE',  ( 0.000000000000000000, 0.000000000000000000, 0.000000000000000000 ) ) ;
#25797 = DIRECTION ( 'NONE',  ( 0.000000000000000000, 0.9723699203976756689, 0.2334453638559095823 ) ) ;
#25798 = AXIS2_PLACEMENT_3D ( 'NONE', #28914, #47746, #22051 ) ;
#25799 = DIRECTION ( 'NONE',  ( 0.000000000000000000, 0.000000000000000000, 1.000000000000000000 ) ) ;
#25801 = EDGE_CURVE ( 'NONE', #44508, #47223, #15456, .T. ) ;
#25800 = DIRECTION ( 'NONE',  ( 1.000000000000000000, 0.000000000000000000, 0.000000000000000000 ) ) ;
#25802 = FACE_OUTER_BOUND ( 'NONE', #3570, .T. ) ;
#25803 = CARTESIAN_POINT ( 'NONE',  ( 10.00000000000000000, -56.15606465355001120, 59.75363087400054951 ) ) ;
#25804 = DIRECTION ( 'NONE',  ( 0.000000000000000000, 0.000000000000000000, 1.000000000000000000 ) ) ;
#25805 = LINE ( 'NONE', #28772, #21561 ) ;
#25806 = DIRECTION ( 'NONE',  ( 0.000000000000000000, -0.9876883405951361050, -0.1564344650402419989 ) ) ;
#25807 = FACE_OUTER_BOUND ( 'NONE', #37422, .T. ) ;
#25808 = CARTESIAN_POINT ( 'NONE',  ( 10.00000000000000000, 0.000000000000000000, 0.000000000000000000 ) ) ;
#25809 = CARTESIAN_POINT ( 'NONE',  ( 11.99999999999999822, 75.16055320797057959, -18.89407956138179046 ) ) ;
#25810 = DIRECTION ( 'NONE',  ( 0.000000000000000000, 0.000000000000000000, 1.000000000000000000 ) ) ;
#25811 = ORIENTED_EDGE ( 'NONE', *, *, #11770, .T. ) ;
#25812 = ORIENTED_EDGE ( 'NONE', *, *, #5035, .T. ) ;
#25813 = AXIS2_PLACEMENT_3D ( 'NONE', #36848, #18502, #10688 ) ;
#25814 = AXIS2_PLACEMENT_3D ( 'NONE', #19500, #12432, #45722 ) ;
#25815 = ORIENTED_EDGE ( 'NONE', *, *, #9664, .F. ) ;
#25816 = AXIS2_PLACEMENT_3D ( 'NONE', #1372, #16300, #2800 ) ;
#25817 = AXIS2_PLACEMENT_3D ( 'NONE', #39155, #31347, #5624 ) ;
#25818 = VERTEX_POINT ( 'NONE', #30389 ) ;
#25819 = DIRECTION ( 'NONE',  ( 0.000000000000000000, 0.000000000000000000, 1.000000000000000000 ) ) ;
#25820 = EDGE_LOOP ( 'NONE', ( #22530, #21361, #914, #2533 ) ) ;
#25821 = VECTOR ( 'NONE', #12031, 1000.000000000000000 ) ;
#25822 = AXIS2_PLACEMENT_3D ( 'NONE', #20879, #25014, #48010 ) ;
#25823 = EDGE_CURVE ( 'NONE', #44743, #33355, #4527, .T. ) ;
#25824 = DIRECTION ( 'NONE',  ( 0.000000000000000000, 0.000000000000000000, 1.000000000000000000 ) ) ;
#25825 = CIRCLE ( 'NONE', #45372, 16.00000000000000000 ) ;
#25826 = CARTESIAN_POINT ( 'NONE',  ( 5.999999999999999112, -27.74655509720617630, -77.16300072079690153 ) ) ;
#25827 = CARTESIAN_POINT ( 'NONE',  ( 0.000000000000000000, 0.000000000000000000, 0.000000000000000000 ) ) ;
#25828 = ORIENTED_EDGE ( 'NONE', *, *, #29993, .F. ) ;
#25829 = CARTESIAN_POINT ( 'NONE',  ( 3.429551818649054340, -146.3199197248623875, -5.500000000000000000 ) ) ;
#25830 = ORIENTED_EDGE ( 'NONE', *, *, #26470, .F. ) ;
#25831 = ORIENTED_EDGE ( 'NONE', *, *, #30969, .T. ) ;
#25832 = ORIENTED_EDGE ( 'NONE', *, *, #17370, .T. ) ;
#25833 = CARTESIAN_POINT ( 'NONE',  ( -1.192633404626841198, -119.0902607174754451, -2.500000000000000000 ) ) ;
#25834 = DIRECTION ( 'NONE',  ( 1.000000000000000000, -0.000000000000000000, 0.000000000000000000 ) ) ;
#25835 = DIRECTION ( 'NONE',  ( 0.000000000000000000, 0.000000000000000000, 1.000000000000000000 ) ) ;
#25836 = VERTEX_POINT ( 'NONE', #37719 ) ;
#25837 = VERTEX_POINT ( 'NONE', #15685 ) ;
#25838 = ORIENTED_EDGE ( 'NONE', *, *, #45162, .F. ) ;
#25839 = CARTESIAN_POINT ( 'NONE',  ( 0.000000000000000000, -30.80686688396994910, -21.53537804866113703 ) ) ;
#25840 = ORIENTED_EDGE ( 'NONE', *, *, #4943, .T. ) ;
#25841 = EDGE_CURVE ( 'NONE', #33636, #21412, #27981, .T. ) ;
#25842 = DIRECTION ( 'NONE',  ( 0.000000000000000000, -0.3090169943749350168, -0.9510565162951576390 ) ) ;
#25843 = DIRECTION ( 'NONE',  ( -1.000000000000000000, 0.000000000000000000, 0.000000000000000000 ) ) ;
#25844 = DIRECTION ( 'NONE',  ( 0.000000000000000000, 0.3090169943749412340, 0.9510565162951556406 ) ) ;
#25845 = CYLINDRICAL_SURFACE ( 'NONE', #27653, 16.00000000000000000 ) ;
#25846 = EDGE_CURVE ( 'NONE', #21200, #10349, #3719, .T. ) ;
#25847 = CARTESIAN_POINT ( 'NONE',  ( 10.00000000000000000, 0.000000000000000000, 0.000000000000000000 ) ) ;
#25848 = DIRECTION ( 'NONE',  ( 0.000000000000000000, 0.4539904997395477482, -0.8910065241883673437 ) ) ;
#25849 = CARTESIAN_POINT ( 'NONE',  ( 0.000000000000000000, -120.0000000000000000, 2.500000000000000000 ) ) ;
#25850 = CARTESIAN_POINT ( 'NONE',  ( 15.07208474345548055, -141.7963818439230010, 2.500000000000000000 ) ) ;
#25851 = VECTOR ( 'NONE', #45141, 1000.000000000000000 ) ;
#25852 = CARTESIAN_POINT ( 'NONE',  ( -10.90093335751250692, 1.782551537117168429E-15, 13.71399988598171049 ) ) ;
#25853 = ORIENTED_EDGE ( 'NONE', *, *, #13597, .F. ) ;
#25854 = VECTOR ( 'NONE', #37647, 999.9999999999998863 ) ;
#25856 = ADVANCED_FACE ( 'NONE', ( #34276 ), #23032, .T. ) ;
#25855 = CARTESIAN_POINT ( 'NONE',  ( 10.00000000000000000, 0.6853352020795618893, -37.58145647212453611 ) ) ;
#25857 = ORIENTED_EDGE ( 'NONE', *, *, #20953, .T. ) ;
#25858 = CIRCLE ( 'NONE', #1631, 77.49899999999999523 ) ;
#25859 = AXIS2_PLACEMENT_3D ( 'NONE', #30317, #11951, #18563 ) ;
#25860 = DIRECTION ( 'NONE',  ( 1.000000000000000000, 0.000000000000000000, 0.000000000000000000 ) ) ;
#25861 = EDGE_CURVE ( 'NONE', #1613, #22152, #19112, .T. ) ;
#25862 = FACE_OUTER_BOUND ( 'NONE', #24237, .T. ) ;
#25863 = DIRECTION ( 'NONE',  ( -1.000000000000000000, -0.000000000000000000, 0.000000000000000000 ) ) ;
#25864 = VECTOR ( 'NONE', #9787, 1000.000000000000114 ) ;
#25865 = VERTEX_POINT ( 'NONE', #45803 ) ;
#25866 = DIRECTION ( 'NONE',  ( -1.000000000000000000, -0.000000000000000000, 0.000000000000000000 ) ) ;
#25867 = AXIS2_PLACEMENT_3D ( 'NONE', #37489, #34773, #38715 ) ;
#25868 = CYLINDRICAL_SURFACE ( 'NONE', #45947, 12.50000000000000000 ) ;
#25869 = ORIENTED_EDGE ( 'NONE', *, *, #15046, .F. ) ;
#25870 = PLANE ( 'NONE',  #13815 ) ;
#25871 = VECTOR ( 'NONE', #19048, 1000.000000000000000 ) ;
#25872 = FACE_OUTER_BOUND ( 'NONE', #37485, .T. ) ;
#25873 = EDGE_CURVE ( 'NONE', #773, #697, #43589, .T. ) ;
#25874 = DIRECTION ( 'NONE',  ( 0.1850432970638656860, -0.9827303690289285187, 0.000000000000000000 ) ) ;
#25875 = SURFACE_STYLE_USAGE ( .BOTH. , #10478 ) ;
#25876 = FACE_OUTER_BOUND ( 'NONE', #4545, .T. ) ;
#25877 = ORIENTED_EDGE ( 'NONE', *, *, #35756, .F. ) ;
#25878 = ORIENTED_EDGE ( 'NONE', *, *, #40898, .T. ) ;
#25879 = EDGE_LOOP ( 'NONE', ( #27842, #36323, #10341, #45719 ) ) ;
#25880 = CARTESIAN_POINT ( 'NONE',  ( 0.000000000000000000, 34.94270380257741238, -74.18225833017852722 ) ) ;
#25881 = CARTESIAN_POINT ( 'NONE',  ( 11.99999999999999822, 0.000000000000000000, 0.000000000000000000 ) ) ;
#25882 = ORIENTED_EDGE ( 'NONE', *, *, #41080, .F. ) ;
#25883 = ORIENTED_EDGE ( 'NONE', *, *, #12286, .F. ) ;
#25884 = VECTOR ( 'NONE', #14012, 1000.000000000000000 ) ;
#25885 = EDGE_CURVE ( 'NONE', #13231, #37836, #30619, .T. ) ;
#25886 = AXIS2_PLACEMENT_3D ( 'NONE', #25543, #3028, #21149 ) ;
#25887 = DIRECTION ( 'NONE',  ( -1.000000000000000000, 0.000000000000000000, 0.000000000000000000 ) ) ;
#25888 = VECTOR ( 'NONE', #32305, 1000.000000000000000 ) ;
#25889 = AXIS2_PLACEMENT_3D ( 'NONE', #27128, #38873, #1167 ) ;
#25890 = EDGE_CURVE ( 'NONE', #44445, #47105, #34985, .T. ) ;
#25891 = ORIENTED_EDGE ( 'NONE', *, *, #2072, .T. ) ;
#25892 = ORIENTED_EDGE ( 'NONE', *, *, #10737, .F. ) ;
#25893 = EDGE_CURVE ( 'NONE', #7880, #20655, #41256, .T. ) ;
#25894 = VECTOR ( 'NONE', #28815, 1000.000000000000000 ) ;
#25895 = DIRECTION ( 'NONE',  ( 0.000000000000000000, -1.000000000000000000, -1.040834085586084730E-14 ) ) ;
#25896 = VERTEX_POINT ( 'NONE', #41172 ) ;
#25897 = CARTESIAN_POINT ( 'NONE',  ( -12.50000000000000000, -120.0000000000000000, 40.00000000000000711 ) ) ;
#25898 = CIRCLE ( 'NONE', #32177, 77.49899999999999523 ) ;
#25899 = VERTEX_POINT ( 'NONE', #30877 ) ;
#25900 = VERTEX_POINT ( 'NONE', #27198 ) ;
#25901 = DIRECTION ( 'NONE',  ( 0.000000000000000000, 0.000000000000000000, 1.000000000000000000 ) ) ;
#25902 = CIRCLE ( 'NONE', #31450, 82.00000000000000000 ) ;
#25903 = CYLINDRICAL_SURFACE ( 'NONE', #48104, 77.49899999999999523 ) ;
#25904 = EDGE_CURVE ( 'NONE', #11527, #26816, #8573, .T. ) ;
#25905 = FACE_OUTER_BOUND ( 'NONE', #12804, .T. ) ;
#25906 = ORIENTED_EDGE ( 'NONE', *, *, #13333, .F. ) ;
#25907 = EDGE_CURVE ( 'NONE', #45279, #32185, #3953, .T. ) ;
#25908 = EDGE_CURVE ( 'NONE', #7802, #39726, #28670, .T. ) ;
#25909 = ORIENTED_EDGE ( 'NONE', *, *, #7636, .T. ) ;
#25910 = DIRECTION ( 'NONE',  ( -1.000000000000000000, 0.000000000000000000, 0.000000000000000000 ) ) ;
#25911 = CARTESIAN_POINT ( 'NONE',  ( -10.00000000000000000, 0.000000000000000000, 0.000000000000000000 ) ) ;
#25912 = ORIENTED_EDGE ( 'NONE', *, *, #36893, .F. ) ;
#25913 = ORIENTED_EDGE ( 'NONE', *, *, #42441, .F. ) ;
#25914 = CARTESIAN_POINT ( 'NONE',  ( 0.000000000000000000, 0.000000000000000000, 5.500000000000000000 ) ) ;
#25915 = DIRECTION ( 'NONE',  ( -1.000000000000000000, 0.000000000000000000, 0.000000000000000000 ) ) ;
#25916 = VERTEX_POINT ( 'NONE', #24478 ) ;
#25917 = CARTESIAN_POINT ( 'NONE',  ( 10.00000000000000000, 0.000000000000000000, 0.000000000000000000 ) ) ;
#25918 = PLANE ( 'NONE',  #39464 ) ;
#25919 = FACE_OUTER_BOUND ( 'NONE', #11418, .T. ) ;
#25920 = CYLINDRICAL_SURFACE ( 'NONE', #41743, 31.99999999999998579 ) ;
#25921 = CARTESIAN_POINT ( 'NONE',  ( 0.000000000000000000, 2.446882695291915554E-15, 2.500000000000016431 ) ) ;
#25922 = CARTESIAN_POINT ( 'NONE',  ( 11.99999999999999822, -68.67312586195022561, 35.91791733033451806 ) ) ;
#25923 = ADVANCED_FACE ( 'NONE', ( #12745 ), #35010, .T. ) ;
#25925 = AXIS2_PLACEMENT_3D ( 'NONE', #20321, #31613, #35507 ) ;
#25924 = CARTESIAN_POINT ( 'NONE',  ( 11.99999999999999822, 34.44570377933693806, -69.42325613327405165 ) ) ;
#25926 = AXIS2_PLACEMENT_3D ( 'NONE', #34097, #15505, #19398 ) ;
#25927 = DIRECTION ( 'NONE',  ( 0.000000000000000000, 0.000000000000000000, 1.000000000000000000 ) ) ;
#25928 = DIRECTION ( 'NONE',  ( -1.000000000000000000, 0.000000000000000000, 0.000000000000000000 ) ) ;
#25929 = ORIENTED_EDGE ( 'NONE', *, *, #20494, .F. ) ;
#25930 = AXIS2_PLACEMENT_3D ( 'NONE', #28911, #36500, #32363 ) ;
#25931 = CARTESIAN_POINT ( 'NONE',  ( 11.99999999999999822, -73.95703589263958122, -23.16143007188505010 ) ) ;
#25932 = CARTESIAN_POINT ( 'NONE',  ( 10.00000000000000000, 0.000000000000000000, 0.000000000000000000 ) ) ;
#25933 = DIRECTION ( 'NONE',  ( 0.000000000000000000, 0.000000000000000000, 1.000000000000000000 ) ) ;
#25934 = VECTOR ( 'NONE', #10155, 1000.000000000000000 ) ;
#25935 = VERTEX_POINT ( 'NONE', #29050 ) ;
#25936 = ORIENTED_EDGE ( 'NONE', *, *, #26427, .F. ) ;
#25937 = DIRECTION ( 'NONE',  ( -1.000000000000000000, -0.000000000000000000, -0.000000000000000000 ) ) ;
#25938 = VECTOR ( 'NONE', #45007, 1000.000000000000000 ) ;
#25939 = LINE ( 'NONE', #13969, #11247 ) ;
#25940 = ORIENTED_EDGE ( 'NONE', *, *, #22756, .T. ) ;
#25941 = EDGE_CURVE ( 'NONE', #19231, #3822, #47521, .T. ) ;
#25942 = LINE ( 'NONE', #11279, #4702 ) ;
#25943 = ORIENTED_EDGE ( 'NONE', *, *, #11934, .F. ) ;
#25944 = DIRECTION ( 'NONE',  ( 0.000000000000000000, 0.000000000000000000, 1.000000000000000000 ) ) ;
#25945 = EDGE_CURVE ( 'NONE', #24044, #17161, #42864, .T. ) ;
#25946 = ORIENTED_EDGE ( 'NONE', *, *, #5597, .F. ) ;
#25947 = ORIENTED_EDGE ( 'NONE', *, *, #34922, .F. ) ;
#25948 = ORIENTED_EDGE ( 'NONE', *, *, #41969, .F. ) ;
#25949 = DIRECTION ( 'NONE',  ( -1.000000000000000000, 0.000000000000000000, 0.000000000000000000 ) ) ;
#25950 = EDGE_CURVE ( 'NONE', #35793, #37523, #1251, .T. ) ;
#25951 = CIRCLE ( 'NONE', #964, 32.00000000000000000 ) ;
#25952 = CARTESIAN_POINT ( 'NONE',  ( 10.00000000000000000, 0.000000000000000000, 0.000000000000000000 ) ) ;
#25953 = VERTEX_POINT ( 'NONE', #35737 ) ;
#25954 = ORIENTED_EDGE ( 'NONE', *, *, #351, .F. ) ;
#25955 = CARTESIAN_POINT ( 'NONE',  ( 10.00000000000000000, -72.35432306680469594, -20.40083707022958848 ) ) ;
#25956 = AXIS2_PLACEMENT_3D ( 'NONE', #13222, #8564, #43079 ) ;
#25957 = ORIENTED_EDGE ( 'NONE', *, *, #35656, .T. ) ;
#25958 = DIRECTION ( 'NONE',  ( -1.000000000000000000, 0.000000000000000000, 0.000000000000000000 ) ) ;
#25959 = DIRECTION ( 'NONE',  ( -0.9038112904824853189, 0.4279312458752976833, 0.000000000000000000 ) ) ;
#25960 = AXIS2_PLACEMENT_3D ( 'NONE', #33868, #19652, #34582 ) ;
#25961 = VERTEX_POINT ( 'NONE', #16898 ) ;
#25962 = EDGE_CURVE ( 'NONE', #45908, #7240, #11583, .T. ) ;
#25963 = DIRECTION ( 'NONE',  ( -0.9730327541852497042, 0.2306669878475622604, 0.000000000000000000 ) ) ;
#25964 = CARTESIAN_POINT ( 'NONE',  ( 0.000000000000000000, 22.90783923731740401, -78.73519480814930205 ) ) ;
#25965 = ADVANCED_FACE ( 'NONE', ( #38707 ), #17128, .F. ) ;
#25966 = ORIENTED_EDGE ( 'NONE', *, *, #32986, .T. ) ;
#25968 = VERTEX_POINT ( 'NONE', #35497 ) ;
#25967 = DIRECTION ( 'NONE',  ( -1.000000000000000000, -0.000000000000000000, 0.000000000000000000 ) ) ;
#25969 = DIRECTION ( 'NONE',  ( 1.000000000000000000, -0.000000000000000000, 0.000000000000000000 ) ) ;
#25970 = ORIENTED_EDGE ( 'NONE', *, *, #3491, .F. ) ;
#25971 = LINE ( 'NONE', #10317, #25617 ) ;
#25972 = ORIENTED_EDGE ( 'NONE', *, *, #14863, .F. ) ;
#25973 = VERTEX_POINT ( 'NONE', #20084 ) ;
#25974 = PLANE ( 'NONE',  #33010 ) ;
#25975 = CARTESIAN_POINT ( 'NONE',  ( 0.000000000000000000, -22.74946021919153694, 29.81001611431000597 ) ) ;
#25976 = ORIENTED_EDGE ( 'NONE', *, *, #10501, .F. ) ;
#25977 = AXIS2_PLACEMENT_3D ( 'NONE', #29736, #48102, #14586 ) ;
#25978 = CARTESIAN_POINT ( 'NONE',  ( 0.000000000000000000, -65.59268652807237743, 36.72794159290217664 ) ) ;
#25979 = DIRECTION ( 'NONE',  ( -1.000000000000000000, 0.000000000000000000, -0.000000000000000000 ) ) ;
#25980 = LINE ( 'NONE', #41644, #21398 ) ;
#25981 = VECTOR ( 'NONE', #35923, 1000.000000000000114 ) ;
#25982 = DIRECTION ( 'NONE',  ( 0.000000000000000000, 0.000000000000000000, 1.000000000000000000 ) ) ;
#25983 = FACE_OUTER_BOUND ( 'NONE', #10904, .T. ) ;
#25984 = EDGE_CURVE ( 'NONE', #18404, #22099, #13917, .T. ) ;
#25985 = CARTESIAN_POINT ( 'NONE',  ( 10.00000000000000000, 33.00180498840072829, -17.80606268964504935 ) ) ;
#25986 = ORIENTED_EDGE ( 'NONE', *, *, #6427, .T. ) ;
#25987 = DIRECTION ( 'NONE',  ( 0.000000000000000000, 0.000000000000000000, 1.000000000000000000 ) ) ;
#25988 = CARTESIAN_POINT ( 'NONE',  ( 10.00000000000000000, 0.000000000000000000, 0.000000000000000000 ) ) ;
#25989 = DIRECTION ( 'NONE',  ( 0.000000000000000000, -0.3826834323650969427, 0.9238795325112837409 ) ) ;
#25990 = CARTESIAN_POINT ( 'NONE',  ( -11.59517495878806947, -96.12423995607481686, 5.500000000000000000 ) ) ;
#25991 = FACE_OUTER_BOUND ( 'NONE', #25761, .T. ) ;
#25992 = DIRECTION ( 'NONE',  ( 0.000000000000000000, 0.9510565162951523099, 0.3090169943749517811 ) ) ;
#25993 = CARTESIAN_POINT ( 'NONE',  ( 10.00000000000000000, 27.13269053701132094, -25.88420570971372570 ) ) ;
#25994 = DIRECTION ( 'NONE',  ( 0.000000000000000000, 0.000000000000000000, 1.000000000000000000 ) ) ;
#25995 = ORIENTED_EDGE ( 'NONE', *, *, #33257, .F. ) ;
#25996 = CIRCLE ( 'NONE', #43954, 77.49899999999999523 ) ;
#25997 = ORIENTED_EDGE ( 'NONE', *, *, #3304, .T. ) ;
#25998 = CARTESIAN_POINT ( 'NONE',  ( 4.999999999999999112, 9.188173127307294408, 40.98264845739752360 ) ) ;
#25999 = EDGE_LOOP ( 'NONE', ( #30073, #16545, #3810, #6476 ) ) ;
#26000 = DIRECTION ( 'NONE',  ( 0.000000000000000000, 0.000000000000000000, 1.000000000000000000 ) ) ;
#26001 = AXIS2_PLACEMENT_3D ( 'NONE', #18021, #6302, #25372 ) ;
#26002 = DIRECTION ( 'NONE',  ( 0.9599519036180297338, 0.2801648492229545928, -5.514559048157468323E-17 ) ) ;
#26003 = AXIS2_PLACEMENT_3D ( 'NONE', #15620, #921, #22964 ) ;
#26004 = CYLINDRICAL_SURFACE ( 'NONE', #6521, 82.00000000000000000 ) ;
#26005 = AXIS2_PLACEMENT_3D ( 'NONE', #24554, #5968, #36695 ) ;
#26006 = ORIENTED_EDGE ( 'NONE', *, *, #30462, .F. ) ;
#26007 = CIRCLE ( 'NONE', #43213, 37.49900000000000944 ) ;
#26008 = AXIS2_PLACEMENT_3D ( 'NONE', #8656, #359, #23596 ) ;
#26009 = ORIENTED_EDGE ( 'NONE', *, *, #41526, .F. ) ;
#26010 = FACE_OUTER_BOUND ( 'NONE', #24204, .T. ) ;
#26011 = EDGE_CURVE ( 'NONE', #43520, #5501, #31851, .T. ) ;
#26012 = EDGE_LOOP ( 'NONE', ( #31796, #1695, #47190, #45245 ) ) ;
#26013 = ADVANCED_FACE ( 'NONE', ( #20308 ), #39168, .T. ) ;
#26014 = LINE ( 'NONE', #40963, #38616 ) ;
#26015 = ORIENTED_EDGE ( 'NONE', *, *, #36477, .F. ) ;
#26016 = EDGE_CURVE ( 'NONE', #4066, #1962, #46524, .T. ) ;
#26017 = CARTESIAN_POINT ( 'NONE',  ( 0.000000000000000000, 35.38097989696512968, 12.42422080174651100 ) ) ;
#26019 = ORIENTED_EDGE ( 'NONE', *, *, #25150, .T. ) ;
#26018 = CYLINDRICAL_SURFACE ( 'NONE', #39480, 31.99999999999998579 ) ;
#26020 = ORIENTED_EDGE ( 'NONE', *, *, #32003, .F. ) ;
#26021 = CARTESIAN_POINT ( 'NONE',  ( 10.00000000000000000, -26.01480285779785362, -70.53064760720343429 ) ) ;
#26022 = AXIS2_PLACEMENT_3D ( 'NONE', #40474, #29447, #6930 ) ;
#26023 = ORIENTED_EDGE ( 'NONE', *, *, #16983, .T. ) ;
#26024 = CARTESIAN_POINT ( 'NONE',  ( 0.000000000000000000, 28.89263327155746097, 71.91182617369197771 ) ) ;
#26025 = DIRECTION ( 'NONE',  ( 0.000000000000000000, 0.000000000000000000, 1.000000000000000000 ) ) ;
#26026 = ADVANCED_FACE ( 'NONE', ( #12996 ), #16186, .T. ) ;
#26027 = CYLINDRICAL_SURFACE ( 'NONE', #36857, 31.99999999999998579 ) ;
#26028 = VECTOR ( 'NONE', #34785, 1000.000000000000000 ) ;
#26029 = FACE_OUTER_BOUND ( 'NONE', #9775, .T. ) ;
#26030 = ORIENTED_EDGE ( 'NONE', *, *, #22985, .T. ) ;
#26031 = DIRECTION ( 'NONE',  ( 0.000000000000000000, -0.1564344650402170744, -0.9876883405951398798 ) ) ;
#26032 = ORIENTED_EDGE ( 'NONE', *, *, #32403, .F. ) ;
#26033 = EDGE_LOOP ( 'NONE', ( #34447, #20872, #1405, #13943 ) ) ;
#26034 = EDGE_CURVE ( 'NONE', #33558, #12152, #3745, .T. ) ;
#26035 = VECTOR ( 'NONE', #21941, 1000.000000000000000 ) ;
#26036 = CARTESIAN_POINT ( 'NONE',  ( 0.000000000000000000, -50.23322058963298531, -64.81221759200398935 ) ) ;
#26037 = CIRCLE ( 'NONE', #5743, 31.99999999999998934 ) ;
#26038 = DIRECTION ( 'NONE',  ( 1.000000000000000000, 0.000000000000000000, 0.000000000000000000 ) ) ;
#26039 = VECTOR ( 'NONE', #13889, 999.9999999999998863 ) ;
#26040 = CARTESIAN_POINT ( 'NONE',  ( 3.429551818649054340, -146.3199197248623875, 5.500000000000000000 ) ) ;
#26041 = LINE ( 'NONE', #37306, #34444 ) ;
#26042 = ORIENTED_EDGE ( 'NONE', *, *, #17040, .F. ) ;
#26043 = DIRECTION ( 'NONE',  ( -1.000000000000000000, -0.000000000000000000, -0.000000000000000000 ) ) ;
#26044 = CIRCLE ( 'NONE', #24471, 32.00000000000000000 ) ;
#26045 = PLANE ( 'NONE',  #13506 ) ;
#26046 = CARTESIAN_POINT ( 'NONE',  ( 0.000000000000000000, -71.87247863392443037, 39.47590169984818687 ) ) ;
#26047 = CARTESIAN_POINT ( 'NONE',  ( 6.938893903907228378E-15, 0.000000000000000000, -15.77977592589476608 ) ) ;
#26048 = EDGE_CURVE ( 'NONE', #15657, #31375, #45201, .T. ) ;
#26049 = CYLINDRICAL_SURFACE ( 'NONE', #24663, 30.50000000000000000 ) ;
#26050 = CIRCLE ( 'NONE', #41674, 15.99999999999999822 ) ;
#26051 = DIRECTION ( 'NONE',  ( 0.000000000000000000, 0.000000000000000000, -1.000000000000000000 ) ) ;
#26052 = ORIENTED_EDGE ( 'NONE', *, *, #5534, .T. ) ;
#26053 = DIRECTION ( 'NONE',  ( -1.000000000000000000, -0.000000000000000000, 0.000000000000000000 ) ) ;
#26054 = DIRECTION ( 'NONE',  ( -1.000000000000000000, -0.000000000000000000, -0.000000000000000000 ) ) ;
#26055 = AXIS2_PLACEMENT_3D ( 'NONE', #21065, #9563, #42646 ) ;
#26056 = FACE_OUTER_BOUND ( 'NONE', #27175, .T. ) ;
#26057 = CYLINDRICAL_SURFACE ( 'NONE', #2622, 42.00000000000000000 ) ;
#26058 = AXIS2_PLACEMENT_3D ( 'NONE', #34245, #45042, #12246 ) ;
#26059 = DIRECTION ( 'NONE',  ( 0.5200609990132993854, 0.8541291221503274356, 0.000000000000000000 ) ) ;
#26060 = EDGE_CURVE ( 'NONE', #26190, #12875, #42052, .T. ) ;
#26061 = CYLINDRICAL_SURFACE ( 'NONE', #46738, 31.99999999999999289 ) ;
#26062 = DIRECTION ( 'NONE',  ( 0.000000000000000000, 0.000000000000000000, 1.000000000000000000 ) ) ;
#26063 = DIRECTION ( 'NONE',  ( 0.000000000000000000, 0.000000000000000000, 1.000000000000000000 ) ) ;
#26064 = DIRECTION ( 'NONE',  ( 0.000000000000000000, -0.3090169943749549453, 0.9510565162951511997 ) ) ;
#26065 = CARTESIAN_POINT ( 'NONE',  ( 0.000000000000000000, -2.663952781845850826, -41.91543099594819921 ) ) ;
#26066 = VERTEX_POINT ( 'NONE', #5170 ) ;
#26067 = AXIS2_PLACEMENT_3D ( 'NONE', #30105, #18096, #41364 ) ;
#26068 = EDGE_CURVE ( 'NONE', #26881, #31305, #32675, .T. ) ;
#26069 = VERTEX_POINT ( 'NONE', #13228 ) ;
#26070 = AXIS2_PLACEMENT_3D ( 'NONE', #11660, #15092, #8462 ) ;
#26071 = AXIS2_PLACEMENT_3D ( 'NONE', #47907, #40816, #7277 ) ;
#26072 = EDGE_CURVE ( 'NONE', #10055, #16517, #28151, .T. ) ;
#26073 = CARTESIAN_POINT ( 'NONE',  ( 0.000000000000000000, 67.80270845531956070, -46.11716303203111522 ) ) ;
#26074 = VERTEX_POINT ( 'NONE', #18521 ) ;
#26075 = EDGE_CURVE ( 'NONE', #43777, #13859, #3336, .T. ) ;
#26076 = AXIS2_PLACEMENT_3D ( 'NONE', #36718, #21569, #2712 ) ;
#26077 = CIRCLE ( 'NONE', #19018, 31.99999999999998934 ) ;
#26078 = DIRECTION ( 'NONE',  ( -1.000000000000000000, 0.000000000000000000, -0.000000000000000000 ) ) ;
#26079 = EDGE_CURVE ( 'NONE', #44863, #13341, #11182, .T. ) ;
#26080 = AXIS2_PLACEMENT_3D ( 'NONE', #35980, #2214, #6609 ) ;
#26081 = CARTESIAN_POINT ( 'NONE',  ( 0.000000000000000000, 64.81221759200342092, 50.23322058963371006 ) ) ;
#26082 = CIRCLE ( 'NONE', #4993, 82.00000000000000000 ) ;
#26084 = ORIENTED_EDGE ( 'NONE', *, *, #4762, .T. ) ;
#26083 = DIRECTION ( 'NONE',  ( 0.000000000000000000, 0.000000000000000000, 1.000000000000000000 ) ) ;
#26085 = VERTEX_POINT ( 'NONE', #40335 ) ;
#26086 = DIRECTION ( 'NONE',  ( -1.000000000000000000, 0.000000000000000000, 0.000000000000000000 ) ) ;
#26087 = ORIENTED_EDGE ( 'NONE', *, *, #28474, .F. ) ;
#26088 = ORIENTED_EDGE ( 'NONE', *, *, #16460, .F. ) ;
#26089 = ORIENTED_EDGE ( 'NONE', *, *, #2144, .T. ) ;
#26090 = AXIS2_PLACEMENT_3D ( 'NONE', #43129, #16228, #24050 ) ;
#26091 = DIRECTION ( 'NONE',  ( -1.000000000000000000, -0.000000000000000000, 0.000000000000000000 ) ) ;
#26092 = DIRECTION ( 'NONE',  ( -1.000000000000000000, 0.000000000000000000, -0.000000000000000000 ) ) ;
#26093 = FACE_BOUND ( 'NONE', #36314, .T. ) ;
#26094 = ORIENTED_EDGE ( 'NONE', *, *, #41897, .T. ) ;
#26095 = ORIENTED_EDGE ( 'NONE', *, *, #40843, .F. ) ;
#26096 = DIRECTION ( 'NONE',  ( 0.000000000000000000, 0.9723699203976756689, 0.2334453638559094157 ) ) ;
#26097 = EDGE_LOOP ( 'NONE', ( #24935, #11525, #39326, #4895 ) ) ;
#26098 = FACE_OUTER_BOUND ( 'NONE', #44647, .T. ) ;
#26099 = CARTESIAN_POINT ( 'NONE',  ( 10.00000000000000000, 0.000000000000000000, 0.000000000000000000 ) ) ;
#26100 = DIRECTION ( 'NONE',  ( 0.000000000000000000, 0.8660254037844432595, 0.4999999999999919509 ) ) ;
#26101 = CARTESIAN_POINT ( 'NONE',  ( 11.99999999999999822, -77.16300072079641836, -27.74655509720752633 ) ) ;
#26102 = DIRECTION ( 'NONE',  ( -1.000000000000000000, -0.000000000000000000, -0.000000000000000000 ) ) ;
#26103 = LINE ( 'NONE', #27556, #10417 ) ;
#26104 = CYLINDRICAL_SURFACE ( 'NONE', #45650, 82.00000000000000000 ) ;
#26105 = AXIS2_PLACEMENT_3D ( 'NONE', #42933, #19011, #33943 ) ;
#26106 = LINE ( 'NONE', #18748, #25103 ) ;
#26107 = CARTESIAN_POINT ( 'NONE',  ( 11.99999999999999822, 34.44570377933598593, 69.42325613327452061 ) ) ;
#26108 = ORIENTED_EDGE ( 'NONE', *, *, #10987, .F. ) ;
#26109 = FACE_OUTER_BOUND ( 'NONE', #46409, .T. ) ;
#26110 = ADVANCED_FACE ( 'NONE', ( #7015 ), #10707, .F. ) ;
#26111 = AXIS2_PLACEMENT_3D ( 'NONE', #40671, #21341, #32379 ) ;
#26112 = ORIENTED_EDGE ( 'NONE', *, *, #18778, .T. ) ;
#26113 = CYLINDRICAL_SURFACE ( 'NONE', #30989, 77.49899999999999523 ) ;
#26114 = VERTEX_POINT ( 'NONE', #7515 ) ;
#26115 = VECTOR ( 'NONE', #39734, 1000.000000000000000 ) ;
#26116 = AXIS2_PLACEMENT_3D ( 'NONE', #12389, #23627, #16535 ) ;
#26117 = CIRCLE ( 'NONE', #44067, 31.99999999999998579 ) ;
#26118 = DIRECTION ( 'NONE',  ( -1.000000000000000000, 0.000000000000000000, 0.000000000000000000 ) ) ;
#26119 = DIRECTION ( 'NONE',  ( 0.000000000000000000, -0.9723699203976789995, 0.2334453638558956490 ) ) ;
#26120 = DIRECTION ( 'NONE',  ( 0.000000000000000000, 1.000000000000000000, 3.469446951953614978E-15 ) ) ;
#26121 = CARTESIAN_POINT ( 'NONE',  ( 0.000000000000000000, -37.22597642581153821, -5.202137450156795850 ) ) ;
#26122 = DIRECTION ( 'NONE',  ( 0.000000000000000000, 0.9510565162951510887, -0.3090169943749551673 ) ) ;
#26123 = ADVANCED_FACE ( 'NONE', ( #32960 ), #30023, .T. ) ;
#26124 = ORIENTED_EDGE ( 'NONE', *, *, #6520, .F. ) ;
#26125 = AXIS2_PLACEMENT_3D ( 'NONE', #14391, #37384, #33466 ) ;
#26126 = VECTOR ( 'NONE', #47073, 1000.000000000000000 ) ;
#26127 = CARTESIAN_POINT ( 'NONE',  ( 11.99999999999999822, -26.02418014898260878, -70.52718814184285634 ) ) ;
#26128 = DIRECTION ( 'NONE',  ( -1.000000000000000000, 0.000000000000000000, -0.000000000000000000 ) ) ;
#26129 = ORIENTED_EDGE ( 'NONE', *, *, #35683, .T. ) ;
#26130 = VECTOR ( 'NONE', #22003, 1000.000000000000000 ) ;
#26131 = VECTOR ( 'NONE', #15380, 1000.000000000000227 ) ;
#26132 = DIRECTION ( 'NONE',  ( 0.000000000000000000, 0.000000000000000000, 1.000000000000000000 ) ) ;
#26133 = DIRECTION ( 'NONE',  ( 0.000000000000000000, -0.2079116908177532086, -0.9781476007338069101 ) ) ;
#26134 = CIRCLE ( 'NONE', #12858, 31.99999999999999289 ) ;
#26135 = ORIENTED_EDGE ( 'NONE', *, *, #42022, .T. ) ;
#26136 = EDGE_CURVE ( 'NONE', #13625, #12338, #33450, .T. ) ;
#26137 = ORIENTED_EDGE ( 'NONE', *, *, #41921, .F. ) ;
#26138 = CARTESIAN_POINT ( 'NONE',  ( 0.000000000000000000, -17.28742895386139722, 75.54627589209937355 ) ) ;
#26139 = EDGE_CURVE ( 'NONE', #15938, #20902, #24093, .T. ) ;
#26140 = DIRECTION ( 'NONE',  ( 0.000000000000000000, 0.9969173337331281859, -0.07845909572784168229 ) ) ;
#26141 = EDGE_LOOP ( 'NONE', ( #14207, #1983, #16819, #30635 ) ) ;
#26142 = ORIENTED_EDGE ( 'NONE', *, *, #34619, .T. ) ;
#26143 = AXIS2_PLACEMENT_3D ( 'NONE', #15229, #41407, #30157 ) ;
#26144 = EDGE_CURVE ( 'NONE', #38104, #41802, #33920, .T. ) ;
#26145 = CARTESIAN_POINT ( 'NONE',  ( 10.00000000000000000, -11.30684508768395524, 76.66974797899831628 ) ) ;
#26146 = AXIS2_PLACEMENT_3D ( 'NONE', #44441, #26078, #22165 ) ;
#26147 = ORIENTED_EDGE ( 'NONE', *, *, #31177, .F. ) ;
#26148 = EDGE_CURVE ( 'NONE', #41584, #33852, #30355, .T. ) ;
#26149 = ORIENTED_EDGE ( 'NONE', *, *, #6940, .F. ) ;
#26150 = AXIS2_PLACEMENT_3D ( 'NONE', #41942, #1037, #16464 ) ;
#26151 = DIRECTION ( 'NONE',  ( -1.000000000000000000, -0.000000000000000000, -0.000000000000000000 ) ) ;
#26152 = DIRECTION ( 'NONE',  ( 0.000000000000000000, 0.000000000000000000, -1.000000000000000000 ) ) ;
#26153 = VECTOR ( 'NONE', #9460, 1000.000000000000000 ) ;
#26154 = AXIS2_PLACEMENT_3D ( 'NONE', #16432, #9323, #43583 ) ;
#26155 = ORIENTED_EDGE ( 'NONE', *, *, #21683, .T. ) ;
#26156 = DIRECTION ( 'NONE',  ( -1.000000000000000000, 0.000000000000000000, 0.000000000000000000 ) ) ;
#26157 = ORIENTED_EDGE ( 'NONE', *, *, #43418, .F. ) ;
#26158 = CIRCLE ( 'NONE', #1141, 30.50000000000000000 ) ;
#26159 = DIRECTION ( 'NONE',  ( -1.000000000000000000, -0.000000000000000000, 0.000000000000000000 ) ) ;
#26160 = AXIS2_PLACEMENT_3D ( 'NONE', #42939, #9883, #39025 ) ;
#26161 = AXIS2_PLACEMENT_3D ( 'NONE', #48006, #29653, #3957 ) ;
#26162 = DIRECTION ( 'NONE',  ( -1.000000000000000000, 0.000000000000000000, 0.000000000000000000 ) ) ;
#26163 = CARTESIAN_POINT ( 'NONE',  ( 0.000000000000000000, 15.48615015657581750, 39.04073710021349797 ) ) ;
#26165 = VERTEX_POINT ( 'NONE', #44465 ) ;
#26164 = AXIS2_PLACEMENT_3D ( 'NONE', #7009, #30270, #45190 ) ;
#26166 = VERTEX_POINT ( 'NONE', #48376 ) ;
#26167 = EDGE_CURVE ( 'NONE', #18579, #36121, #41289, .T. ) ;
#26168 = FACE_OUTER_BOUND ( 'NONE', #8216, .T. ) ;
#26169 = CARTESIAN_POINT ( 'NONE',  ( 0.000000000000000000, 0.000000000000000000, 0.000000000000000000 ) ) ;
#26170 = VERTEX_POINT ( 'NONE', #25373 ) ;
#26171 = ORIENTED_EDGE ( 'NONE', *, *, #17025, .T. ) ;
#26172 = DIRECTION ( 'NONE',  ( 0.000000000000000000, 0.07845909572783797692, 0.9969173337331285190 ) ) ;
#26173 = ORIENTED_EDGE ( 'NONE', *, *, #42934, .F. ) ;
#26174 = DIRECTION ( 'NONE',  ( -1.000000000000000000, 0.000000000000000000, -0.000000000000000000 ) ) ;
#26175 = DIRECTION ( 'NONE',  ( 0.000000000000000000, 0.000000000000000000, -1.000000000000000000 ) ) ;
#26176 = CARTESIAN_POINT ( 'NONE',  ( 0.7195005275814480017, -121.3161758966073052, -2.500000000000000000 ) ) ;
#26177 = CARTESIAN_POINT ( 'NONE',  ( 11.99999999999999822, 0.000000000000000000, 0.000000000000000000 ) ) ;
#26178 = DIRECTION ( 'NONE',  ( -1.000000000000000000, 0.000000000000000000, 0.000000000000000000 ) ) ;
#26179 = DIRECTION ( 'NONE',  ( -0.2867529058022035837, 0.9580045777625452175, 0.000000000000000000 ) ) ;
#26180 = DIRECTION ( 'NONE',  ( 0.000000000000000000, 0.000000000000000000, 1.000000000000000000 ) ) ;
#26181 = AXIS2_PLACEMENT_3D ( 'NONE', #40740, #3537, #7459 ) ;
#26182 = DIRECTION ( 'NONE',  ( 0.000000000000000000, 0.000000000000000000, 1.000000000000000000 ) ) ;
#26183 = FACE_OUTER_BOUND ( 'NONE', #18033, .T. ) ;
#26184 = VECTOR ( 'NONE', #38768, 1000.000000000000000 ) ;
#26185 = EDGE_CURVE ( 'NONE', #18083, #5936, #20949, .T. ) ;
#26186 = PLANE ( 'NONE',  #33887 ) ;
#26187 = LINE ( 'NONE', #34002, #9763 ) ;
#26188 = EDGE_CURVE ( 'NONE', #15261, #2795, #7257, .T. ) ;
#26189 = DIRECTION ( 'NONE',  ( 0.000000000000000000, 0.000000000000000000, 1.000000000000000000 ) ) ;
#26190 = VERTEX_POINT ( 'NONE', #15350 ) ;
#26191 = CIRCLE ( 'NONE', #17583, 31.99999999999998934 ) ;
#26192 = AXIS2_PLACEMENT_3D ( 'NONE', #18819, #221, #33754 ) ;
#26193 = PRODUCT_DEFINITION_CONTEXT ( 'detailed design', #45743, 'design' ) ;
#26194 = CYLINDRICAL_SURFACE ( 'NONE', #36994, 35.50000000000000711 ) ;
#26195 = VECTOR ( 'NONE', #35377, 1000.000000000000000 ) ;
#26196 = CARTESIAN_POINT ( 'NONE',  ( 10.00000000000000000, 0.000000000000000000, 0.000000000000000000 ) ) ;
#26197 = EDGE_CURVE ( 'NONE', #34678, #3459, #12361, .T. ) ;
#26198 = CARTESIAN_POINT ( 'NONE',  ( 15.00000000000000000, 5.835314593368777558, 22.81335362449846471 ) ) ;
#26199 = AXIS2_PLACEMENT_3D ( 'NONE', #2797, #10386, #25305 ) ;
#26200 = ORIENTED_EDGE ( 'NONE', *, *, #31867, .F. ) ;
#26201 = ADVANCED_FACE ( 'NONE', ( #6789 ), #26104, .T. ) ;
#26202 = AXIS2_PLACEMENT_3D ( 'NONE', #3196, #29877, #32816 ) ;
#26203 = EDGE_CURVE ( 'NONE', #45055, #15896, #44705, .T. ) ;
#26204 = EDGE_LOOP ( 'NONE', ( #22537, #41893, #45864, #30741 ) ) ;
#26205 = FACE_OUTER_BOUND ( 'NONE', #37474, .T. ) ;
#26206 = ORIENTED_EDGE ( 'NONE', *, *, #14729, .F. ) ;
#26207 = ORIENTED_EDGE ( 'NONE', *, *, #3128, .F. ) ;
#26208 = ORIENTED_EDGE ( 'NONE', *, *, #34146, .F. ) ;
#26209 = ORIENTED_EDGE ( 'NONE', *, *, #37862, .T. ) ;
#26210 = EDGE_CURVE ( 'NONE', #28599, #17728, #15848, .T. ) ;
#26211 = ORIENTED_EDGE ( 'NONE', *, *, #16020, .T. ) ;
#26212 = LINE ( 'NONE', #11528, #44116 ) ;
#26213 = AXIS2_PLACEMENT_3D ( 'NONE', #25024, #13534, #43409 ) ;
#26214 = DIRECTION ( 'NONE',  ( 0.000000000000000000, 0.000000000000000000, 1.000000000000000000 ) ) ;
#26215 = ORIENTED_EDGE ( 'NONE', *, *, #40153, .T. ) ;
#26216 = EDGE_LOOP ( 'NONE', ( #29159, #5094, #19672, #36666 ) ) ;
#26217 = LINE ( 'NONE', #19340, #4048 ) ;
#26218 = ORIENTED_EDGE ( 'NONE', *, *, #33298, .F. ) ;
#26219 = FACE_OUTER_BOUND ( 'NONE', #19625, .T. ) ;
#26220 = DIRECTION ( 'NONE',  ( -0.4279312458753000703, -0.9038112904824842087, 0.000000000000000000 ) ) ;
#26221 = ORIENTED_EDGE ( 'NONE', *, *, #6966, .F. ) ;
#26222 = ORIENTED_EDGE ( 'NONE', *, *, #6063, .F. ) ;
#26223 = CARTESIAN_POINT ( 'NONE',  ( 10.00000000000000000, 41.81611651403861885, 3.925862922256313503 ) ) ;
#26224 = DIRECTION ( 'NONE',  ( 0.000000000000000000, 0.5877852522924797984, 0.8090169943749426773 ) ) ;
#26225 = VERTEX_POINT ( 'NONE', #40796 ) ;
#26226 = CYLINDRICAL_SURFACE ( 'NONE', #2330, 82.00000000000000000 ) ;
#26227 = DIRECTION ( 'NONE',  ( 0.000000000000000000, -0.000000000000000000, 1.000000000000000000 ) ) ;
#26228 = AXIS2_PLACEMENT_3D ( 'NONE', #15982, #38014, #30661 ) ;
#26229 = CIRCLE ( 'NONE', #31703, 77.49900000000002365 ) ;
#26230 = ORIENTED_EDGE ( 'NONE', *, *, #42708, .F. ) ;
#26231 = LINE ( 'NONE', #19353, #27171 ) ;
#26232 = VERTEX_POINT ( 'NONE', #22190 ) ;
#26233 = ORIENTED_EDGE ( 'NONE', *, *, #37250, .F. ) ;
#26234 = CARTESIAN_POINT ( 'NONE',  ( 5.000000000000002665, -22.90783923731575911, -78.73519480814978522 ) ) ;
#26235 = CARTESIAN_POINT ( 'NONE',  ( 0.000000000000000000, 70.52718814184260054, 26.02418014898334420 ) ) ;
#26236 = CARTESIAN_POINT ( 'NONE',  ( 0.000000000000000000, 0.000000000000000000, 0.000000000000000000 ) ) ;
#26237 = AXIS2_PLACEMENT_3D ( 'NONE', #33628, #3280, #18212 ) ;
#26238 = CARTESIAN_POINT ( 'NONE',  ( 10.00000000000000000, 11.30684508768452545, -76.66974797899825944 ) ) ;
#26239 = CARTESIAN_POINT ( 'NONE',  ( -3.000000000000002665, 2.527670993440137339E-15, -20.64000000000000057 ) ) ;
#26240 = CIRCLE ( 'NONE', #5138, 77.49899999999999523 ) ;
#26241 = DIRECTION ( 'NONE',  ( 1.000000000000000000, 0.000000000000000000, 0.000000000000000000 ) ) ;
#26242 = AXIS2_PLACEMENT_3D ( 'NONE', #6356, #3640, #13933 ) ;
#26244 = EDGE_CURVE ( 'NONE', #25968, #29983, #43970, .T. ) ;
#26243 = CARTESIAN_POINT ( 'NONE',  ( -3.000000000000000000, 14.60985201121729737, -18.46759930825687945 ) ) ;
#26245 = CARTESIAN_POINT ( 'NONE',  ( 12.49999999999999822, -120.0000000000000000, 125.0000000000000000 ) ) ;
#26246 = EDGE_CURVE ( 'NONE', #14664, #3154, #22444, .T. ) ;
#26247 = DIRECTION ( 'NONE',  ( -1.000000000000000000, 0.000000000000000000, 0.000000000000000000 ) ) ;
#26248 = FACE_OUTER_BOUND ( 'NONE', #34707, .T. ) ;
#26249 = DIRECTION ( 'NONE',  ( -1.000000000000000000, -0.000000000000000000, -0.000000000000000000 ) ) ;
#26250 = DIRECTION ( 'NONE',  ( 0.000000000000000000, 0.000000000000000000, 1.000000000000000000 ) ) ;
#26251 = EDGE_CURVE ( 'NONE', #19471, #40712, #16065, .T. ) ;
#26252 = VECTOR ( 'NONE', #29070, 1000.000000000000000 ) ;
#26253 = DIRECTION ( 'NONE',  ( 0.000000000000000000, 0.000000000000000000, -1.000000000000000000 ) ) ;
#26254 = DIRECTION ( 'NONE',  ( -1.000000000000000000, -0.000000000000000000, -0.000000000000000000 ) ) ;
#26255 = CARTESIAN_POINT ( 'NONE',  ( 10.00000000000000000, -30.80686688396994910, -21.53537804866113703 ) ) ;
#26256 = AXIS2_PLACEMENT_3D ( 'NONE', #5449, #30669, #45590 ) ;
#26257 = DIRECTION ( 'NONE',  ( 0.000000000000000000, 0.000000000000000000, -1.000000000000000000 ) ) ;
#26258 = EDGE_CURVE ( 'NONE', #8436, #40486, #31006, .T. ) ;
#26259 = ORIENTED_EDGE ( 'NONE', *, *, #45962, .T. ) ;
#26260 = ORIENTED_EDGE ( 'NONE', *, *, #48300, .F. ) ;
#26261 = AXIS2_PLACEMENT_3D ( 'NONE', #37733, #41649, #4215 ) ;
#26262 = LINE ( 'NONE', #775, #5863 ) ;
#26263 = ORIENTED_EDGE ( 'NONE', *, *, #4269, .F. ) ;
#26264 = DIRECTION ( 'NONE',  ( -1.000000000000000000, 0.000000000000000000, -0.000000000000000000 ) ) ;
#26265 = CARTESIAN_POINT ( 'NONE',  ( 0.000000000000000000, -120.0000000000000000, -40.00000000000001421 ) ) ;
#26266 = DIRECTION ( 'NONE',  ( 0.000000000000000000, 6.938893903907228378E-16, 1.000000000000000000 ) ) ;
#26267 = ORIENTED_EDGE ( 'NONE', *, *, #36135, .T. ) ;
#26268 = EDGE_CURVE ( 'NONE', #5700, #13430, #29235, .T. ) ;
#26269 = EDGE_CURVE ( 'NONE', #36359, #33795, #44075, .T. ) ;
#26270 = CIRCLE ( 'NONE', #24693, 16.00000000000000000 ) ;
#26271 = DIRECTION ( 'NONE',  ( -1.000000000000000000, 0.000000000000000000, -0.000000000000000000 ) ) ;
#26272 = VECTOR ( 'NONE', #18872, 1000.000000000000000 ) ;
#26273 = ORIENTED_EDGE ( 'NONE', *, *, #8061, .T. ) ;
#26274 = AXIS2_PLACEMENT_3D ( 'NONE', #10090, #24787, #39231 ) ;
#26275 = EDGE_CURVE ( 'NONE', #15797, #2768, #34638, .T. ) ;
#26276 = DIRECTION ( 'NONE',  ( -1.000000000000000000, -0.000000000000000000, 0.000000000000000000 ) ) ;
#26277 = CIRCLE ( 'NONE', #32525, 82.00000000000000000 ) ;
#26278 = DIRECTION ( 'NONE',  ( -1.000000000000000000, 0.000000000000000000, 0.000000000000000000 ) ) ;
#26279 = CARTESIAN_POINT ( 'NONE',  ( 0.000000000000000000, 0.000000000000000000, 0.000000000000000000 ) ) ;
#26280 = ORIENTED_EDGE ( 'NONE', *, *, #35909, .T. ) ;
#26281 = AXIS2_PLACEMENT_3D ( 'NONE', #2757, #6685, #10107 ) ;
#26282 = VECTOR ( 'NONE', #24532, 1000.000000000000000 ) ;
#26283 = DIRECTION ( 'NONE',  ( 0.000000000000000000, -0.5224985647159559043, 0.8526401643540879594 ) ) ;
#26284 = DIRECTION ( 'NONE',  ( -1.000000000000000000, 0.000000000000000000, 0.000000000000000000 ) ) ;
#26285 = CARTESIAN_POINT ( 'NONE',  ( 10.00000000000000000, 41.19522573413731692, 65.64334221924924861 ) ) ;
#26286 = CARTESIAN_POINT ( 'NONE',  ( 11.99999999999999822, -36.73666225445845157, -65.58780272294114866 ) ) ;
#26287 = ORIENTED_EDGE ( 'NONE', *, *, #40833, .F. ) ;
#26288 = CARTESIAN_POINT ( 'NONE',  ( 11.99999999999999822, 71.21200624218852226, -40.65526001592539984 ) ) ;
#26289 = ORIENTED_EDGE ( 'NONE', *, *, #32067, .T. ) ;
#26290 = ORIENTED_EDGE ( 'NONE', *, *, #14363, .F. ) ;
#26291 = DIRECTION ( 'NONE',  ( 0.000000000000000000, -0.8090169943749403458, -0.5877852522924830181 ) ) ;
#26292 = FACE_OUTER_BOUND ( 'NONE', #30998, .T. ) ;
#26293 = DIRECTION ( 'NONE',  ( 0.000000000000000000, 0.7071067811865487940, -0.7071067811865462405 ) ) ;
#26294 = DIRECTION ( 'NONE',  ( -1.000000000000000000, -0.000000000000000000, -0.000000000000000000 ) ) ;
#26295 = VERTEX_POINT ( 'NONE', #26591 ) ;
#26296 = CARTESIAN_POINT ( 'NONE',  ( 10.00000000000000000, -35.53030884539094103, 12.26510123303246935 ) ) ;
#26297 = CARTESIAN_POINT ( 'NONE',  ( 12.50000000000000000, -132.5000000000000000, 40.00000000000000000 ) ) ;
#26298 = CYLINDRICAL_SURFACE ( 'NONE', #31331, 77.49899999999999523 ) ;
#26299 = DIRECTION ( 'NONE',  ( -0.2079116908177527367, 0.000000000000000000, 0.9781476007338070211 ) ) ;
#26300 = CARTESIAN_POINT ( 'NONE',  ( 0.000000000000000000, -120.0000000000000000, 2.500000000000000000 ) ) ;
#26301 = AXIS2_PLACEMENT_3D ( 'NONE', #32246, #28573, #20978 ) ;
#26302 = ADVANCED_FACE ( 'NONE', ( #27557 ), #45422, .T. ) ;
#26303 = DIRECTION ( 'NONE',  ( -1.000000000000000000, 0.000000000000000000, -0.000000000000000000 ) ) ;
#26304 = DIRECTION ( 'NONE',  ( 0.000000000000000000, 0.000000000000000000, 1.000000000000000000 ) ) ;
#26305 = FACE_OUTER_BOUND ( 'NONE', #19493, .T. ) ;
#26306 = EDGE_CURVE ( 'NONE', #39373, #15331, #26786, .T. ) ;
#26307 = AXIS2_PLACEMENT_3D ( 'NONE', #13011, #32322, #42863 ) ;
#26308 = CYLINDRICAL_SURFACE ( 'NONE', #24388, 42.00000000000000000 ) ;
#26309 = LINE ( 'NONE', #47833, #45615 ) ;
#26310 = EDGE_CURVE ( 'NONE', #33751, #22836, #15571, .T. ) ;
#26311 = LINE ( 'NONE', #41003, #19212 ) ;
#26312 = CYLINDRICAL_SURFACE ( 'NONE', #5294, 31.99999999999999289 ) ;
#26313 = CYLINDRICAL_SURFACE ( 'NONE', #26925, 12.49999999999999645 ) ;
#26314 = AXIS2_PLACEMENT_3D ( 'NONE', #36158, #20995, #39123 ) ;
#26315 = CARTESIAN_POINT ( 'NONE',  ( 0.000000000000000000, 0.000000000000000000, 0.000000000000000000 ) ) ;
#26316 = LINE ( 'NONE', #44666, #36356 ) ;
#26317 = STYLED_ITEM ( 'NONE', ( #27100 ), #3572 ) ;
#26318 = CYLINDRICAL_SURFACE ( 'NONE', #25197, 31.99999999999998579 ) ;
#26319 = VERTEX_POINT ( 'NONE', #19704 ) ;
#26320 = EDGE_CURVE ( 'NONE', #12477, #41267, #26007, .T. ) ;
#26321 = ORIENTED_EDGE ( 'NONE', *, *, #30580, .T. ) ;
#26322 = ADVANCED_FACE ( 'NONE', ( #38096 ), #26829, .T. ) ;
#26323 = VECTOR ( 'NONE', #30042, 1000.000000000000000 ) ;
#26324 = ADVANCED_FACE ( 'NONE', ( #23631 ), #27322, .T. ) ;
#26325 = VERTEX_POINT ( 'NONE', #641 ) ;
#26326 = DIRECTION ( 'NONE',  ( 1.000000000000000000, 0.000000000000000000, 0.000000000000000000 ) ) ;
#26327 = VERTEX_POINT ( 'NONE', #31483 ) ;
#26328 = AXIS2_PLACEMENT_3D ( 'NONE', #30692, #4282, #34118 ) ;
#26329 = EDGE_CURVE ( 'NONE', #34476, #36248, #34893, .T. ) ;
#26330 = AXIS2_PLACEMENT_3D ( 'NONE', #10699, #18738, #7006 ) ;
#26331 = CARTESIAN_POINT ( 'NONE',  ( 10.00000000000000000, 0.000000000000000000, 0.000000000000000000 ) ) ;
#26332 = CARTESIAN_POINT ( 'NONE',  ( 10.00000000000000000, 2.946379043146343246, 75.11764819372150725 ) ) ;
#26333 = DIRECTION ( 'NONE',  ( 0.000000000000000000, 0.000000000000000000, 1.000000000000000000 ) ) ;
#26334 = EDGE_LOOP ( 'NONE', ( #21654, #33947, #32520, #47459 ) ) ;
#26335 = VECTOR ( 'NONE', #27394, 1000.000000000000000 ) ;
#26336 = CARTESIAN_POINT ( 'NONE',  ( 0.000000000000000000, -26.08949754953044220, 27.05870788708222818 ) ) ;
#26337 = VERTEX_POINT ( 'NONE', #41765 ) ;
#26338 = VERTEX_POINT ( 'NONE', #7973 ) ;
#26339 = DIRECTION ( 'NONE',  ( -1.000000000000000000, 0.000000000000000000, -0.000000000000000000 ) ) ;
#26340 = CARTESIAN_POINT ( 'NONE',  ( 0.000000000000000000, 33.00180498840046539, 17.80606268964551120 ) ) ;
#26341 = DIRECTION ( 'NONE',  ( 0.000000000000000000, 0.8526401643540897357, 0.5224985647159531288 ) ) ;
#26342 = VERTEX_POINT ( 'NONE', #19959 ) ;
#26343 = AXIS2_PLACEMENT_3D ( 'NONE', #30226, #37554, #1067 ) ;
#26344 = VERTEX_POINT ( 'NONE', #1374 ) ;
#26345 = LINE ( 'NONE', #44223, #2881 ) ;
#26346 = EDGE_LOOP ( 'NONE', ( #17735, #13288, #17575, #1581 ) ) ;
#26347 = LINE ( 'NONE', #18261, #28548 ) ;
#26348 = DIRECTION ( 'NONE',  ( -1.000000000000000000, 0.000000000000000000, -0.000000000000000000 ) ) ;
#26349 = DIRECTION ( 'NONE',  ( 0.000000000000000000, 0.000000000000000000, 1.000000000000000000 ) ) ;
#26350 = CARTESIAN_POINT ( 'NONE',  ( 10.00000000000000000, 0.000000000000000000, 0.000000000000000000 ) ) ;
#26351 = CYLINDRICAL_SURFACE ( 'NONE', #31408, 77.49899999999999523 ) ;
#26352 = CARTESIAN_POINT ( 'NONE',  ( -11.59517495878806947, -96.12423995607481686, 5.500000000000000000 ) ) ;
#26353 = CIRCLE ( 'NONE', #2892, 31.99999999999999645 ) ;
#26354 = CARTESIAN_POINT ( 'NONE',  ( 11.99999999999999822, -26.01480285779885904, 70.53064760720306481 ) ) ;
#26355 = DIRECTION ( 'NONE',  ( 1.000000000000000000, -0.000000000000000000, -0.000000000000000000 ) ) ;
#26356 = CARTESIAN_POINT ( 'NONE',  ( 0.000000000000000000, -74.65374052328644439, -8.840884882375878107 ) ) ;
#26357 = ORIENTED_EDGE ( 'NONE', *, *, #22001, .F. ) ;
#26358 = AXIS2_PLACEMENT_3D ( 'NONE', #46415, #46669, #27832 ) ;
#26359 = LINE ( 'NONE', #43986, #22018 ) ;
#26360 = ORIENTED_EDGE ( 'NONE', *, *, #27600, .T. ) ;
#26361 = ADVANCED_FACE ( 'NONE', ( #19464 ), #5290, .T. ) ;
#26362 = DIRECTION ( 'NONE',  ( -1.000000000000000000, 0.000000000000000000, 0.000000000000000000 ) ) ;
#26363 = ORIENTED_EDGE ( 'NONE', *, *, #43823, .T. ) ;
#26364 = EDGE_CURVE ( 'NONE', #23315, #6278, #15815, .T. ) ;
#26365 = DIRECTION ( 'NONE',  ( 0.000000000000000000, 0.000000000000000000, 1.000000000000000000 ) ) ;
#26366 = DIRECTION ( 'NONE',  ( 0.9966891607226785466, 0.08130631524009969413, -0.000000000000000000 ) ) ;
#26367 = LINE ( 'NONE', #7985, #15122 ) ;
#26368 = ADVANCED_FACE ( 'NONE', ( #45672 ), #12163, .T. ) ;
#26369 = ADVANCED_FACE ( 'NONE', ( #2099 ), #24843, .T. ) ;
#26370 = AXIS2_PLACEMENT_3D ( 'NONE', #10656, #3048, #39793 ) ;
#26371 = DIRECTION ( 'NONE',  ( 0.000000000000000000, 0.000000000000000000, 1.000000000000000000 ) ) ;
#26372 = DIRECTION ( 'NONE',  ( 0.000000000000000000, -0.9510565162951565288, 0.3090169943749384029 ) ) ;
#26373 = AXIS2_PLACEMENT_3D ( 'NONE', #21152, #13833, #17005 ) ;
#26374 = ORIENTED_EDGE ( 'NONE', *, *, #3265, .T. ) ;
#26375 = DIRECTION ( 'NONE',  ( -1.000000000000000000, 0.000000000000000000, 0.000000000000000000 ) ) ;
#26376 = EDGE_CURVE ( 'NONE', #239, #5723, #2556, .T. ) ;
#26377 = LINE ( 'NONE', #17808, #40979 ) ;
#26378 = EDGE_CURVE ( 'NONE', #38979, #46234, #987, .T. ) ;
#26379 = DIRECTION ( 'NONE',  ( 0.000000000000000000, 0.000000000000000000, 1.000000000000000000 ) ) ;
#26380 = SURFACE_SIDE_STYLE ('',( #45699 ) ) ;
#26381 = DIRECTION ( 'NONE',  ( 1.000000000000000000, -0.000000000000000000, -0.000000000000000000 ) ) ;
#26382 = ORIENTED_EDGE ( 'NONE', *, *, #26798, .T. ) ;
#26383 = EDGE_LOOP ( 'NONE', ( #13570, #31176, #28746, #7590 ) ) ;
#26384 = ORIENTED_EDGE ( 'NONE', *, *, #28878, .F. ) ;
#26385 = VECTOR ( 'NONE', #31025, 1000.000000000000000 ) ;
#26386 = EDGE_CURVE ( 'NONE', #46514, #5548, #28357, .T. ) ;
#26387 = EDGE_LOOP ( 'NONE', ( #3778, #19918, #18059, #11032 ) ) ;
#26388 = CARTESIAN_POINT ( 'NONE',  ( 0.000000000000000000, 0.000000000000000000, 0.000000000000000000 ) ) ;
#26389 = DIRECTION ( 'NONE',  ( 0.000000000000000000, 0.000000000000000000, -1.000000000000000000 ) ) ;
#26390 = VERTEX_POINT ( 'NONE', #6252 ) ;
#26391 = CIRCLE ( 'NONE', #16226, 77.49899999999999523 ) ;
#26392 = ORIENTED_EDGE ( 'NONE', *, *, #23585, .F. ) ;
#26393 = EDGE_CURVE ( 'NONE', #40235, #26069, #31968, .T. ) ;
#26394 = DIRECTION ( 'NONE',  ( -1.000000000000000000, -0.000000000000000000, 0.000000000000000000 ) ) ;
#26395 = VERTEX_POINT ( 'NONE', #36097 ) ;
#26396 = ORIENTED_EDGE ( 'NONE', *, *, #45885, .T. ) ;
#26397 = CYLINDRICAL_SURFACE ( 'NONE', #17800, 31.99999999999998579 ) ;
#26398 = DIRECTION ( 'NONE',  ( -1.000000000000000000, -0.000000000000000000, -0.000000000000000000 ) ) ;
#26399 = EDGE_CURVE ( 'NONE', #29561, #42467, #12068, .T. ) ;
#26400 = VECTOR ( 'NONE', #3706, 1000.000000000000000 ) ;
#26401 = LINE ( 'NONE', #7783, #8664 ) ;
#26402 = ORIENTED_EDGE ( 'NONE', *, *, #19095, .F. ) ;
#26403 = DIRECTION ( 'NONE',  ( 0.000000000000000000, 0.000000000000000000, 1.000000000000000000 ) ) ;
#26404 = VERTEX_POINT ( 'NONE', #6486 ) ;
#26405 = ORIENTED_EDGE ( 'NONE', *, *, #38248, .F. ) ;
#26406 = LINE ( 'NONE', #4127, #43150 ) ;
#26407 = VECTOR ( 'NONE', #6688, 1000.000000000000000 ) ;
#26408 = CYLINDRICAL_SURFACE ( 'NONE', #976, 31.99999999999998579 ) ;
#26409 = CARTESIAN_POINT ( 'NONE',  ( 10.00000000000000000, 62.50329211542435104, 41.76937507738811917 ) ) ;
#26410 = ORIENTED_EDGE ( 'NONE', *, *, #11999, .T. ) ;
#26411 = ORIENTED_EDGE ( 'NONE', *, *, #12310, .F. ) ;
#26413 = EDGE_CURVE ( 'NONE', #25896, #43886, #21406, .T. ) ;
#26412 = LINE ( 'NONE', #41346, #36802 ) ;
#26414 = LINE ( 'NONE', #33733, #39196 ) ;
#26415 = EDGE_LOOP ( 'NONE', ( #25409, #37531, #25943, #9285 ) ) ;
#26416 = ORIENTED_EDGE ( 'NONE', *, *, #27466, .F. ) ;
#26417 = EDGE_CURVE ( 'NONE', #27310, #21510, #46886, .T. ) ;
#26418 = DIRECTION ( 'NONE',  ( -1.000000000000000000, -0.000000000000000000, 0.000000000000000000 ) ) ;
#26419 = ORIENTED_EDGE ( 'NONE', *, *, #14591, .F. ) ;
#26420 = DIRECTION ( 'NONE',  ( 0.000000000000000000, 0.8910065241883655673, 0.4539904997395510233 ) ) ;
#26421 = DIRECTION ( 'NONE',  ( -1.000000000000000000, 0.000000000000000000, 0.000000000000000000 ) ) ;
#26422 = CYLINDRICAL_SURFACE ( 'NONE', #7103, 31.99999999999999289 ) ;
#26423 = CARTESIAN_POINT ( 'NONE',  ( 14.59956846177685996, -138.4757300459248484, 5.500000000000000000 ) ) ;
#26424 = EDGE_CURVE ( 'NONE', #17817, #15931, #1858, .T. ) ;
#26425 = CARTESIAN_POINT ( 'NONE',  ( 0.000000000000000000, 8.688484142254221609, -21.88630264137359660 ) ) ;
#26426 = FACE_OUTER_BOUND ( 'NONE', #3592, .T. ) ;
#26427 = EDGE_CURVE ( 'NONE', #17574, #32005, #28761, .T. ) ;
#26428 = CIRCLE ( 'NONE', #43606, 31.99999999999999645 ) ;
#26429 = CYLINDRICAL_SURFACE ( 'NONE', #45905, 16.00000000000000000 ) ;
#26430 = CARTESIAN_POINT ( 'NONE',  ( 11.99999999999999822, 62.50884508063427347, 41.76106447765511831 ) ) ;
#26431 = DIRECTION ( 'NONE',  ( -0.000000000000000000, 0.000000000000000000, 1.000000000000000000 ) ) ;
#26432 = EDGE_CURVE ( 'NONE', #1046, #2861, #13843, .T. ) ;
#26433 = DIRECTION ( 'NONE',  ( -0.4279312458752977388, -0.9038112904824853189, 0.000000000000000000 ) ) ;
#26434 = CARTESIAN_POINT ( 'NONE',  ( 10.00000000000000000, 12.42422080174688404, -35.38097989696498047 ) ) ;
#26435 = DIRECTION ( 'NONE',  ( 0.8774505977381978905, 0.4796670183876304283, -0.000000000000000000 ) ) ;
#26436 = ORIENTED_EDGE ( 'NONE', *, *, #4041, .T. ) ;
#26437 = VECTOR ( 'NONE', #18746, 1000.000000000000000 ) ;
#26438 = DIRECTION ( 'NONE',  ( -1.000000000000000000, -0.000000000000000000, 0.000000000000000000 ) ) ;
#26439 = VECTOR ( 'NONE', #24746, 1000.000000000000000 ) ;
#26440 = DIRECTION ( 'NONE',  ( -1.000000000000000000, -0.000000000000000000, 0.000000000000000000 ) ) ;
#26441 = DIRECTION ( 'NONE',  ( 1.000000000000000000, 0.000000000000000000, 0.000000000000000000 ) ) ;
#26442 = CIRCLE ( 'NONE', #3791, 77.49900000000000944 ) ;
#26443 = ORIENTED_EDGE ( 'NONE', *, *, #43315, .F. ) ;
#26444 = VERTEX_POINT ( 'NONE', #43686 ) ;
#26445 = DIRECTION ( 'NONE',  ( 1.000000000000000000, 0.000000000000000000, -0.000000000000000000 ) ) ;
#26446 = ORIENTED_EDGE ( 'NONE', *, *, #6239, .F. ) ;
#26447 = ORIENTED_EDGE ( 'NONE', *, *, #34839, .T. ) ;
#26448 = ORIENTED_EDGE ( 'NONE', *, *, #33590, .F. ) ;
#26449 = ORIENTED_EDGE ( 'NONE', *, *, #38304, .T. ) ;
#26450 = EDGE_LOOP ( 'NONE', ( #3670, #39668, #19315, #37696 ) ) ;
#26451 = CARTESIAN_POINT ( 'NONE',  ( -10.00000000000000000, 0.000000000000000000, 0.000000000000000000 ) ) ;
#26452 =( GEOMETRIC_REPRESENTATION_CONTEXT ( 3 ) GLOBAL_UNCERTAINTY_ASSIGNED_CONTEXT ( ( #47719 ) ) GLOBAL_UNIT_ASSIGNED_CONTEXT ( ( #4820, #34663, #37628 ) ) REPRESENTATION_CONTEXT ( 'NONE', 'WORKASPACE' ) );
#26453 = AXIS2_PLACEMENT_3D ( 'NONE', #45, #17923, #44128 ) ;
#26454 = DIRECTION ( 'NONE',  ( 0.000000000000000000, -0.5877852522924689183, -0.8090169943749504489 ) ) ;
#26455 = ORIENTED_EDGE ( 'NONE', *, *, #9596, .F. ) ;
#26456 = ORIENTED_EDGE ( 'NONE', *, *, #7215, .T. ) ;
#26457 = DIRECTION ( 'NONE',  ( 0.000000000000000000, 0.000000000000000000, 1.000000000000000000 ) ) ;
#26458 = ORIENTED_EDGE ( 'NONE', *, *, #24660, .T. ) ;
#26459 = CARTESIAN_POINT ( 'NONE',  ( 0.000000000000000000, -41.91543099594816368, -2.663952781846588014 ) ) ;
#26460 = DIRECTION ( 'NONE',  ( -1.000000000000000000, -0.000000000000000000, -0.000000000000000000 ) ) ;
#26461 = ORIENTED_EDGE ( 'NONE', *, *, #17282, .F. ) ;
#26462 = CARTESIAN_POINT ( 'NONE',  ( 10.00000000000000000, -4.992566952385247170, 37.16516213103275845 ) ) ;
#26463 = CARTESIAN_POINT ( 'NONE',  ( 10.00000000000000000, -30.84782396557233142, 21.32104025579104345 ) ) ;
#26464 = ORIENTED_EDGE ( 'NONE', *, *, #2390, .T. ) ;
#26465 = CARTESIAN_POINT ( 'NONE',  ( 0.000000000000000000, -120.0000000000000000, -2.500000000000000000 ) ) ;
#26466 = CARTESIAN_POINT ( 'NONE',  ( 15.00000000000000000, 16.83928648764945635, 16.46020748918027010 ) ) ;
#26467 = EDGE_LOOP ( 'NONE', ( #12693, #2904, #25721, #27182 ) ) ;
#26468 = CARTESIAN_POINT ( 'NONE',  ( 10.00000000000000000, 37.22597642581158084, -5.202137450156524068 ) ) ;
#26469 = EDGE_LOOP ( 'NONE', ( #43757, #48042, #7977, #12649 ) ) ;
#26470 = EDGE_CURVE ( 'NONE', #36854, #17158, #39055, .T. ) ;
#26471 = LINE ( 'NONE', #15459, #1801 ) ;
#26472 = CARTESIAN_POINT ( 'NONE',  ( 10.00000000000000000, -68.26794271651286294, 31.47745569255117104 ) ) ;
#26473 = ORIENTED_EDGE ( 'NONE', *, *, #41491, .F. ) ;
#26474 = CIRCLE ( 'NONE', #47556, 31.99999999999998579 ) ;
#26475 = CARTESIAN_POINT ( 'NONE',  ( 10.00000000000000000, -74.65491531819111515, -8.830959090343204920 ) ) ;
#26476 = CARTESIAN_POINT ( 'NONE',  ( 0.000000000000000000, 32.34446384429971033, 26.79245525562726371 ) ) ;
#26477 = CARTESIAN_POINT ( 'NONE',  ( -10.00000000000000000, 0.000000000000000000, 0.000000000000000000 ) ) ;
#26478 = CIRCLE ( 'NONE', #5371, 77.49900000000000944 ) ;
#26479 = ADVANCED_FACE ( 'NONE', ( #2804 ), #25076, .T. ) ;
#26480 = AXIS2_PLACEMENT_3D ( 'NONE', #20924, #13827, #10634 ) ;
#26481 = CARTESIAN_POINT ( 'NONE',  ( 10.00000000000000000, -30.80686688396994910, -21.53537804866113703 ) ) ;
#26482 = CYLINDRICAL_SURFACE ( 'NONE', #36060, 32.00000000000000000 ) ;
#26483 = EDGE_CURVE ( 'NONE', #23779, #36359, #17738, .T. ) ;
#26484 = CARTESIAN_POINT ( 'NONE',  ( -10.00000000000000000, 0.000000000000000000, 0.000000000000000000 ) ) ;
#26485 = LINE ( 'NONE', #45089, #8289 ) ;
#26486 = CARTESIAN_POINT ( 'NONE',  ( -3.000000000000000000, -22.67460108101774807, -6.353146135318215038 ) ) ;
#26487 = DIRECTION ( 'NONE',  ( 0.000000000000000000, 0.000000000000000000, 1.000000000000000000 ) ) ;
#26488 = DIRECTION ( 'NONE',  ( 1.000000000000000000, -0.000000000000000000, 0.000000000000000000 ) ) ;
#26489 = EDGE_CURVE ( 'NONE', #46875, #21273, #46651, .T. ) ;
#26490 = ADVANCED_FACE ( 'NONE', ( #42737 ), #2322, .F. ) ;
#26491 = CARTESIAN_POINT ( 'NONE',  ( 10.00000000000000000, -5.256550761633413060, 77.32052557432841411 ) ) ;
#26492 = DIRECTION ( 'NONE',  ( 0.000000000000000000, 0.9510565162951544194, -0.3090169943749446757 ) ) ;
#26493 = CYLINDRICAL_SURFACE ( 'NONE', #4530, 31.99999999999998579 ) ;
#26494 = DIRECTION ( 'NONE',  ( 9.814797785686868941E-17, 1.000000000000000000, -0.000000000000000000 ) ) ;
#26495 = VERTEX_POINT ( 'NONE', #17242 ) ;
#26496 = AXIS2_PLACEMENT_3D ( 'NONE', #21294, #10284, #21780 ) ;
#26497 = ORIENTED_EDGE ( 'NONE', *, *, #44143, .T. ) ;
#26498 = DIRECTION ( 'NONE',  ( -1.000000000000000000, -0.000000000000000000, -0.000000000000000000 ) ) ;
#26499 = ORIENTED_EDGE ( 'NONE', *, *, #40301, .T. ) ;
#26500 = CARTESIAN_POINT ( 'NONE',  ( 12.13205353604972991, -140.1820037904669789, -5.500000000000000000 ) ) ;
#26501 = DIRECTION ( 'NONE',  ( 0.000000000000000000, 0.000000000000000000, 1.000000000000000000 ) ) ;
#26502 = DIRECTION ( 'NONE',  ( 0.000000000000000000, 0.000000000000000000, 1.000000000000000000 ) ) ;
#26503 = ORIENTED_EDGE ( 'NONE', *, *, #46315, .T. ) ;
#26504 = CIRCLE ( 'NONE', #22583, 42.00000000000000000 ) ;
#26505 = CARTESIAN_POINT ( 'NONE',  ( 11.99999999999999822, -59.03342792756231461, -46.54456581323868392 ) ) ;
#26506 = VECTOR ( 'NONE', #40048, 1000.000000000000000 ) ;
#26507 = ORIENTED_EDGE ( 'NONE', *, *, #9739, .T. ) ;
#26508 = ORIENTED_EDGE ( 'NONE', *, *, #34535, .T. ) ;
#26509 = CIRCLE ( 'NONE', #45272, 31.99999999999999289 ) ;
#26510 = ADVANCED_FACE ( 'NONE', ( #28046 ), #9422, .T. ) ;
#26511 = ADVANCED_FACE ( 'NONE', ( #37309 ), #29714, .T. ) ;
#26512 = DIRECTION ( 'NONE',  ( 0.000000000000000000, 0.000000000000000000, 1.000000000000000000 ) ) ;
#26513 = ORIENTED_EDGE ( 'NONE', *, *, #31869, .T. ) ;
#26514 = CYLINDRICAL_SURFACE ( 'NONE', #36715, 77.49899999999999523 ) ;
#26516 = ORIENTED_EDGE ( 'NONE', *, *, #17271, .T. ) ;
#26515 = CARTESIAN_POINT ( 'NONE',  ( -1.250000000000000000, -12.36245420541525597, 0.000000000000000000 ) ) ;
#26517 = ADVANCED_FACE ( 'NONE', ( #44894 ), #18209, .T. ) ;
#26518 = VERTEX_POINT ( 'NONE', #91 ) ;
#26519 = ADVANCED_FACE ( 'NONE', ( #22615 ), #7454, .T. ) ;
#26520 = CARTESIAN_POINT ( 'NONE',  ( 12.00000000000000000, 5.835314593368470248, -22.81335362449854642 ) ) ;
#26521 = DIRECTION ( 'NONE',  ( 1.000000000000000000, 0.000000000000000000, 0.000000000000000000 ) ) ;
#26522 = CARTESIAN_POINT ( 'NONE',  ( 11.99999999999999822, 2.956366410621684260, -75.11725578898465017 ) ) ;
#26523 = DIRECTION ( 'NONE',  ( 1.000000000000000000, 0.000000000000000000, 0.000000000000000000 ) ) ;
#26524 = ORIENTED_EDGE ( 'NONE', *, *, #32101, .T. ) ;
#26525 = LINE ( 'NONE', #34326, #27957 ) ;
#26526 = ORIENTED_EDGE ( 'NONE', *, *, #22026, .T. ) ;
#26527 = ORIENTED_EDGE ( 'NONE', *, *, #32926, .F. ) ;
#26528 = CARTESIAN_POINT ( 'NONE',  ( 10.00000000000000000, 27.13269053701132094, -25.88420570971372570 ) ) ;
#26529 = CARTESIAN_POINT ( 'NONE',  ( -3.000000000000000000, 5.835314593368772229, -22.81335362449846826 ) ) ;
#26530 = DIRECTION ( 'NONE',  ( -0.000000000000000000, -0.000000000000000000, -1.000000000000000000 ) ) ;
#26531 = CARTESIAN_POINT ( 'NONE',  ( -2.981742216678212820, 0.000000000000000000, 0.000000000000000000 ) ) ;
#26532 = VERTEX_POINT ( 'NONE', #33155 ) ;
#26533 = LINE ( 'NONE', #338, #33126 ) ;
#26534 = ADVANCED_FACE ( 'NONE', ( #18693 ), #26045, .F. ) ;
#26535 = FACE_OUTER_BOUND ( 'NONE', #41485, .T. ) ;
#26536 = EDGE_CURVE ( 'NONE', #39340, #42505, #29959, .T. ) ;
#26537 = EDGE_CURVE ( 'NONE', #48195, #17387, #41746, .T. ) ;
#26538 = CARTESIAN_POINT ( 'NONE',  ( 0.000000000000000000, 0.000000000000000000, 0.000000000000000000 ) ) ;
#26539 = DIRECTION ( 'NONE',  ( 0.000000000000000000, -0.7071067811865389130, -0.7071067811865562325 ) ) ;
#26541 = AXIS2_PLACEMENT_3D ( 'NONE', #5650, #9797, #35748 ) ;
#26540 = DIRECTION ( 'NONE',  ( 1.000000000000000000, 0.000000000000000000, 0.000000000000000000 ) ) ;
#26542 = AXIS2_PLACEMENT_3D ( 'NONE', #9701, #19737, #28307 ) ;
#26543 = DIRECTION ( 'NONE',  ( -1.000000000000000000, 0.000000000000000000, -0.000000000000000000 ) ) ;
#26544 = CARTESIAN_POINT ( 'NONE',  ( -10.00000000000000000, 0.000000000000000000, 0.000000000000000000 ) ) ;
#26545 = DIRECTION ( 'NONE',  ( -1.000000000000000000, 0.000000000000000000, 0.000000000000000000 ) ) ;
#26546 = AXIS2_PLACEMENT_3D ( 'NONE', #28302, #10419, #25341 ) ;
#26547 = CARTESIAN_POINT ( 'NONE',  ( 10.00000000000000000, -55.19960302592104284, 51.03279382321070301 ) ) ;
#26548 = DIRECTION ( 'NONE',  ( -1.000000000000000000, 0.000000000000000000, 0.000000000000000000 ) ) ;
#26549 = DIRECTION ( 'NONE',  ( 0.000000000000000000, 0.000000000000000000, 1.000000000000000000 ) ) ;
#26550 = EDGE_CURVE ( 'NONE', #12857, #43286, #25792, .T. ) ;
#26551 = DIRECTION ( 'NONE',  ( 1.000000000000000000, 6.951859121168206841E-17, -0.000000000000000000 ) ) ;
#26552 = DIRECTION ( 'NONE',  ( 0.000000000000000000, -0.9969173337331271867, -0.07845909572785571273 ) ) ;
#26553 = LINE ( 'NONE', #7934, #2040 ) ;
#26554 = EDGE_LOOP ( 'NONE', ( #34193, #18378, #20418, #8088 ) ) ;
#26555 = PRODUCT_DEFINITION_SHAPE ( 'NONE', 'NONE',  #48465 ) ;
#26556 = CARTESIAN_POINT ( 'NONE',  ( 10.00000000000000000, -10.74501242461258244, -35.92658777277521409 ) ) ;
#26557 = VERTEX_POINT ( 'NONE', #40992 ) ;
#26558 = ORIENTED_EDGE ( 'NONE', *, *, #21006, .F. ) ;
#26559 = DIRECTION ( 'NONE',  ( -1.000000000000000000, 0.000000000000000000, 0.000000000000000000 ) ) ;
#26560 = ORIENTED_EDGE ( 'NONE', *, *, #45150, .T. ) ;
#26561 = AXIS2_PLACEMENT_3D ( 'NONE', #45261, #33995, #29839 ) ;
#26562 = EDGE_CURVE ( 'NONE', #27232, #20085, #33834, .T. ) ;
#26563 = CYLINDRICAL_SURFACE ( 'NONE', #22235, 77.49899999999999523 ) ;
#26564 = VECTOR ( 'NONE', #38551, 1000.000000000000000 ) ;
#26565 = CARTESIAN_POINT ( 'NONE',  ( 10.00000000000000000, -2.663952781846440576, 41.91543099594817789 ) ) ;
#26566 = DIRECTION ( 'NONE',  ( -1.000000000000000000, 0.000000000000000000, 0.000000000000000000 ) ) ;
#26568 = EDGE_CURVE ( 'NONE', #1420, #27090, #26050, .T. ) ;
#26567 = CIRCLE ( 'NONE', #36691, 31.99999999999999289 ) ;
#26569 = ORIENTED_EDGE ( 'NONE', *, *, #3709, .T. ) ;
#26570 = DIRECTION ( 'NONE',  ( 0.000000000000000000, 0.000000000000000000, 1.000000000000000000 ) ) ;
#26571 = ORIENTED_EDGE ( 'NONE', *, *, #14421, .T. ) ;
#26572 = EDGE_CURVE ( 'NONE', #19224, #23745, #15890, .T. ) ;
#26573 = ORIENTED_EDGE ( 'NONE', *, *, #46315, .F. ) ;
#26574 = AXIS2_PLACEMENT_3D ( 'NONE', #20987, #2374, #17301 ) ;
#26575 = DIRECTION ( 'NONE',  ( 0.000000000000000000, 0.000000000000000000, 1.000000000000000000 ) ) ;
#26576 = CARTESIAN_POINT ( 'NONE',  ( 0.000000000000000000, -65.64334221924882229, -41.19522573413803457 ) ) ;
#26577 = CARTESIAN_POINT ( 'NONE',  ( 10.00000000000000000, 0.000000000000000000, 0.000000000000000000 ) ) ;
#26578 = ORIENTED_EDGE ( 'NONE', *, *, #21722, .T. ) ;
#26579 = ORIENTED_EDGE ( 'NONE', *, *, #29940, .F. ) ;
#26580 = ORIENTED_EDGE ( 'NONE', *, *, #10558, .F. ) ;
#26581 = AXIS2_PLACEMENT_3D ( 'NONE', #38992, #9587, #46328 ) ;
#26582 = CARTESIAN_POINT ( 'NONE',  ( 11.99999999999999822, 73.95703589264006439, -23.16143007188350822 ) ) ;
#26583 = ORIENTED_EDGE ( 'NONE', *, *, #23519, .F. ) ;
#26584 = EDGE_CURVE ( 'NONE', #6051, #31655, #14316, .T. ) ;
#26585 = CARTESIAN_POINT ( 'NONE',  ( 10.00000000000000000, -37.22597642581161637, 5.202137450156258502 ) ) ;
#26586 = DIRECTION ( 'NONE',  ( 0.02332147558787822997, 0.9997280174009349762, 0.000000000000000000 ) ) ;
#26587 = DIRECTION ( 'NONE',  ( 0.000000000000000000, -0.8910065241883627918, -0.4539904997395568520 ) ) ;
#26588 = DIRECTION ( 'NONE',  ( -0.6064928550163511956, -0.7950889364178798102, 0.000000000000000000 ) ) ;
#26589 = DIRECTION ( 'NONE',  ( 0.000000000000000000, 0.000000000000000000, 1.000000000000000000 ) ) ;
#26590 = DIRECTION ( 'NONE',  ( 0.000000000000000000, 1.000000000000000000, 3.491481338843133750E-15 ) ) ;
#26591 = CARTESIAN_POINT ( 'NONE',  ( 0.000000000000000000, 16.00000000000000000, 2.500000000000000000 ) ) ;
#26592 = ADVANCED_FACE ( 'NONE', ( #40272 ), #21656, .T. ) ;
#26593 = ORIENTED_EDGE ( 'NONE', *, *, #20386, .T. ) ;
#26594 = EDGE_CURVE ( 'NONE', #43524, #11302, #17965, .T. ) ;
#26595 = CARTESIAN_POINT ( 'NONE',  ( 0.000000000000000000, -81.96053171279903893, 2.543863470248094227 ) ) ;
#26596 = DIRECTION ( 'NONE',  ( -1.000000000000000000, 0.000000000000000000, 0.000000000000000000 ) ) ;
#26597 = ORIENTED_EDGE ( 'NONE', *, *, #25059, .F. ) ;
#26598 = DIRECTION ( 'NONE',  ( -1.000000000000000000, 0.000000000000000000, 0.000000000000000000 ) ) ;
#26599 = VERTEX_POINT ( 'NONE', #6965 ) ;
#26600 = ORIENTED_EDGE ( 'NONE', *, *, #38815, .T. ) ;
#26601 = DIRECTION ( 'NONE',  ( -1.000000000000000000, -0.000000000000000000, 0.000000000000000000 ) ) ;
#26602 = DIRECTION ( 'NONE',  ( 0.000000000000000000, -0.5224985647159379187, -0.8526401643540989506 ) ) ;
#26603 = CARTESIAN_POINT ( 'NONE',  ( 0.000000000000000000, 10.74501242461282757, 35.92658777277515014 ) ) ;
#26604 = DIRECTION ( 'NONE',  ( -1.000000000000000000, -0.000000000000000000, -0.000000000000000000 ) ) ;
#26605 =( LENGTH_UNIT ( ) NAMED_UNIT ( * ) SI_UNIT ( .MILLI., .METRE. ) );
#26606 = DIRECTION ( 'NONE',  ( 0.000000000000000000, 0.000000000000000000, 1.000000000000000000 ) ) ;
#26607 = EDGE_CURVE ( 'NONE', #293, #10700, #15083, .T. ) ;
#26608 = AXIS2_PLACEMENT_3D ( 'NONE', #12145, #8675, #41749 ) ;
#26609 = ORIENTED_EDGE ( 'NONE', *, *, #38639, .F. ) ;
#26610 = CARTESIAN_POINT ( 'NONE',  ( -10.00000000000000000, 0.000000000000000000, 0.000000000000000000 ) ) ;
#26611 = CARTESIAN_POINT ( 'NONE',  ( 0.000000000000000000, 0.000000000000000000, 0.000000000000000000 ) ) ;
#26612 = VECTOR ( 'NONE', #20859, 1000.000000000000114 ) ;
#26613 = VECTOR ( 'NONE', #6483, 1000.000000000000000 ) ;
#26614 = AXIS2_PLACEMENT_3D ( 'NONE', #242, #34026, #26214 ) ;
#26615 = DIRECTION ( 'NONE',  ( 0.000000000000000000, -0.1564344650402381687, 0.9876883405951365491 ) ) ;
#26616 = EDGE_LOOP ( 'NONE', ( #27365, #6228, #41400, #4835 ) ) ;
#26617 = VECTOR ( 'NONE', #2744, 1000.000000000000000 ) ;
#26618 = AXIS2_PLACEMENT_3D ( 'NONE', #27436, #20552, #5166 ) ;
#26619 = ORIENTED_EDGE ( 'NONE', *, *, #18822, .F. ) ;
#26620 = CYLINDRICAL_SURFACE ( 'NONE', #19457, 16.00000000000000000 ) ;
#26621 = DIRECTION ( 'NONE',  ( -1.000000000000000000, 0.000000000000000000, 0.000000000000000000 ) ) ;
#26622 = VERTEX_POINT ( 'NONE', #3277 ) ;
#26623 = CARTESIAN_POINT ( 'NONE',  ( -3.000000000000000000, 24.81905959214261514, 9.408202855044825341 ) ) ;
#26624 = ADVANCED_FACE ( 'NONE', ( #48080 ), #14566, .T. ) ;
#26625 = ORIENTED_EDGE ( 'NONE', *, *, #4744, .F. ) ;
#26626 = ORIENTED_EDGE ( 'NONE', *, *, #24273, .T. ) ;
#26627 = EDGE_CURVE ( 'NONE', #5583, #25081, #33060, .T. ) ;
#26628 = EDGE_CURVE ( 'NONE', #40230, #28665, #3363, .T. ) ;
#26629 = DIRECTION ( 'NONE',  ( -1.000000000000000000, -0.000000000000000000, 0.000000000000000000 ) ) ;
#26631 = VERTEX_POINT ( 'NONE', #41704 ) ;
#26630 = DIRECTION ( 'NONE',  ( 0.000000000000000000, 0.000000000000000000, 1.000000000000000000 ) ) ;
#26632 = AXIS2_PLACEMENT_3D ( 'NONE', #16009, #45873, #42182 ) ;
#26633 = DIRECTION ( 'NONE',  ( -1.000000000000000000, -0.000000000000000000, -0.000000000000000000 ) ) ;
#26635 = ORIENTED_EDGE ( 'NONE', *, *, #31584, .F. ) ;
#26634 = VECTOR ( 'NONE', #18785, 1000.000000000000000 ) ;
#26636 = FACE_OUTER_BOUND ( 'NONE', #46225, .T. ) ;
#26637 = ADVANCED_FACE ( 'NONE', ( #41961 ), #8639, .F. ) ;
#26638 = ORIENTED_EDGE ( 'NONE', *, *, #22932, .T. ) ;
#26639 = VERTEX_POINT ( 'NONE', #42181 ) ;
#26640 = CARTESIAN_POINT ( 'NONE',  ( 0.000000000000000000, 76.69515212746057387, -29.01471420065480089 ) ) ;
#26641 = CIRCLE ( 'NONE', #32877, 19.21700905503013601 ) ;
#26642 = AXIS2_PLACEMENT_3D ( 'NONE', #35953, #25166, #32062 ) ;
#26643 = CARTESIAN_POINT ( 'NONE',  ( 6.938893903907228378E-15, 0.000000000000000000, 0.000000000000000000 ) ) ;
#26644 = DIRECTION ( 'NONE',  ( 0.000000000000000000, 0.000000000000000000, 1.000000000000000000 ) ) ;
#26645 = ORIENTED_EDGE ( 'NONE', *, *, #47028, .T. ) ;
#26646 =( GEOMETRIC_REPRESENTATION_CONTEXT ( 3 ) GLOBAL_UNCERTAINTY_ASSIGNED_CONTEXT ( ( #34007 ) ) GLOBAL_UNIT_ASSIGNED_CONTEXT ( ( #21796, #13975, #47733 ) ) REPRESENTATION_CONTEXT ( 'NONE', 'WORKASPACE' ) );
#26647 = ORIENTED_EDGE ( 'NONE', *, *, #8016, .T. ) ;
#26648 = ADVANCED_FACE ( 'NONE', ( #45140 ), #38272, .F. ) ;
#26649 = CIRCLE ( 'NONE', #37619, 16.00000000000000000 ) ;
#26650 = FACE_OUTER_BOUND ( 'NONE', #16631, .T. ) ;
#26651 = FACE_OUTER_BOUND ( 'NONE', #5116, .T. ) ;
#26652 = VERTEX_POINT ( 'NONE', #16253 ) ;
#26653 = VECTOR ( 'NONE', #24183, 1000.000000000000000 ) ;
#26654 = ORIENTED_EDGE ( 'NONE', *, *, #44273, .T. ) ;
#26655 = ADVANCED_FACE ( 'NONE', ( #27265 ), #12340, .T. ) ;
#26656 = DIRECTION ( 'NONE',  ( 0.000000000000000000, -0.8526401643540970632, 0.5224985647159410274 ) ) ;
#26657 = ORIENTED_EDGE ( 'NONE', *, *, #37189, .F. ) ;
#26658 = DIRECTION ( 'NONE',  ( 0.000000000000000000, 0.000000000000000000, 1.000000000000000000 ) ) ;
#26659 = FACE_OUTER_BOUND ( 'NONE', #12929, .T. ) ;
#26660 = FACE_OUTER_BOUND ( 'NONE', #7076, .T. ) ;
#26661 = LINE ( 'NONE', #26423, #13616 ) ;
#26662 = ORIENTED_EDGE ( 'NONE', *, *, #34309, .F. ) ;
#26663 = CARTESIAN_POINT ( 'NONE',  ( 0.000000000000000000, -10.96151621346514382, 35.95386929396252640 ) ) ;
#26664 = DIRECTION ( 'NONE',  ( 0.000000000000000000, 0.3826834323650840086, 0.9238795325112891810 ) ) ;
#26665 = CARTESIAN_POINT ( 'NONE',  ( 5.000000000000000000, -74.74816331893404708, -33.71516098798818462 ) ) ;
#26666 = EDGE_CURVE ( 'NONE', #39708, #45284, #24477, .T. ) ;
#26667 = DIRECTION ( 'NONE',  ( 1.000000000000000000, 0.000000000000000000, 0.000000000000000000 ) ) ;
#26668 = DIRECTION ( 'NONE',  ( 0.000000000000000000, 0.9510565162951544194, -0.3090169943749446757 ) ) ;
#26669 = ORIENTED_EDGE ( 'NONE', *, *, #38145, .F. ) ;
#26670 = DIRECTION ( 'NONE',  ( 1.000000000000000000, 0.000000000000000000, 0.000000000000000000 ) ) ;
#26671 = DIRECTION ( 'NONE',  ( -1.000000000000000000, 0.000000000000000000, 0.000000000000000000 ) ) ;
#26672 = FACE_OUTER_BOUND ( 'NONE', #28844, .T. ) ;
#26673 = ORIENTED_EDGE ( 'NONE', *, *, #14405, .T. ) ;
#26674 = AXIS2_PLACEMENT_3D ( 'NONE', #30401, #46053, #19586 ) ;
#26675 = ADVANCED_FACE ( 'NONE', ( #22854 ), #11609, .T. ) ;
#26676 = AXIS2_PLACEMENT_3D ( 'NONE', #21643, #28976, #29468 ) ;
#26677 = UNCERTAINTY_MEASURE_WITH_UNIT (LENGTH_MEASURE( 1.000000000000000082E-05 ), #2630, 'distance_accuracy_value', 'NONE');
#26678 = DIRECTION ( 'NONE',  ( -1.000000000000000000, -0.000000000000000000, 0.000000000000000000 ) ) ;
#26679 = CIRCLE ( 'NONE', #39993, 31.99999999999998579 ) ;
#26680 = CARTESIAN_POINT ( 'NONE',  ( -3.000000000000000000, -18.13022148937243472, -15.02647892043568767 ) ) ;
#26681 = DIRECTION ( 'NONE',  ( -1.000000000000000000, 0.000000000000000000, -0.000000000000000000 ) ) ;
#26682 = VERTEX_POINT ( 'NONE', #38040 ) ;
#26683 = AXIS2_PLACEMENT_3D ( 'NONE', #33985, #4135, #7568 ) ;
#26684 = ORIENTED_EDGE ( 'NONE', *, *, #21709, .F. ) ;
#26685 = ADVANCED_FACE ( 'NONE', ( #26535 ), #4738, .T. ) ;
#26686 = CARTESIAN_POINT ( 'NONE',  ( 0.000000000000000000, 6.903761155838878061, -77.19088730480517313 ) ) ;
#26687 = EDGE_CURVE ( 'NONE', #15060, #34442, #8412, .T. ) ;
#26688 = ORIENTED_EDGE ( 'NONE', *, *, #13649, .F. ) ;
#26689 = EDGE_LOOP ( 'NONE', ( #40496, #1984, #26593, #22871 ) ) ;
#26690 = ORIENTED_EDGE ( 'NONE', *, *, #39586, .T. ) ;
#26691 = EDGE_CURVE ( 'NONE', #26325, #37458, #30686, .T. ) ;
#26692 = AXIS2_PLACEMENT_3D ( 'NONE', #11326, #38662, #41188 ) ;
#26693 = DIRECTION ( 'NONE',  ( 0.000000000000000000, -1.776356839400250465E-15, -1.000000000000000000 ) ) ;
#26694 = ORIENTED_EDGE ( 'NONE', *, *, #26079, .T. ) ;
#26695 = ORIENTED_EDGE ( 'NONE', *, *, #23214, .F. ) ;
#26696 = EDGE_CURVE ( 'NONE', #36602, #3853, #18973, .T. ) ;
#26697 = ORIENTED_EDGE ( 'NONE', *, *, #27987, .T. ) ;
#26698 = DIRECTION ( 'NONE',  ( 1.000000000000000000, 0.000000000000000000, -0.000000000000000000 ) ) ;
#26699 = EDGE_LOOP ( 'NONE', ( #19401, #36969, #5646, #24679 ) ) ;
#26700 = DIRECTION ( 'NONE',  ( 0.000000000000000000, 0.000000000000000000, 1.000000000000000000 ) ) ;
#26701 = CARTESIAN_POINT ( 'NONE',  ( -18.24502636017238899, -100.7225776329765665, -5.500000000000000000 ) ) ;
#26702 = ORIENTED_EDGE ( 'NONE', *, *, #33033, .T. ) ;
#26703 = DIRECTION ( 'NONE',  ( 0.000000000000000000, 0.000000000000000000, 1.000000000000000000 ) ) ;
#26704 = ORIENTED_EDGE ( 'NONE', *, *, #46092, .F. ) ;
#26705 = CIRCLE ( 'NONE', #15772, 31.99999999999998934 ) ;
#26706 = CARTESIAN_POINT ( 'NONE',  ( 4.999999999999999112, 36.13751322684449008, -21.40280677340332716 ) ) ;
#26707 = LINE ( 'NONE', #18390, #12574 ) ;
#26708 = EDGE_LOOP ( 'NONE', ( #24837, #43028 ) ) ;
#26709 = AXIS2_PLACEMENT_3D ( 'NONE', #33609, #30670, #8155 ) ;
#26710 = DIRECTION ( 'NONE',  ( 0.000000000000000000, -0.5877852522924625900, -0.8090169943749551118 ) ) ;
#26711 = ORIENTED_EDGE ( 'NONE', *, *, #44315, .T. ) ;
#26712 = ORIENTED_EDGE ( 'NONE', *, *, #42968, .F. ) ;
#26713 = DIRECTION ( 'NONE',  ( -1.000000000000000000, 0.000000000000000000, -0.000000000000000000 ) ) ;
#26714 = CARTESIAN_POINT ( 'NONE',  ( 10.00000000000000000, 44.99326035066149387, -68.55367621811095091 ) ) ;
#26715 = CIRCLE ( 'NONE', #29848, 82.00000000000000000 ) ;
#26716 = DIRECTION ( 'NONE',  ( 0.000000000000000000, -0.3826834323650970537, 0.9238795325112838519 ) ) ;
#26717 = FACE_OUTER_BOUND ( 'NONE', #43710, .T. ) ;
#26718 = DIRECTION ( 'NONE',  ( 0.000000000000000000, 0.000000000000000000, 1.000000000000000000 ) ) ;
#26719 = STYLED_ITEM ( 'NONE', ( #12347 ), #2931 ) ;
#26720 = LINE ( 'NONE', #23043, #25753 ) ;
#26721 = CIRCLE ( 'NONE', #15782, 82.00000000000000000 ) ;
#26722 = CARTESIAN_POINT ( 'NONE',  ( -10.00000000000000000, 0.000000000000000000, 0.000000000000000000 ) ) ;
#26723 = LINE ( 'NONE', #42135, #13804 ) ;
#26724 = ORIENTED_EDGE ( 'NONE', *, *, #19177, .F. ) ;
#26725 = DIRECTION ( 'NONE',  ( -1.000000000000000000, -0.000000000000000000, 0.000000000000000000 ) ) ;
#26726 = CARTESIAN_POINT ( 'NONE',  ( 10.00000000000000178, 2.571758278209441661E-15, -21.00000000000000000 ) ) ;
#26727 = CYLINDRICAL_SURFACE ( 'NONE', #32529, 82.00000000000000000 ) ;
#26728 = AXIS2_PLACEMENT_3D ( 'NONE', #1915, #46702, #23439 ) ;
#26729 = CARTESIAN_POINT ( 'NONE',  ( 10.00000000000000000, 2.543863470248371783, 81.96053171279901051 ) ) ;
#26730 = CARTESIAN_POINT ( 'NONE',  ( -9.937067298023317008, 7.583184918921301865, -54.99999999999999289 ) ) ;
#26731 = CYLINDRICAL_SURFACE ( 'NONE', #1427, 12.49999999999999822 ) ;
#26732 = PLANE ( 'NONE',  #35844 ) ;
#26733 = VERTEX_POINT ( 'NONE', #12573 ) ;
#26734 = ORIENTED_EDGE ( 'NONE', *, *, #37982, .F. ) ;
#26735 = CARTESIAN_POINT ( 'NONE',  ( 12.00000000000000000, -10.45096189432314127, 21.10159698893440350 ) ) ;
#26736 = EDGE_LOOP ( 'NONE', ( #4826, #27803, #43835, #48233 ) ) ;
#26737 = CARTESIAN_POINT ( 'NONE',  ( 0.000000000000000000, 0.000000000000000000, 0.000000000000000000 ) ) ;
#26738 = APPLICATION_PROTOCOL_DEFINITION ( 'draft international standard', 'automotive_design', 1998, #14148 ) ;
#26739 = CARTESIAN_POINT ( 'NONE',  ( 6.377742925735834234, -145.7647898336708181, 2.500000000000000000 ) ) ;
#26740 = ORIENTED_EDGE ( 'NONE', *, *, #667, .F. ) ;
#26741 = AXIS2_PLACEMENT_3D ( 'NONE', #17499, #32906, #44180 ) ;
#26742 = ADVANCED_FACE ( 'NONE', ( #27508 ), #8891, .T. ) ;
#26743 = VECTOR ( 'NONE', #33552, 1000.000000000000000 ) ;
#26744 = CYLINDRICAL_SURFACE ( 'NONE', #14343, 16.00000000000000000 ) ;
#26745 = VERTEX_POINT ( 'NONE', #19412 ) ;
#26746 = EDGE_CURVE ( 'NONE', #12928, #41352, #7280, .T. ) ;
#26747 = AXIS2_PLACEMENT_3D ( 'NONE', #30689, #15761, #26539 ) ;
#26748 = DIRECTION ( 'NONE',  ( -0.9918136447140104561, 0.1276937514489679681, 0.000000000000000000 ) ) ;
#26749 = EDGE_CURVE ( 'NONE', #45907, #39835, #47910, .T. ) ;
#26750 = CARTESIAN_POINT ( 'NONE',  ( 11.99999999999999822, 6.903761155838878061, -77.19088730480517313 ) ) ;
#26752 = ORIENTED_EDGE ( 'NONE', *, *, #4595, .T. ) ;
#26751 = LINE ( 'NONE', #27239, #45764 ) ;
#26753 = ORIENTED_EDGE ( 'NONE', *, *, #15985, .T. ) ;
#26754 = ADVANCED_FACE ( 'NONE', ( #26770 ), #34336, .T. ) ;
#26755 = ORIENTED_EDGE ( 'NONE', *, *, #33571, .F. ) ;
#26756 = CYLINDRICAL_SURFACE ( 'NONE', #14410, 37.49900000000000233 ) ;
#26757 = DIRECTION ( 'NONE',  ( 0.000000000000000000, 0.9510565162951544194, -0.3090169943749446757 ) ) ;
#26758 = DIRECTION ( 'NONE',  ( 0.000000000000000000, 0.1045284632676449221, -0.9945218953682741780 ) ) ;
#26759 = CARTESIAN_POINT ( 'NONE',  ( -42.50000000000000000, 0.000000000000000000, 0.000000000000000000 ) ) ;
#26760 = ORIENTED_EDGE ( 'NONE', *, *, #26034, .T. ) ;
#26761 = CARTESIAN_POINT ( 'NONE',  ( 0.000000000000000000, 0.000000000000000000, 0.000000000000000000 ) ) ;
#26762 = ORIENTED_EDGE ( 'NONE', *, *, #37012, .T. ) ;
#26763 = EDGE_LOOP ( 'NONE', ( #2122, #24631, #46709, #9672 ) ) ;
#26764 = CARTESIAN_POINT ( 'NONE',  ( 0.000000000000000000, -12.26510123303234501, -35.53030884539098366 ) ) ;
#26765 = CARTESIAN_POINT ( 'NONE',  ( 0.000000000000000000, 6.555932627142952995, -37.01155633439051940 ) ) ;
#26766 = DIRECTION ( 'NONE',  ( -1.000000000000000000, 0.000000000000000000, 0.000000000000000000 ) ) ;
#26767 = DIRECTION ( 'NONE',  ( 1.000000000000000000, -0.000000000000000000, -0.000000000000000000 ) ) ;
#26768 = ORIENTED_EDGE ( 'NONE', *, *, #43863, .T. ) ;
#26769 = DIRECTION ( 'NONE',  ( 0.000000000000000000, 0.6494480483301848794, -0.7604059656000299317 ) ) ;
#26770 = FACE_OUTER_BOUND ( 'NONE', #2876, .T. ) ;
#26771 = ADVANCED_FACE ( 'NONE', ( #16964 ), #28711, .T. ) ;
#26772 = CARTESIAN_POINT ( 'NONE',  ( 12.00000000000000000, 16.83928648764945635, 16.46020748918027010 ) ) ;
#26773 = VECTOR ( 'NONE', #8647, 1000.000000000000000 ) ;
#26774 = CARTESIAN_POINT ( 'NONE',  ( 10.00000000000000000, -75.16055320797016748, -18.89407956138335365 ) ) ;
#26775 = DIRECTION ( 'NONE',  ( 1.000000000000000000, 0.000000000000000000, 0.000000000000000000 ) ) ;
#26776 = DIRECTION ( 'NONE',  ( 1.000000000000000000, -0.000000000000000000, 0.000000000000000000 ) ) ;
#26777 = CYLINDRICAL_SURFACE ( 'NONE', #33380, 42.00000000000000000 ) ;
#26778 = DIRECTION ( 'NONE',  ( -1.000000000000000000, 0.000000000000000000, 0.000000000000000000 ) ) ;
#26779 = AXIS2_PLACEMENT_3D ( 'NONE', #13935, #28855, #48188 ) ;
#26780 = CARTESIAN_POINT ( 'NONE',  ( 11.99999999999999822, -75.16055320797043748, 18.89407956138231270 ) ) ;
#26781 = DIRECTION ( 'NONE',  ( 0.000000000000000000, 0.000000000000000000, 1.000000000000000000 ) ) ;
#26782 = CARTESIAN_POINT ( 'NONE',  ( 11.99999999999999822, -74.65491531819111515, -8.830959090343204920 ) ) ;
#26783 = EDGE_CURVE ( 'NONE', #45354, #7708, #16653, .T. ) ;
#26784 = DIRECTION ( 'NONE',  ( -1.000000000000000000, -0.000000000000000000, 0.000000000000000000 ) ) ;
#26785 = DIRECTION ( 'NONE',  ( -1.000000000000000000, -0.000000000000000000, 0.000000000000000000 ) ) ;
#26786 = CIRCLE ( 'NONE', #11169, 82.00000000000000000 ) ;
#26787 = DIRECTION ( 'NONE',  ( -1.000000000000000000, -0.000000000000000000, -0.000000000000000000 ) ) ;
#26788 = ORIENTED_EDGE ( 'NONE', *, *, #42517, .F. ) ;
#26789 = AXIS2_PLACEMENT_3D ( 'NONE', #3060, #18713, #29502 ) ;
#26790 = EDGE_CURVE ( 'NONE', #43952, #19231, #9140, .T. ) ;
#26791 = EDGE_CURVE ( 'NONE', #16717, #38747, #20554, .T. ) ;
#26792 = LINE ( 'NONE', #4042, #32280 ) ;
#26793 = VERTEX_POINT ( 'NONE', #35318 ) ;
#26794 = ORIENTED_EDGE ( 'NONE', *, *, #2758, .T. ) ;
#26795 = VERTEX_POINT ( 'NONE', #39239 ) ;
#26796 = CARTESIAN_POINT ( 'NONE',  ( 0.000000000000000000, 0.000000000000000000, 0.000000000000000000 ) ) ;
#26797 = AXIS2_PLACEMENT_3D ( 'NONE', #7164, #22086, #37020 ) ;
#26798 = EDGE_CURVE ( 'NONE', #38628, #19539, #5966, .T. ) ;
#26799 = VERTEX_POINT ( 'NONE', #31679 ) ;
#26800 = EDGE_CURVE ( 'NONE', #2137, #28615, #42445, .T. ) ;
#26801 = ADVANCED_FACE ( 'NONE', ( #5707 ), #39494, .T. ) ;
#26802 = CIRCLE ( 'NONE', #1012, 77.49899999999999523 ) ;
#26803 = AXIS2_PLACEMENT_3D ( 'NONE', #35500, #28389, #2209 ) ;
#26804 = DIRECTION ( 'NONE',  ( -1.000000000000000000, -0.000000000000000000, 0.000000000000000000 ) ) ;
#26805 = CARTESIAN_POINT ( 'NONE',  ( 5.000000000000002665, -81.96053171279901051, -2.543863470249246195 ) ) ;
#26806 = AXIS2_PLACEMENT_3D ( 'NONE', #23882, #31240, #5520 ) ;
#26807 = LINE ( 'NONE', #38076, #20662 ) ;
#26808 = VERTEX_POINT ( 'NONE', #24076 ) ;
#26809 = CARTESIAN_POINT ( 'NONE',  ( 0.000000000000000000, 8.688484142253939169, 21.88630264137371029 ) ) ;
#26810 = ORIENTED_EDGE ( 'NONE', *, *, #8949, .F. ) ;
#26811 = AXIS2_PLACEMENT_3D ( 'NONE', #35697, #46952, #36161 ) ;
#26812 = EDGE_LOOP ( 'NONE', ( #47679, #10262, #15146, #25594 ) ) ;
#26813 = VERTEX_POINT ( 'NONE', #35807 ) ;
#26814 = DIRECTION ( 'NONE',  ( 0.9997280174009348652, -0.02332147558787931590, 0.000000000000000000 ) ) ;
#26815 = DIRECTION ( 'NONE',  ( -1.000000000000000000, -0.000000000000000000, -0.000000000000000000 ) ) ;
#26816 = VERTEX_POINT ( 'NONE', #2268 ) ;
#26817 = VECTOR ( 'NONE', #9859, 1000.000000000000000 ) ;
#26818 = ORIENTED_EDGE ( 'NONE', *, *, #24883, .F. ) ;
#26819 = ORIENTED_EDGE ( 'NONE', *, *, #17855, .T. ) ;
#26820 = CARTESIAN_POINT ( 'NONE',  ( 0.000000000000000000, -51.02545421589363883, 55.20638768913742922 ) ) ;
#26821 = VERTEX_POINT ( 'NONE', #32385 ) ;
#26822 = CARTESIAN_POINT ( 'NONE',  ( 5.000000000000002665, 29.01471420065674423, -76.69515212745984911 ) ) ;
#26823 = CIRCLE ( 'NONE', #23672, 11.59999999999999964 ) ;
#26824 = CARTESIAN_POINT ( 'NONE',  ( 10.00000000000000000, -22.64427369931148348, -30.00120703465229965 ) ) ;
#26825 = CARTESIAN_POINT ( 'NONE',  ( 10.00000000000000000, -67.80270845531921964, 46.11716303203163392 ) ) ;
#26826 = DIRECTION ( 'NONE',  ( 1.000000000000000000, 0.000000000000000000, 0.000000000000000000 ) ) ;
#26827 = DIRECTION ( 'NONE',  ( -1.000000000000000000, -0.000000000000000000, 0.000000000000000000 ) ) ;
#26828 = FACE_OUTER_BOUND ( 'NONE', #26387, .T. ) ;
#26829 = CYLINDRICAL_SURFACE ( 'NONE', #3325, 77.49899999999999523 ) ;
#26830 = CARTESIAN_POINT ( 'NONE',  ( 10.00000000000000000, -36.88895765772628010, -6.736453364083947015 ) ) ;
#26831 = DIRECTION ( 'NONE',  ( 0.000000000000000000, 0.000000000000000000, 1.000000000000000000 ) ) ;
#26832 = ORIENTED_EDGE ( 'NONE', *, *, #23197, .F. ) ;
#26833 = DIRECTION ( 'NONE',  ( -1.000000000000000000, -0.000000000000000000, 0.000000000000000000 ) ) ;
#26834 = CARTESIAN_POINT ( 'NONE',  ( 10.00000000000000000, -37.58145647212455032, 16.68533520207890319 ) ) ;
#26835 = ORIENTED_EDGE ( 'NONE', *, *, #35476, .F. ) ;
#26836 = EDGE_LOOP ( 'NONE', ( #29654, #19489, #43518, #32171 ) ) ;
#26837 = CARTESIAN_POINT ( 'NONE',  ( 10.00000000000000000, 37.01155633439059756, 6.555932627142549762 ) ) ;
#26838 = DIRECTION ( 'NONE',  ( 0.000000000000000000, 0.4539904997395479702, -0.8910065241883673437 ) ) ;
#26839 = CARTESIAN_POINT ( 'NONE',  ( 30.50000000000000000, -120.0000000000000000, -5.500000000000000000 ) ) ;
#26840 = CARTESIAN_POINT ( 'NONE',  ( 0.000000000000000000, 62.20884554314020676, 46.21855187248652896 ) ) ;
#26841 = EDGE_CURVE ( 'NONE', #16242, #975, #5463, .T. ) ;
#26842 = DIRECTION ( 'NONE',  ( 0.3090169943749573878, -0.9510565162951503115, 0.000000000000000000 ) ) ;
#26844 = AXIS2_PLACEMENT_3D ( 'NONE', #29607, #29849, #22014 ) ;
#26843 = LINE ( 'NONE', #30038, #38895 ) ;
#26845 = EDGE_CURVE ( 'NONE', #38558, #23222, #36968, .T. ) ;
#26846 = FACE_OUTER_BOUND ( 'NONE', #26216, .T. ) ;
#26847 = CARTESIAN_POINT ( 'NONE',  ( 10.00000000000000000, 0.000000000000000000, 0.000000000000000000 ) ) ;
#26848 = VECTOR ( 'NONE', #9970, 1000.000000000000000 ) ;
#26849 = AXIS2_PLACEMENT_3D ( 'NONE', #7850, #22780, #31059 ) ;
#26850 = VECTOR ( 'NONE', #39201, 1000.000000000000000 ) ;
#26851 = EDGE_CURVE ( 'NONE', #32445, #1298, #20380, .T. ) ;
#26852 = CIRCLE ( 'NONE', #35442, 31.99999999999999289 ) ;
#26853 = ORIENTED_EDGE ( 'NONE', *, *, #10498, .T. ) ;
#26854 = ADVANCED_FACE ( 'NONE', ( #21100 ), #35077, .T. ) ;
#26855 = AXIS2_PLACEMENT_3D ( 'NONE', #8708, #16312, #27095 ) ;
#26856 = CARTESIAN_POINT ( 'NONE',  ( 0.000000000000000000, 36.13751322684419165, 21.40280677340384585 ) ) ;
#26857 = ORIENTED_EDGE ( 'NONE', *, *, #4576, .F. ) ;
#26858 = VECTOR ( 'NONE', #34591, 1000.000000000000000 ) ;
#26859 = CIRCLE ( 'NONE', #24514, 82.00000000000000000 ) ;
#26860 = ORIENTED_EDGE ( 'NONE', *, *, #46361, .F. ) ;
#26861 = EDGE_CURVE ( 'NONE', #21976, #33652, #29964, .T. ) ;
#26862 = AXIS2_PLACEMENT_3D ( 'NONE', #22824, #4237, #19148 ) ;
#26863 = ORIENTED_EDGE ( 'NONE', *, *, #18522, .F. ) ;
#26864 = LINE ( 'NONE', #14884, #31234 ) ;
#26865 = FACE_OUTER_BOUND ( 'NONE', #14409, .T. ) ;
#26866 = ORIENTED_EDGE ( 'NONE', *, *, #33218, .T. ) ;
#26867 = CIRCLE ( 'NONE', #22946, 37.49900000000000944 ) ;
#26868 = ADVANCED_FACE ( 'NONE', ( #47313 ), #20630, .T. ) ;
#26869 = EDGE_CURVE ( 'NONE', #26327, #30863, #42919, .T. ) ;
#26870 = VERTEX_POINT ( 'NONE', #36039 ) ;
#26871 = DIRECTION ( 'NONE',  ( -1.000000000000000000, 0.000000000000000000, 0.000000000000000000 ) ) ;
#26872 = VERTEX_POINT ( 'NONE', #43156 ) ;
#26873 = ADVANCED_BREP_SHAPE_REPRESENTATION ( '', ( #35540, #11636 ), #2952 ) ;
#26874 = EDGE_LOOP ( 'NONE', ( #4549, #40701, #19350, #10816 ) ) ;
#26875 = AXIS2_PLACEMENT_3D ( 'NONE', #22218, #3610, #25874 ) ;
#26876 = DIRECTION ( 'NONE',  ( 0.000000000000000000, 0.000000000000000000, 1.000000000000000000 ) ) ;
#26877 = EDGE_CURVE ( 'NONE', #32425, #43019, #24551, .T. ) ;
#26879 = ORIENTED_EDGE ( 'NONE', *, *, #42830, .T. ) ;
#26878 = CARTESIAN_POINT ( 'NONE',  ( 10.00000000000000000, -20.41045688087772092, -72.35160999960838524 ) ) ;
#26880 = CARTESIAN_POINT ( 'NONE',  ( 15.00000000000000000, -3.948201729842032215, 23.21447184625297666 ) ) ;
#26881 = VERTEX_POINT ( 'NONE', #12815 ) ;
#26882 = VERTEX_POINT ( 'NONE', #27759 ) ;
#26883 = FACE_OUTER_BOUND ( 'NONE', #10962, .T. ) ;
#26884 = ORIENTED_EDGE ( 'NONE', *, *, #20567, .F. ) ;
#26885 = VERTEX_POINT ( 'NONE', #25248 ) ;
#26886 = CARTESIAN_POINT ( 'NONE',  ( 10.00000000000000000, 0.000000000000000000, 0.000000000000000000 ) ) ;
#26887 = AXIS2_PLACEMENT_3D ( 'NONE', #36812, #26043, #22853 ) ;
#26888 = VECTOR ( 'NONE', #1855, 1000.000000000000000 ) ;
#26889 = CIRCLE ( 'NONE', #19846, 82.00000000000000000 ) ;
#26890 = CARTESIAN_POINT ( 'NONE',  ( 12.00000000000000000, -4.261787119644963262, 26.19803753235780164 ) ) ;
#26891 = CARTESIAN_POINT ( 'NONE',  ( -3.000000000000000000, 18.84667830672579925, 18.68964196561269020 ) ) ;
#26892 = ORIENTED_EDGE ( 'NONE', *, *, #1644, .F. ) ;
#26893 = VERTEX_POINT ( 'NONE', #32837 ) ;
#26894 = FACE_OUTER_BOUND ( 'NONE', #21689, .T. ) ;
#26895 = CARTESIAN_POINT ( 'NONE',  ( 5.000000000000000000, 2.663952781846149254, 41.91543099594818500 ) ) ;
#26896 = VECTOR ( 'NONE', #2353, 1000.000000000000000 ) ;
#26897 = CIRCLE ( 'NONE', #5801, 31.99999999999998934 ) ;
#26898 = VERTEX_POINT ( 'NONE', #40675 ) ;
#26899 = AXIS2_PLACEMENT_3D ( 'NONE', #13237, #28871, #32779 ) ;
#26900 = DIRECTION ( 'NONE',  ( -1.000000000000000000, 0.000000000000000000, -0.000000000000000000 ) ) ;
#26901 = ORIENTED_EDGE ( 'NONE', *, *, #43592, .T. ) ;
#26902 = CIRCLE ( 'NONE', #10476, 31.99999999999999289 ) ;
#26903 = CARTESIAN_POINT ( 'NONE',  ( 0.000000000000000000, 60.67117009219135326, 55.16347631943062169 ) ) ;
#26904 = DIRECTION ( 'NONE',  ( 0.000000000000000000, -0.9876883405951361050, -0.1564344650402419989 ) ) ;
#26905 = CARTESIAN_POINT ( 'NONE',  ( -3.000000000000000000, -22.67460108101783334, 6.353146135317912169 ) ) ;
#26906 = CARTESIAN_POINT ( 'NONE',  ( 0.000000000000000000, -59.75363087400114637, 56.15606465354937171 ) ) ;
#26907 = LINE ( 'NONE', #1445, #37755 ) ;
#26908 = DIRECTION ( 'NONE',  ( 0.000000000000000000, -0.2334453638559126909, 0.9723699203976748917 ) ) ;
#26909 = VECTOR ( 'NONE', #22833, 1000.000000000000000 ) ;
#26910 = DIRECTION ( 'NONE',  ( 0.000000000000000000, 0.000000000000000000, -1.000000000000000000 ) ) ;
#26911 = CARTESIAN_POINT ( 'NONE',  ( 0.000000000000000000, 76.69515212746057387, -29.01471420065479379 ) ) ;
#26912 = LINE ( 'NONE', #4628, #9817 ) ;
#26913 = ADVANCED_FACE ( 'NONE', ( #3218 ), #39970, .T. ) ;
#26914 = CARTESIAN_POINT ( 'NONE',  ( 0.000000000000000000, 21.32104025579114648, 30.84782396557224970 ) ) ;
#26915 = DIRECTION ( 'NONE',  ( -1.000000000000000000, 0.000000000000000000, -0.000000000000000000 ) ) ;
#26916 =( NAMED_UNIT ( * ) PLANE_ANGLE_UNIT ( ) SI_UNIT ( $, .RADIAN. ) );
#26917 = DIRECTION ( 'NONE',  ( 1.000000000000000000, -0.000000000000000000, 0.000000000000000000 ) ) ;
#26918 = EDGE_CURVE ( 'NONE', #30740, #13430, #28110, .T. ) ;
#26919 = VERTEX_POINT ( 'NONE', #22332 ) ;
#26920 = ORIENTED_EDGE ( 'NONE', *, *, #9230, .T. ) ;
#26921 = VECTOR ( 'NONE', #2926, 1000.000000000000000 ) ;
#26922 = ADVANCED_FACE ( 'NONE', ( #44112 ), #3473, .T. ) ;
#26923 = CARTESIAN_POINT ( 'NONE',  ( -11.99999999999999645, 0.000000000000000000, 0.000000000000000000 ) ) ;
#26924 = VECTOR ( 'NONE', #698, 1000.000000000000000 ) ;
#26925 = AXIS2_PLACEMENT_3D ( 'NONE', #18942, #4291, #19202 ) ;
#26926 = AXIS2_PLACEMENT_3D ( 'NONE', #7672, #30430, #37293 ) ;
#26927 = DIRECTION ( 'NONE',  ( 0.000000000000000000, 0.3090169943749412340, 0.9510565162951556406 ) ) ;
#26928 = DIRECTION ( 'NONE',  ( -1.000000000000000000, 0.000000000000000000, 0.000000000000000000 ) ) ;
#26929 = ORIENTED_EDGE ( 'NONE', *, *, #3310, .T. ) ;
#26930 = EDGE_CURVE ( 'NONE', #4565, #42647, #14801, .T. ) ;
#26931 = ORIENTED_EDGE ( 'NONE', *, *, #6268, .F. ) ;
#26932 = AXIS2_PLACEMENT_3D ( 'NONE', #33658, #40309, #26333 ) ;
#26933 = AXIS2_PLACEMENT_3D ( 'NONE', #6384, #6861, #32787 ) ;
#26934 = EDGE_CURVE ( 'NONE', #36269, #40640, #44588, .T. ) ;
#26935 = CIRCLE ( 'NONE', #41021, 31.99999999999999289 ) ;
#26936 = CARTESIAN_POINT ( 'NONE',  ( 15.00000000000000000, 22.07842321921480888, -8.187992925817425771 ) ) ;
#26937 = CIRCLE ( 'NONE', #33181, 82.00000000000000000 ) ;
#26938 = ORIENTED_EDGE ( 'NONE', *, *, #19909, .F. ) ;
#26939 = VERTEX_POINT ( 'NONE', #18642 ) ;
#26940 = ORIENTED_EDGE ( 'NONE', *, *, #23995, .T. ) ;
#26941 = ORIENTED_EDGE ( 'NONE', *, *, #23488, .T. ) ;
#26942 = VECTOR ( 'NONE', #46654, 1000.000000000000000 ) ;
#26943 = EDGE_CURVE ( 'NONE', #5822, #30085, #33340, .T. ) ;
#26944 = CARTESIAN_POINT ( 'NONE',  ( 12.50000000000000000, -107.5000000000000000, 2.500000000000000000 ) ) ;
#26945 = VERTEX_POINT ( 'NONE', #11320 ) ;
#26946 = ORIENTED_EDGE ( 'NONE', *, *, #35523, .T. ) ;
#26947 = LINE ( 'NONE', #42346, #18431 ) ;
#26948 = ORIENTED_EDGE ( 'NONE', *, *, #18333, .T. ) ;
#26949 = CARTESIAN_POINT ( 'NONE',  ( 0.000000000000000000, -120.0000000000000000, -125.0000000000000000 ) ) ;
#26950 = EDGE_LOOP ( 'NONE', ( #11690, #13286, #40649, #3840 ) ) ;
#26951 = DIRECTION ( 'NONE',  ( -0.9038112904824853189, 0.4279312458752976833, 0.000000000000000000 ) ) ;
#26952 = CARTESIAN_POINT ( 'NONE',  ( 0.000000000000000000, 0.000000000000000000, -54.99999999999998579 ) ) ;
#26953 = VERTEX_POINT ( 'NONE', #22066 ) ;
#26954 = DIRECTION ( 'NONE',  ( 0.000000000000000000, 0.000000000000000000, 1.000000000000000000 ) ) ;
#26955 = ORIENTED_EDGE ( 'NONE', *, *, #25801, .F. ) ;
#26956 = DIRECTION ( 'NONE',  ( 0.000000000000000000, 0.000000000000000000, -1.000000000000000000 ) ) ;
#26957 = AXIS2_PLACEMENT_3D ( 'NONE', #44765, #45487, #41588 ) ;
#26958 = CARTESIAN_POINT ( 'NONE',  ( 11.99999999999999822, 62.20884554314020676, 46.21855187248652896 ) ) ;
#26959 = EDGE_LOOP ( 'NONE', ( #23853, #32374, #18528, #22383 ) ) ;
#26960 = DIRECTION ( 'NONE',  ( -1.000000000000000000, 0.000000000000000000, -0.000000000000000000 ) ) ;
#26961 = ORIENTED_EDGE ( 'NONE', *, *, #33269, .T. ) ;
#26962 = CARTESIAN_POINT ( 'NONE',  ( 0.000000000000000000, -73.73191006444582740, 14.66109333815435889 ) ) ;
#26963 = CIRCLE ( 'NONE', #12125, 82.00000000000000000 ) ;
#26964 = LINE ( 'NONE', #19578, #42593 ) ;
#26965 = EDGE_LOOP ( 'NONE', ( #30484, #4125, #27677, #37928 ) ) ;
#26966 = AXIS2_PLACEMENT_3D ( 'NONE', #11338, #45833, #34303 ) ;
#26967 = DIRECTION ( 'NONE',  ( -0.000000000000000000, -0.000000000000000000, -1.000000000000000000 ) ) ;
#26968 = DIRECTION ( 'NONE',  ( -0.000000000000000000, -0.000000000000000000, -1.000000000000000000 ) ) ;
#26969 = CARTESIAN_POINT ( 'NONE',  ( 12.69589495141918611, -96.69089767102708777, 5.500000000000000000 ) ) ;
#26970 = CARTESIAN_POINT ( 'NONE',  ( 0.000000000000000000, -73.73191006444561424, -14.66109333815538918 ) ) ;
#26971 = DIRECTION ( 'NONE',  ( 0.000000000000000000, 0.000000000000000000, 1.000000000000000000 ) ) ;
#26972 = FACE_OUTER_BOUND ( 'NONE', #10633, .T. ) ;
#26973 = ORIENTED_EDGE ( 'NONE', *, *, #34688, .T. ) ;
#26974 = VECTOR ( 'NONE', #29692, 1000.000000000000000 ) ;
#26975 = AXIS2_PLACEMENT_3D ( 'NONE', #21778, #36703, #4411 ) ;
#26976 = DIRECTION ( 'NONE',  ( 0.000000000000000000, 0.000000000000000000, 1.000000000000000000 ) ) ;
#26977 = CARTESIAN_POINT ( 'NONE',  ( 0.000000000000000000, 0.000000000000000000, 0.000000000000000000 ) ) ;
#26978 = PLANE ( 'NONE',  #7524 ) ;
#26979 = EDGE_CURVE ( 'NONE', #22916, #1311, #32766, .T. ) ;
#26980 = ORIENTED_EDGE ( 'NONE', *, *, #46708, .F. ) ;
#26981 = EDGE_CURVE ( 'NONE', #1470, #24537, #17926, .T. ) ;
#26982 = CIRCLE ( 'NONE', #1963, 42.00000000000000000 ) ;
#26983 = CARTESIAN_POINT ( 'NONE',  ( -3.000000000000000000, -18.13022148937243472, -15.02647892043568767 ) ) ;
#26984 = LINE ( 'NONE', #1272, #28500 ) ;
#26985 = DIRECTION ( 'NONE',  ( -1.000000000000000000, 0.000000000000000000, -0.000000000000000000 ) ) ;
#26986 = DIRECTION ( 'NONE',  ( -0.000000000000000000, -0.000000000000000000, -1.000000000000000000 ) ) ;
#26987 = EDGE_CURVE ( 'NONE', #32749, #16632, #48015, .T. ) ;
#26988 = VERTEX_POINT ( 'NONE', #7392 ) ;
#26989 = VERTEX_POINT ( 'NONE', #21826 ) ;
#26990 = FACE_BOUND ( 'NONE', #48302, .T. ) ;
#26991 = ADVANCED_FACE ( 'NONE', ( #14504 ), #28928, .T. ) ;
#26992 = ORIENTED_EDGE ( 'NONE', *, *, #32506, .F. ) ;
#26993 = EDGE_CURVE ( 'NONE', #5309, #17850, #29431, .T. ) ;
#26994 = CYLINDRICAL_SURFACE ( 'NONE', #34604, 31.99999999999998579 ) ;
#26995 = CIRCLE ( 'NONE', #44977, 31.99999999999998934 ) ;
#26996 = DIRECTION ( 'NONE',  ( -0.2867529058022021404, 0.9580045777625456616, 0.000000000000000000 ) ) ;
#26997 = ORIENTED_EDGE ( 'NONE', *, *, #21744, .T. ) ;
#26998 = CARTESIAN_POINT ( 'NONE',  ( 10.00000000000000000, -33.80338159004273280, -16.23288003029533044 ) ) ;
#26999 = ORIENTED_EDGE ( 'NONE', *, *, #44755, .T. ) ;
#27000 = EDGE_CURVE ( 'NONE', #46255, #1961, #32611, .T. ) ;
#27001 = VECTOR ( 'NONE', #38253, 1000.000000000000114 ) ;
#27002 = AXIS2_PLACEMENT_3D ( 'NONE', #18130, #9588, #20871 ) ;
#27003 = CARTESIAN_POINT ( 'NONE',  ( 0.000000000000000000, 39.04073710021344112, 15.48615015657596672 ) ) ;
#27004 = CARTESIAN_POINT ( 'NONE',  ( 10.00000000000000000, 0.000000000000000000, 0.000000000000000000 ) ) ;
#27005 = DIRECTION ( 'NONE',  ( 0.000000000000000000, 0.000000000000000000, 1.000000000000000000 ) ) ;
#27006 = ORIENTED_EDGE ( 'NONE', *, *, #42432, .T. ) ;
#27007 = CIRCLE ( 'NONE', #34009, 31.99999999999998579 ) ;
#27008 = EDGE_CURVE ( 'NONE', #4028, #20089, #23416, .T. ) ;
#27009 = AXIS2_PLACEMENT_3D ( 'NONE', #8687, #35366, #1851 ) ;
#27010 = AXIS2_PLACEMENT_3D ( 'NONE', #29351, #21523, #22250 ) ;
#27011 = LINE ( 'NONE', #42165, #13647 ) ;
#27012 = CARTESIAN_POINT ( 'NONE',  ( 12.00000000000000000, -20.55727247249725664, 16.78983467731313084 ) ) ;
#27013 = DIRECTION ( 'NONE',  ( 1.000000000000000000, 0.000000000000000000, -0.000000000000000000 ) ) ;
#27014 = EDGE_CURVE ( 'NONE', #31086, #29937, #38276, .T. ) ;
#27016 = EDGE_LOOP ( 'NONE', ( #12063, #18175, #31068, #31706 ) ) ;
#27015 = LINE ( 'NONE', #16241, #29650 ) ;
#27017 = ORIENTED_EDGE ( 'NONE', *, *, #5747, .F. ) ;
#27018 = DIRECTION ( 'NONE',  ( 0.000000000000000000, -0.9510565162951565288, 0.3090169943749382364 ) ) ;
#27019 = ORIENTED_EDGE ( 'NONE', *, *, #35214, .F. ) ;
#27020 = ORIENTED_EDGE ( 'NONE', *, *, #5539, .F. ) ;
#27021 = CARTESIAN_POINT ( 'NONE',  ( 0.000000000000000000, 16.65972982745046238, -80.28980883073738539 ) ) ;
#27022 = ORIENTED_EDGE ( 'NONE', *, *, #36151, .T. ) ;
#27023 = CARTESIAN_POINT ( 'NONE',  ( -7.468086116107294004, -12.33868914344945189, -1.199999999999999956 ) ) ;
#27024 = AXIS2_PLACEMENT_3D ( 'NONE', #38165, #1942, #15892 ) ;
#27025 = DIRECTION ( 'NONE',  ( -1.000000000000000000, -0.000000000000000000, -0.000000000000000000 ) ) ;
#27026 = DIRECTION ( 'NONE',  ( 0.000000000000000000, 0.000000000000000000, 1.000000000000000000 ) ) ;
#27027 = ORIENTED_EDGE ( 'NONE', *, *, #18933, .F. ) ;
#27028 = CARTESIAN_POINT ( 'NONE',  ( 0.000000000000000000, 36.13751322684449008, -21.40280677340332716 ) ) ;
#27029 = CARTESIAN_POINT ( 'NONE',  ( 11.99999999999999822, 51.03279382321088065, 55.19960302592086521 ) ) ;
#27030 = DIRECTION ( 'NONE',  ( 0.000000000000000000, 0.000000000000000000, 1.000000000000000000 ) ) ;
#27031 = CARTESIAN_POINT ( 'NONE',  ( -18.12185313557660038, -104.9634299478706794, 2.500000000000000000 ) ) ;
#27032 = CARTESIAN_POINT ( 'NONE',  ( 10.00000000000000000, 68.67312586194995561, 35.91791733033500122 ) ) ;
#27033 = CARTESIAN_POINT ( 'NONE',  ( 11.99999999999999822, -73.44644590900043113, -24.73286445877782924 ) ) ;
#27034 = DIRECTION ( 'NONE',  ( -0.000000000000000000, -0.000000000000000000, -1.000000000000000000 ) ) ;
#27035 = CARTESIAN_POINT ( 'NONE',  ( 10.00000000000000000, 0.000000000000000000, 0.000000000000000000 ) ) ;
#27036 = EDGE_CURVE ( 'NONE', #44505, #44810, #33542, .T. ) ;
#27037 = DIRECTION ( 'NONE',  ( -1.000000000000000000, -0.000000000000000000, 0.000000000000000000 ) ) ;
#27038 = DIRECTION ( 'NONE',  ( -1.000000000000000000, -0.000000000000000000, -0.000000000000000000 ) ) ;
#27039 = EDGE_CURVE ( 'NONE', #21719, #22698, #47762, .T. ) ;
#27040 = VERTEX_POINT ( 'NONE', #40451 ) ;
#27041 = CARTESIAN_POINT ( 'NONE',  ( 11.99999999999999822, -73.95703589263990807, 23.16143007188399139 ) ) ;
#27042 = ORIENTED_EDGE ( 'NONE', *, *, #12447, .T. ) ;
#27043 = VECTOR ( 'NONE', #26156, 1000.000000000000000 ) ;
#27044 = CARTESIAN_POINT ( 'NONE',  ( 10.00000000000000000, -76.41127070299280888, 12.93880638057289012 ) ) ;
#27045 = CARTESIAN_POINT ( 'NONE',  ( 0.000000000000000000, 35.53030884539084866, 12.26510123303271982 ) ) ;
#27046 = ORIENTED_EDGE ( 'NONE', *, *, #24883, .T. ) ;
#27047 = VERTEX_POINT ( 'NONE', #4209 ) ;
#27048 = ADVANCED_FACE ( 'NONE', ( #4920 ), #27207, .T. ) ;
#27049 = AXIS2_PLACEMENT_3D ( 'NONE', #39559, #21167, #17743 ) ;
#27050 = DIRECTION ( 'NONE',  ( 1.000000000000000000, -0.000000000000000000, -0.000000000000000000 ) ) ;
#27051 = AXIS2_PLACEMENT_3D ( 'NONE', #805, #42673, #45599 ) ;
#27052 = ORIENTED_EDGE ( 'NONE', *, *, #2055, .F. ) ;
#27053 = ORIENTED_EDGE ( 'NONE', *, *, #27901, .F. ) ;
#27054 = AXIS2_PLACEMENT_3D ( 'NONE', #9090, #20326, #27951 ) ;
#27055 = ORIENTED_EDGE ( 'NONE', *, *, #46135, .F. ) ;
#27056 = CYLINDRICAL_SURFACE ( 'NONE', #16402, 42.00000000000000000 ) ;
#27057 = CIRCLE ( 'NONE', #27876, 82.00000000000000000 ) ;
#27058 = EDGE_LOOP ( 'NONE', ( #990, #511, #10077, #17263 ) ) ;
#27059 = AXIS2_PLACEMENT_3D ( 'NONE', #41595, #33998, #34234 ) ;
#27060 = CARTESIAN_POINT ( 'NONE',  ( 0.000000000000000000, 38.55633173627010279, 16.65560815589424593 ) ) ;
#27061 = CARTESIAN_POINT ( 'NONE',  ( 0.000000000000000000, 40.98264845739749518, 9.188173127307448951 ) ) ;
#27062 = LINE ( 'NONE', #19219, #25377 ) ;
#27063 = ORIENTED_EDGE ( 'NONE', *, *, #10899, .T. ) ;
#27064 = CARTESIAN_POINT ( 'NONE',  ( 0.000000000000000000, 0.6853352020795618893, -37.58145647212453611 ) ) ;
#27065 = ORIENTED_EDGE ( 'NONE', *, *, #14044, .T. ) ;
#27066 = AXIS2_PLACEMENT_3D ( 'NONE', #47379, #6493, #18215 ) ;
#27067 = ORIENTED_EDGE ( 'NONE', *, *, #25125, .F. ) ;
#27068 = ORIENTED_EDGE ( 'NONE', *, *, #2215, .F. ) ;
#27069 = DIRECTION ( 'NONE',  ( 0.000000000000000000, 0.4539904997395413089, 0.8910065241883705633 ) ) ;
#27070 = CARTESIAN_POINT ( 'NONE',  ( 10.00000000000000000, 73.95703589264006439, -23.16143007188350822 ) ) ;
#27071 = AXIS2_PLACEMENT_3D ( 'NONE', #22957, #38876, #23436 ) ;
#27072 = ORIENTED_EDGE ( 'NONE', *, *, #6802, .T. ) ;
#27073 = VERTEX_POINT ( 'NONE', #33802 ) ;
#27074 = DIRECTION ( 'NONE',  ( -1.000000000000000000, 0.000000000000000000, -0.000000000000000000 ) ) ;
#27075 = VERTEX_POINT ( 'NONE', #15465 ) ;
#27076 = CARTESIAN_POINT ( 'NONE',  ( 10.00000000000000000, 0.000000000000000000, 0.000000000000000000 ) ) ;
#27077 = EDGE_CURVE ( 'NONE', #1459, #29919, #757, .T. ) ;
#27078 = VECTOR ( 'NONE', #28467, 1000.000000000000000 ) ;
#27079 = CARTESIAN_POINT ( 'NONE',  ( 0.000000000000000000, 20.85821328998741109, 10.92862929874522315 ) ) ;
#27080 = CARTESIAN_POINT ( 'NONE',  ( 10.00000000000000000, 35.38097989696528600, -12.42422080174602605 ) ) ;
#27081 = DIRECTION ( 'NONE',  ( 0.000000000000000000, -0.8090169943749532244, 0.5877852522924652545 ) ) ;
#27082 = CARTESIAN_POINT ( 'NONE',  ( 10.00000000000000178, 0.000000000000000000, 0.000000000000000000 ) ) ;
#27083 = DIRECTION ( 'NONE',  ( 0.000000000000000000, 0.000000000000000000, 1.000000000000000000 ) ) ;
#27084 = CARTESIAN_POINT ( 'NONE',  ( -10.00000000000000000, 0.000000000000000000, 0.000000000000000000 ) ) ;
#27085 = DIRECTION ( 'NONE',  ( 0.08130631524010117905, -0.9966891607226784355, 0.000000000000000000 ) ) ;
#27086 = DIRECTION ( 'NONE',  ( 0.5200609990132993854, 0.8541291221503275466, 0.000000000000000000 ) ) ;
#27087 = CARTESIAN_POINT ( 'NONE',  ( 10.00000000000000000, 0.000000000000000000, 0.000000000000000000 ) ) ;
#27088 = CARTESIAN_POINT ( 'NONE',  ( 6.000000000000000000, 80.55351364060611274, -15.33399622253396899 ) ) ;
#27089 = VERTEX_POINT ( 'NONE', #42132 ) ;
#27090 = VERTEX_POINT ( 'NONE', #34286 ) ;
#27091 = AXIS2_PLACEMENT_3D ( 'NONE', #29490, #33405, #35443 ) ;
#27092 = DIRECTION ( 'NONE',  ( 0.000000000000000000, 0.000000000000000000, 1.000000000000000000 ) ) ;
#27093 = CARTESIAN_POINT ( 'NONE',  ( 11.99999999999999822, -41.76937507738831812, 62.50329211542423025 ) ) ;
#27094 = LINE ( 'NONE', #7265, #21240 ) ;
#27095 = DIRECTION ( 'NONE',  ( 0.000000000000000000, 0.2334453638558989796, 0.9723699203976782224 ) ) ;
#27096 = EDGE_CURVE ( 'NONE', #48217, #18490, #37979, .T. ) ;
#27097 = VECTOR ( 'NONE', #37962, 1000.000000000000000 ) ;
#27098 = EDGE_CURVE ( 'NONE', #46297, #25935, #42960, .T. ) ;
#27099 = EDGE_CURVE ( 'NONE', #23605, #19451, #21036, .T. ) ;
#27100 = PRESENTATION_STYLE_ASSIGNMENT (( #38109 ) ) ;
#27101 = PLANE ( 'NONE',  #31095 ) ;
#27102 = AXIS2_PLACEMENT_3D ( 'NONE', #421, #33465, #34186 ) ;
#27103 = ORIENTED_EDGE ( 'NONE', *, *, #40898, .F. ) ;
#27104 = CARTESIAN_POINT ( 'NONE',  ( 10.00000000000000000, 40.98264845739749518, 9.188173127307441845 ) ) ;
#27105 = CARTESIAN_POINT ( 'NONE',  ( 10.00000000000000000, -65.58780272294100655, 36.73666225445870737 ) ) ;
#27106 = EDGE_CURVE ( 'NONE', #17899, #6838, #729, .T. ) ;
#27107 = ADVANCED_FACE ( 'NONE', ( #7864 ), #274, .F. ) ;
#27108 = ORIENTED_EDGE ( 'NONE', *, *, #30250, .T. ) ;
#27109 =( NAMED_UNIT ( * ) SI_UNIT ( $, .STERADIAN. ) SOLID_ANGLE_UNIT ( ) );
#27110 = CARTESIAN_POINT ( 'NONE',  ( 5.000000000000002665, -22.90783923731686045, 78.73519480814945837 ) ) ;
#27111 = ORIENTED_EDGE ( 'NONE', *, *, #44436, .F. ) ;
#27112 = ORIENTED_EDGE ( 'NONE', *, *, #23866, .F. ) ;
#27113 = CIRCLE ( 'NONE', #18494, 31.99999999999998579 ) ;
#27114 = ORIENTED_EDGE ( 'NONE', *, *, #6674, .F. ) ;
#27115 = EDGE_CURVE ( 'NONE', #37098, #24652, #16195, .T. ) ;
#27116 = CIRCLE ( 'NONE', #1291, 77.49900000000000944 ) ;
#27117 = LINE ( 'NONE', #35400, #4631 ) ;
#27118 = ORIENTED_EDGE ( 'NONE', *, *, #21286, .T. ) ;
#27119 = EDGE_CURVE ( 'NONE', #47457, #21501, #24949, .T. ) ;
#27120 = ORIENTED_EDGE ( 'NONE', *, *, #9998, .T. ) ;
#27121 = DIRECTION ( 'NONE',  ( 0.000000000000000000, 0.5877852522924797984, -0.8090169943749426773 ) ) ;
#27122 = ORIENTED_EDGE ( 'NONE', *, *, #28471, .T. ) ;
#27123 = VERTEX_POINT ( 'NONE', #31125 ) ;
#27124 = AXIS2_PLACEMENT_3D ( 'NONE', #31983, #5059, #17253 ) ;
#27125 = LINE ( 'NONE', #7780, #46812 ) ;
#27126 = DIRECTION ( 'NONE',  ( 0.000000000000000000, 0.000000000000000000, 1.000000000000000000 ) ) ;
#27127 = CIRCLE ( 'NONE', #9159, 16.00000000000000000 ) ;
#27128 = CARTESIAN_POINT ( 'NONE',  ( 0.000000000000000000, -120.0000000000000000, 2.500000000000000000 ) ) ;
#27129 = EDGE_CURVE ( 'NONE', #13681, #35947, #13259, .T. ) ;
#27130 = ORIENTED_EDGE ( 'NONE', *, *, #37622, .F. ) ;
#27131 = CYLINDRICAL_SURFACE ( 'NONE', #19262, 42.00000000000000000 ) ;
#27132 = ORIENTED_EDGE ( 'NONE', *, *, #2960, .F. ) ;
#27133 = ORIENTED_EDGE ( 'NONE', *, *, #12839, .T. ) ;
#27134 = DIRECTION ( 'NONE',  ( -1.000000000000000000, -0.000000000000000000, 0.000000000000000000 ) ) ;
#27135 = DIRECTION ( 'NONE',  ( -1.000000000000000000, -0.000000000000000000, 0.000000000000000000 ) ) ;
#27136 = ADVANCED_FACE ( 'NONE', ( #12041 ), #22565, .T. ) ;
#27137 = ORIENTED_EDGE ( 'NONE', *, *, #5996, .T. ) ;
#27138 = DIRECTION ( 'NONE',  ( 0.000000000000000000, 0.000000000000000000, 1.000000000000000000 ) ) ;
#27139 = DIRECTION ( 'NONE',  ( 0.000000000000000000, 0.000000000000000000, -1.000000000000000000 ) ) ;
#27140 = EDGE_CURVE ( 'NONE', #22304, #36859, #18870, .T. ) ;
#27141 = ORIENTED_EDGE ( 'NONE', *, *, #31861, .T. ) ;
#27142 = ORIENTED_EDGE ( 'NONE', *, *, #16850, .F. ) ;
#27143 = CIRCLE ( 'NONE', #22415, 12.49999999999999645 ) ;
#27144 =( NAMED_UNIT ( * ) SI_UNIT ( $, .STERADIAN. ) SOLID_ANGLE_UNIT ( ) );
#27145 = CARTESIAN_POINT ( 'NONE',  ( 0.000000000000000000, -66.50666863322028632, 39.78640506895582973 ) ) ;
#27146 = AXIS2_PLACEMENT_3D ( 'NONE', #2314, #23875, #5282 ) ;
#27147 = ORIENTED_EDGE ( 'NONE', *, *, #30966, .T. ) ;
#27148 = CYLINDRICAL_SURFACE ( 'NONE', #30679, 16.00000000000000000 ) ;
#27149 = ORIENTED_EDGE ( 'NONE', *, *, #43713, .F. ) ;
#27150 = CARTESIAN_POINT ( 'NONE',  ( 4.999999999999999112, -41.91543099594819921, 2.663952781846001816 ) ) ;
#27151 = LINE ( 'NONE', #37918, #17707 ) ;
#27152 = CYLINDRICAL_SURFACE ( 'NONE', #30820, 82.00000000000000000 ) ;
#27153 = EDGE_LOOP ( 'NONE', ( #649, #26088, #38864, #19619 ) ) ;
#27154 = DIRECTION ( 'NONE',  ( 0.000000000000000000, 0.000000000000000000, 1.000000000000000000 ) ) ;
#27155 = ADVANCED_FACE ( 'NONE', ( #34054 ), #23515, .T. ) ;
#27156 = EDGE_CURVE ( 'NONE', #39835, #3149, #26720, .T. ) ;
#27157 = DIRECTION ( 'NONE',  ( 1.000000000000000000, -0.000000000000000000, 0.000000000000000000 ) ) ;
#27158 = VECTOR ( 'NONE', #18149, 999.9999999999998863 ) ;
#27159 = CARTESIAN_POINT ( 'NONE',  ( 10.00000000000000000, -74.65491531819111515, 23.16904090965678975 ) ) ;
#27160 = CYLINDRICAL_SURFACE ( 'NONE', #2045, 31.99999999999998579 ) ;
#27161 = CARTESIAN_POINT ( 'NONE',  ( 0.000000000000000000, -19.89357724625003598, 12.59942793731059574 ) ) ;
#27162 = CARTESIAN_POINT ( 'NONE',  ( 10.00000000000000000, 0.000000000000000000, 0.000000000000000000 ) ) ;
#27163 = EDGE_CURVE ( 'NONE', #35465, #34102, #19361, .T. ) ;
#27164 = ORIENTED_EDGE ( 'NONE', *, *, #38351, .T. ) ;
#27165 = CONICAL_SURFACE ( 'NONE', #15424, 20.64000000000000057, 0.7853981633974482790 ) ;
#27166 = DIRECTION ( 'NONE',  ( -1.000000000000000000, -0.000000000000000000, -0.000000000000000000 ) ) ;
#27167 = ORIENTED_EDGE ( 'NONE', *, *, #11828, .F. ) ;
#27168 = CARTESIAN_POINT ( 'NONE',  ( 15.00000000000000000, -11.95096189432312350, 23.69967320028773372 ) ) ;
#27169 = DIRECTION ( 'NONE',  ( -1.000000000000000000, -0.000000000000000000, -0.000000000000000000 ) ) ;
#27170 = ORIENTED_EDGE ( 'NONE', *, *, #32329, .F. ) ;
#27171 = VECTOR ( 'NONE', #11308, 1000.000000000000000 ) ;
#27172 = CARTESIAN_POINT ( 'NONE',  ( 0.000000000000000000, 75.11725578898467859, 2.956366410620910656 ) ) ;
#27173 = ORIENTED_EDGE ( 'NONE', *, *, #30546, .F. ) ;
#27174 = VECTOR ( 'NONE', #3348, 1000.000000000000114 ) ;
#27175 = EDGE_LOOP ( 'NONE', ( #32314, #41754, #26580, #961 ) ) ;
#27176 = ORIENTED_EDGE ( 'NONE', *, *, #27257, .T. ) ;
#27177 = ORIENTED_EDGE ( 'NONE', *, *, #30195, .T. ) ;
#27178 = ORIENTED_EDGE ( 'NONE', *, *, #44319, .T. ) ;
#27179 = DIRECTION ( 'NONE',  ( -1.000000000000000000, 0.000000000000000000, -0.000000000000000000 ) ) ;
#27180 = EDGE_CURVE ( 'NONE', #15804, #390, #30887, .T. ) ;
#27181 = VECTOR ( 'NONE', #30893, 1000.000000000000114 ) ;
#27182 = ORIENTED_EDGE ( 'NONE', *, *, #33692, .T. ) ;
#27183 = LINE ( 'NONE', #46025, #11426 ) ;
#27184 = EDGE_LOOP ( 'NONE', ( #35890, #39445, #20747, #6990 ) ) ;
#27185 = CARTESIAN_POINT ( 'NONE',  ( 10.00000000000000000, -17.67226234102801286, -33.17418723428327354 ) ) ;
#27186 = ORIENTED_EDGE ( 'NONE', *, *, #29689, .T. ) ;
#27187 = EDGE_CURVE ( 'NONE', #17554, #25213, #38457, .T. ) ;
#27188 = DIRECTION ( 'NONE',  ( -1.000000000000000000, -0.000000000000000000, -0.000000000000000000 ) ) ;
#27189 = CARTESIAN_POINT ( 'NONE',  ( 11.99999999999999822, 0.000000000000000000, 0.000000000000000000 ) ) ;
#27190 = EDGE_CURVE ( 'NONE', #31053, #42577, #31226, .T. ) ;
#27191 = VERTEX_POINT ( 'NONE', #23761 ) ;
#27192 = PLANE ( 'NONE',  #3212 ) ;
#27193 = ORIENTED_EDGE ( 'NONE', *, *, #40473, .T. ) ;
#27194 = CIRCLE ( 'NONE', #8424, 82.00000000000000000 ) ;
#27195 = LINE ( 'NONE', #30871, #44611 ) ;
#27196 = CYLINDRICAL_SURFACE ( 'NONE', #45394, 82.00000000000000000 ) ;
#27197 = ORIENTED_EDGE ( 'NONE', *, *, #36362, .T. ) ;
#27198 = CARTESIAN_POINT ( 'NONE',  ( -14.87942725330654348, -141.9795960975983178, -2.500000000000000000 ) ) ;
#27199 = VERTEX_POINT ( 'NONE', #35981 ) ;
#27200 = ORIENTED_EDGE ( 'NONE', *, *, #16790, .T. ) ;
#27201 = CARTESIAN_POINT ( 'NONE',  ( 0.000000000000000000, 0.000000000000000000, 0.000000000000000000 ) ) ;
#27202 = DIRECTION ( 'NONE',  ( 1.000000000000000000, 0.000000000000000000, 0.000000000000000000 ) ) ;
#27203 = EDGE_LOOP ( 'NONE', ( #31989, #14277, #33908, #5684 ) ) ;
#27204 = LINE ( 'NONE', #45809, #15950 ) ;
#27205 = DIRECTION ( 'NONE',  ( 0.000000000000000000, 0.6494480483301793283, 0.7604059656000345946 ) ) ;
#27206 = DIRECTION ( 'NONE',  ( 0.000000000000000000, 0.000000000000000000, -1.000000000000000000 ) ) ;
#27207 = CYLINDRICAL_SURFACE ( 'NONE', #12464, 37.49900000000000233 ) ;
#27208 = EDGE_CURVE ( 'NONE', #46458, #19020, #31370, .T. ) ;
#27209 = FACE_OUTER_BOUND ( 'NONE', #39595, .T. ) ;
#27210 = ADVANCED_FACE ( 'NONE', ( #16664 ), #32087, .F. ) ;
#27211 = DIRECTION ( 'NONE',  ( 0.000000000000000000, 0.000000000000000000, -1.000000000000000000 ) ) ;
#27212 = VECTOR ( 'NONE', #5641, 1000.000000000000000 ) ;
#27213 = FACE_OUTER_BOUND ( 'NONE', #365, .T. ) ;
#27214 = EDGE_CURVE ( 'NONE', #30440, #48354, #47618, .T. ) ;
#27215 = DIRECTION ( 'NONE',  ( -0.000000000000000000, -0.000000000000000000, -1.000000000000000000 ) ) ;
#27216 = DIRECTION ( 'NONE',  ( 0.000000000000000000, 0.000000000000000000, 1.000000000000000000 ) ) ;
#27217 = ORIENTED_EDGE ( 'NONE', *, *, #15315, .T. ) ;
#27218 = MECHANICAL_DESIGN_GEOMETRIC_PRESENTATION_REPRESENTATION (  '', ( #34989 ), #20145 ) ;
#27219 = CARTESIAN_POINT ( 'NONE',  ( 10.00000000000000000, -81.96053171279899630, -2.543863470249235981 ) ) ;
#27220 = FACE_OUTER_BOUND ( 'NONE', #45742, .T. ) ;
#27222 = VECTOR ( 'NONE', #44217, 1000.000000000000114 ) ;
#27221 = CARTESIAN_POINT ( 'NONE',  ( 0.000000000000000000, 37.22597642581158084, 10.79786254984347593 ) ) ;
#27223 = EDGE_CURVE ( 'NONE', #24537, #23027, #11688, .T. ) ;
#27224 = ORIENTED_EDGE ( 'NONE', *, *, #7584, .F. ) ;
#27225 = DIRECTION ( 'NONE',  ( 0.000000000000000000, 0.000000000000000000, 1.000000000000000000 ) ) ;
#27226 = ORIENTED_EDGE ( 'NONE', *, *, #12601, .F. ) ;
#27227 = DIRECTION ( 'NONE',  ( 1.000000000000000000, -0.000000000000000000, -0.000000000000000000 ) ) ;
#27228 = SHAPE_DEFINITION_REPRESENTATION ( #43706, #40966 ) ;
#27229 = DIRECTION ( 'NONE',  ( -0.9580045777625456616, -0.2867529058022021404, 0.000000000000000000 ) ) ;
#27230 = ORIENTED_EDGE ( 'NONE', *, *, #26918, .T. ) ;
#27231 = AXIS2_PLACEMENT_3D ( 'NONE', #7253, #25843, #43977 ) ;
#27232 = VERTEX_POINT ( 'NONE', #35018 ) ;
#27233 = CARTESIAN_POINT ( 'NONE',  ( 11.99999999999999822, -20.41045688087772092, -72.35160999960838524 ) ) ;
#27234 = ORIENTED_EDGE ( 'NONE', *, *, #46555, .F. ) ;
#27235 = FACE_OUTER_BOUND ( 'NONE', #18011, .T. ) ;
#27236 = ORIENTED_EDGE ( 'NONE', *, *, #23791, .T. ) ;
#27237 = LINE ( 'NONE', #42159, #46177 ) ;
#27238 = ORIENTED_EDGE ( 'NONE', *, *, #36476, .F. ) ;
#27239 = CARTESIAN_POINT ( 'NONE',  ( -23.42219527698293646, -121.9106984081423803, -2.500000000000000000 ) ) ;
#27240 = ORIENTED_EDGE ( 'NONE', *, *, #33329, .F. ) ;
#27242 = EDGE_CURVE ( 'NONE', #1046, #39954, #14025, .T. ) ;
#27241 = AXIS2_PLACEMENT_3D ( 'NONE', #10046, #28881, #43814 ) ;
#27243 = CIRCLE ( 'NONE', #677, 31.99999999999999289 ) ;
#27244 = ADVANCED_FACE ( 'NONE', ( #38717 ), #1992, .F. ) ;
#27245 = CIRCLE ( 'NONE', #28057, 31.99999999999998934 ) ;
#27246 = ADVANCED_FACE ( 'NONE', ( #28161 ), #46285, .T. ) ;
#27247 = CARTESIAN_POINT ( 'NONE',  ( 11.59999999999999787, 1.420590287010929336E-15, -54.99999999999998579 ) ) ;
#27248 = DIRECTION ( 'NONE',  ( -1.000000000000000000, 0.000000000000000000, 0.000000000000000000 ) ) ;
#27249 = DIRECTION ( 'NONE',  ( 1.000000000000000000, 0.000000000000000000, -0.000000000000000000 ) ) ;
#27250 = EDGE_CURVE ( 'NONE', #23892, #24690, #24488, .T. ) ;
#27252 = EDGE_LOOP ( 'NONE', ( #29826, #10267, #30092, #25107 ) ) ;
#27251 = CARTESIAN_POINT ( 'NONE',  ( -6.880223345695647197, -142.5202692415819854, 2.500000000000000000 ) ) ;
#27253 = EDGE_LOOP ( 'NONE', ( #41208, #27613, #13610, #10006 ) ) ;
#27254 = CARTESIAN_POINT ( 'NONE',  ( 0.000000000000000000, 0.000000000000000000, -1.199999999999999956 ) ) ;
#27255 = ORIENTED_EDGE ( 'NONE', *, *, #14053, .T. ) ;
#27256 = VERTEX_POINT ( 'NONE', #21049 ) ;
#27257 = EDGE_CURVE ( 'NONE', #5571, #47807, #9314, .T. ) ;
#27258 = CARTESIAN_POINT ( 'NONE',  ( 10.00000000000000000, 55.38113227695858143, -54.21277698773617715 ) ) ;
#27259 = ORIENTED_EDGE ( 'NONE', *, *, #19332, .F. ) ;
#27260 = CARTESIAN_POINT ( 'NONE',  ( 15.00000000000000000, 5.835314593368470248, -22.81335362449854642 ) ) ;
#27261 = DIRECTION ( 'NONE',  ( 0.2867529058022035837, -0.9580045777625452175, 0.000000000000000000 ) ) ;
#27262 = FACE_OUTER_BOUND ( 'NONE', #45951, .T. ) ;
#27263 = ORIENTED_EDGE ( 'NONE', *, *, #16027, .T. ) ;
#27264 = LINE ( 'NONE', #16482, #46419 ) ;
#27265 = FACE_OUTER_BOUND ( 'NONE', #2947, .T. ) ;
#27266 = CYLINDRICAL_SURFACE ( 'NONE', #14932, 82.00000000000000000 ) ;
#27267 = EDGE_CURVE ( 'NONE', #26813, #34977, #774, .T. ) ;
#27268 = VECTOR ( 'NONE', #33818, 1000.000000000000000 ) ;
#27269 = DIRECTION ( 'NONE',  ( 0.000000000000000000, 0.000000000000000000, 1.000000000000000000 ) ) ;
#27270 = DIRECTION ( 'NONE',  ( 0.000000000000000000, 0.8090169943749445647, 0.5877852522924771339 ) ) ;
#27271 = CYLINDRICAL_SURFACE ( 'NONE', #428, 16.00000000000000000 ) ;
#27272 = EDGE_CURVE ( 'NONE', #47811, #31605, #17139, .T. ) ;
#27273 = LINE ( 'NONE', #31685, #904 ) ;
#27274 = DIRECTION ( 'NONE',  ( -1.000000000000000000, -0.000000000000000000, -0.000000000000000000 ) ) ;
#27275 = DIRECTION ( 'NONE',  ( -1.000000000000000000, -0.000000000000000000, 0.000000000000000000 ) ) ;
#27276 = DIRECTION ( 'NONE',  ( 0.000000000000000000, 0.000000000000000000, 1.000000000000000000 ) ) ;
#27277 = ORIENTED_EDGE ( 'NONE', *, *, #2764, .T. ) ;
#27278 = ADVANCED_FACE ( 'NONE', ( #24738 ), #6135, .T. ) ;
#27279 = ORIENTED_EDGE ( 'NONE', *, *, #15682, .T. ) ;
#27280 = CARTESIAN_POINT ( 'NONE',  ( 0.000000000000000000, 0.000000000000000000, 125.0000000000000000 ) ) ;
#27281 = DIRECTION ( 'NONE',  ( -1.000000000000000000, -0.000000000000000000, 0.000000000000000000 ) ) ;
#27282 = CIRCLE ( 'NONE', #23453, 82.00000000000000000 ) ;
#27283 = ORIENTED_EDGE ( 'NONE', *, *, #25945, .F. ) ;
#27284 = VERTEX_POINT ( 'NONE', #9085 ) ;
#27285 = DIRECTION ( 'NONE',  ( -1.000000000000000000, 0.000000000000000000, 0.000000000000000000 ) ) ;
#27286 = CIRCLE ( 'NONE', #7737, 42.00000000000000000 ) ;
#27287 = VECTOR ( 'NONE', #41096, 1000.000000000000000 ) ;
#27288 = DIRECTION ( 'NONE',  ( -1.000000000000000000, -0.000000000000000000, 0.000000000000000000 ) ) ;
#27289 = ORIENTED_EDGE ( 'NONE', *, *, #47611, .T. ) ;
#27290 = EDGE_CURVE ( 'NONE', #41381, #410, #20094, .T. ) ;
#27291 = VERTEX_POINT ( 'NONE', #27447 ) ;
#27292 = ORIENTED_EDGE ( 'NONE', *, *, #2118, .T. ) ;
#27293 = ORIENTED_EDGE ( 'NONE', *, *, #6854, .F. ) ;
#27294 = ORIENTED_EDGE ( 'NONE', *, *, #10211, .T. ) ;
#27295 = MECHANICAL_DESIGN_GEOMETRIC_PRESENTATION_REPRESENTATION (  '', ( #17872 ), #23366 ) ;
#27296 = DIRECTION ( 'NONE',  ( -1.000000000000000000, 0.000000000000000000, 0.000000000000000000 ) ) ;
#27297 = ADVANCED_FACE ( 'NONE', ( #5179 ), #1500, .T. ) ;
#27298 = CARTESIAN_POINT ( 'NONE',  ( 10.00000000000000000, -73.44644590900043113, -24.73286445877782924 ) ) ;
#27299 = CARTESIAN_POINT ( 'NONE',  ( 10.00000000000000000, 25.88420570971400991, 27.13269053701105449 ) ) ;
#27300 = ORIENTED_EDGE ( 'NONE', *, *, #46637, .T. ) ;
#27301 = DIRECTION ( 'NONE',  ( 0.000000000000000000, 0.000000000000000000, 1.000000000000000000 ) ) ;
#27302 = ORIENTED_EDGE ( 'NONE', *, *, #45644, .T. ) ;
#27303 = ORIENTED_EDGE ( 'NONE', *, *, #47834, .F. ) ;
#27304 = EDGE_CURVE ( 'NONE', #16330, #32691, #15626, .T. ) ;
#27305 = CARTESIAN_POINT ( 'NONE',  ( 0.000000000000000000, -70.53064760720336324, 26.01480285779810231 ) ) ;
#27306 = DIRECTION ( 'NONE',  ( -1.000000000000000000, -0.000000000000000000, -0.000000000000000000 ) ) ;
#27307 = CARTESIAN_POINT ( 'NONE',  ( 5.000000000000000000, -60.67117009219176538, 55.16347631943019536 ) ) ;
#27308 = VECTOR ( 'NONE', #8108, 1000.000000000000000 ) ;
#27309 = VERTEX_POINT ( 'NONE', #36929 ) ;
#27310 = VERTEX_POINT ( 'NONE', #17617 ) ;
#27311 = AXIS2_PLACEMENT_3D ( 'NONE', #13145, #35662, #16568 ) ;
#27312 = CARTESIAN_POINT ( 'NONE',  ( 0.000000000000000000, 0.000000000000000000, 0.000000000000000000 ) ) ;
#27313 = ORIENTED_EDGE ( 'NONE', *, *, #9650, .T. ) ;
#27314 = ADVANCED_FACE ( 'NONE', ( #18343 ), #37191, .T. ) ;
#27315 = FACE_OUTER_BOUND ( 'NONE', #34020, .T. ) ;
#27316 = AXIS2_PLACEMENT_3D ( 'NONE', #33474, #40823, #18550 ) ;
#27317 = CYLINDRICAL_SURFACE ( 'NONE', #32692, 31.99999999999998579 ) ;
#27318 = DIRECTION ( 'NONE',  ( 0.000000000000000000, 0.000000000000000000, -1.000000000000000000 ) ) ;
#27319 = DIRECTION ( 'NONE',  ( 0.000000000000000000, 0.000000000000000000, -1.000000000000000000 ) ) ;
#27320 = DIRECTION ( 'NONE',  ( 0.000000000000000000, 0.9510565162951536422, 0.3090169943749471182 ) ) ;
#27321 = DIRECTION ( 'NONE',  ( -1.000000000000000000, 0.000000000000000000, 0.000000000000000000 ) ) ;
#27322 = CYLINDRICAL_SURFACE ( 'NONE', #18293, 16.00000000000000000 ) ;
#27323 = ORIENTED_EDGE ( 'NONE', *, *, #31152, .F. ) ;
#27324 = FACE_OUTER_BOUND ( 'NONE', #3750, .T. ) ;
#27325 = CARTESIAN_POINT ( 'NONE',  ( 0.000000000000000000, -76.66974797899844418, 11.30684508768314522 ) ) ;
#27326 = CARTESIAN_POINT ( 'NONE',  ( 11.99999999999999822, 8.840884882375075193, 74.65374052328651544 ) ) ;
#27327 = ORIENTED_EDGE ( 'NONE', *, *, #37401, .T. ) ;
#27328 = CIRCLE ( 'NONE', #38251, 77.49900000000000944 ) ;
#27329 = LINE ( 'NONE', #27823, #25472 ) ;
#27330 = CARTESIAN_POINT ( 'NONE',  ( 10.00000000000000000, -0.6853352020787742971, -37.58145647212455032 ) ) ;
#27331 = PLANE ( 'NONE',  #22783 ) ;
#27332 = CARTESIAN_POINT ( 'NONE',  ( 0.000000000000000000, -69.42325613327415113, -34.44570377933671779 ) ) ;
#27333 = DIRECTION ( 'NONE',  ( 0.000000000000000000, 0.5877852522924696954, 0.8090169943749498938 ) ) ;
#27334 = CARTESIAN_POINT ( 'NONE',  ( 10.00000000000000000, 0.000000000000000000, 0.000000000000000000 ) ) ;
#27335 = DIRECTION ( 'NONE',  ( -1.000000000000000000, 0.000000000000000000, 0.000000000000000000 ) ) ;
#27336 = CARTESIAN_POINT ( 'NONE',  ( 10.00000000000000000, -27.74655509720723501, 77.16300072079651784 ) ) ;
#27337 = VERTEX_POINT ( 'NONE', #6375 ) ;
#27338 = ORIENTED_EDGE ( 'NONE', *, *, #36184, .T. ) ;
#27339 = CARTESIAN_POINT ( 'NONE',  ( 6.000000000000000000, 22.90783923731740401, -78.73519480814930205 ) ) ;
#27340 = VERTEX_POINT ( 'NONE', #25673 ) ;
#27341 = ADVANCED_FACE ( 'NONE', ( #47954 ), #33277, .F. ) ;
#27342 = ORIENTED_EDGE ( 'NONE', *, *, #37409, .T. ) ;
#27343 = AXIS2_PLACEMENT_3D ( 'NONE', #9953, #6054, #36845 ) ;
#27344 = ORIENTED_EDGE ( 'NONE', *, *, #36184, .F. ) ;
#27345 = AXIS2_PLACEMENT_3D ( 'NONE', #46799, #32350, #47031 ) ;
#27346 = DIRECTION ( 'NONE',  ( -1.000000000000000000, -0.000000000000000000, -0.000000000000000000 ) ) ;
#27347 = ORIENTED_EDGE ( 'NONE', *, *, #1670, .F. ) ;
#27348 = AXIS2_PLACEMENT_3D ( 'NONE', #19961, #23391, #31738 ) ;
#27349 = ORIENTED_EDGE ( 'NONE', *, *, #37164, .F. ) ;
#27350 = VECTOR ( 'NONE', #43143, 1000.000000000000000 ) ;
#27351 = ADVANCED_FACE ( 'NONE', ( #2680 ), #44051, .T. ) ;
#27352 = DIRECTION ( 'NONE',  ( -0.9918136447140100120, 0.1276937514489704939, 0.000000000000000000 ) ) ;
#27353 = DIRECTION ( 'NONE',  ( -1.000000000000000000, -0.000000000000000000, -0.000000000000000000 ) ) ;
#27354 = VERTEX_POINT ( 'NONE', #40617 ) ;
#27355 = ORIENTED_EDGE ( 'NONE', *, *, #12073, .T. ) ;
#27356 = EDGE_CURVE ( 'NONE', #38735, #46006, #22005, .T. ) ;
#27357 = CARTESIAN_POINT ( 'NONE',  ( -3.000000000000000000, 14.60985201121729737, -18.46759930825687945 ) ) ;
#27359 = ORIENTED_EDGE ( 'NONE', *, *, #45225, .T. ) ;
#27358 = CARTESIAN_POINT ( 'NONE',  ( 10.00000000000000000, 0.000000000000000000, 0.000000000000000000 ) ) ;
#27360 = DIRECTION ( 'NONE',  ( 0.8774505977381978905, 0.4796670183876304283, 0.000000000000000000 ) ) ;
#27361 = ORIENTED_EDGE ( 'NONE', *, *, #20055, .F. ) ;
#27362 = EDGE_LOOP ( 'NONE', ( #14571, #10067, #7056, #15438 ) ) ;
#27363 = PLANE ( 'NONE',  #20037 ) ;
#27364 = ORIENTED_EDGE ( 'NONE', *, *, #25062, .F. ) ;
#27365 = ORIENTED_EDGE ( 'NONE', *, *, #32701, .F. ) ;
#27366 = EDGE_CURVE ( 'NONE', #5777, #39278, #32061, .T. ) ;
#27367 = LINE ( 'NONE', #8749, #9346 ) ;
#27368 = LINE ( 'NONE', #42544, #42090 ) ;
#27369 = ORIENTED_EDGE ( 'NONE', *, *, #33873, .F. ) ;
#27370 = EDGE_CURVE ( 'NONE', #1330, #45913, #25192, .T. ) ;
#27371 = DIRECTION ( 'NONE',  ( 1.000000000000000000, -0.000000000000000000, 0.000000000000000000 ) ) ;
#27372 = DIRECTION ( 'NONE',  ( -1.000000000000000000, 0.000000000000000000, 0.000000000000000000 ) ) ;
#27373 = LINE ( 'NONE', #24412, #21310 ) ;
#27374 = VERTEX_POINT ( 'NONE', #6853 ) ;
#27375 = ORIENTED_EDGE ( 'NONE', *, *, #7045, .T. ) ;
#27376 = DIRECTION ( 'NONE',  ( -1.000000000000000000, -0.000000000000000000, 0.000000000000000000 ) ) ;
#27377 = CIRCLE ( 'NONE', #17985, 1.000000000000000000 ) ;
#27378 = CARTESIAN_POINT ( 'NONE',  ( 5.000000000000000000, 41.91543099594818500, -2.663952781846291362 ) ) ;
#27379 = ORIENTED_EDGE ( 'NONE', *, *, #39115, .T. ) ;
#27380 = CIRCLE ( 'NONE', #35954, 16.00000000000000000 ) ;
#27381 = CARTESIAN_POINT ( 'NONE',  ( 10.00000000000000000, 0.000000000000000000, 0.000000000000000000 ) ) ;
#27382 = VERTEX_POINT ( 'NONE', #43577 ) ;
#27383 = AXIS2_PLACEMENT_3D ( 'NONE', #23481, #33767, #8070 ) ;
#27385 = EDGE_CURVE ( 'NONE', #19503, #36132, #34368, .T. ) ;
#27384 = DIRECTION ( 'NONE',  ( 1.000000000000000000, 0.000000000000000000, 0.000000000000000000 ) ) ;
#27386 = CARTESIAN_POINT ( 'NONE',  ( 0.000000000000000000, 12.26510123303259725, 35.53030884539089840 ) ) ;
#27387 = DIRECTION ( 'NONE',  ( -1.000000000000000000, -0.000000000000000000, -0.000000000000000000 ) ) ;
#27388 = VERTEX_POINT ( 'NONE', #40864 ) ;
#27389 = CARTESIAN_POINT ( 'NONE',  ( 10.00000000000000000, 0.000000000000000000, 0.000000000000000000 ) ) ;
#27390 = CIRCLE ( 'NONE', #11761, 0.5000000000000004441 ) ;
#27391 = EDGE_LOOP ( 'NONE', ( #21126, #46569, #22318, #36508 ) ) ;
#27392 = DIRECTION ( 'NONE',  ( 1.000000000000000000, 0.000000000000000000, 0.000000000000000000 ) ) ;
#27393 = VECTOR ( 'NONE', #7917, 1000.000000000000000 ) ;
#27394 = DIRECTION ( 'NONE',  ( -1.000000000000000000, 0.000000000000000000, 0.000000000000000000 ) ) ;
#27395 = CARTESIAN_POINT ( 'NONE',  ( 0.000000000000000000, 27.05870788708267582, -26.08949754952995903 ) ) ;
#27396 = VECTOR ( 'NONE', #38205, 1000.000000000000000 ) ;
#27397 = CARTESIAN_POINT ( 'NONE',  ( 0.000000000000000000, 3.925862922256769583, -41.81611651403857621 ) ) ;
#27398 = VERTEX_POINT ( 'NONE', #25922 ) ;
#27399 = LINE ( 'NONE', #8775, #17461 ) ;
#27400 = ORIENTED_EDGE ( 'NONE', *, *, #1759, .T. ) ;
#27401 = ORIENTED_EDGE ( 'NONE', *, *, #6410, .F. ) ;
#27402 = ADVANCED_FACE ( 'NONE', ( #14685 ), #7082, .T. ) ;
#27403 = DIRECTION ( 'NONE',  ( 0.000000000000000000, 0.000000000000000000, -1.000000000000000000 ) ) ;
#27404 = EDGE_LOOP ( 'NONE', ( #11875, #40776, #42324, #45984 ) ) ;
#27405 = ADVANCED_FACE ( 'NONE', ( #40150 ), #10524, .T. ) ;
#27406 = ORIENTED_EDGE ( 'NONE', *, *, #40729, .T. ) ;
#27407 = CARTESIAN_POINT ( 'NONE',  ( 0.000000000000000000, 37.58145647212453611, 0.6853352020791767529 ) ) ;
#27408 = CARTESIAN_POINT ( 'NONE',  ( 32.50000000000000000, -120.0000000000000000, -2.500000000000000000 ) ) ;
#27409 = EDGE_CURVE ( 'NONE', #40538, #16837, #1562, .T. ) ;
#27410 = ORIENTED_EDGE ( 'NONE', *, *, #43763, .T. ) ;
#27411 = ORIENTED_EDGE ( 'NONE', *, *, #41777, .F. ) ;
#27412 = AXIS2_PLACEMENT_3D ( 'NONE', #34317, #16702, #20355 ) ;
#27413 = CARTESIAN_POINT ( 'NONE',  ( 10.00000000000000000, -30.80686688397025108, 21.53537804866070715 ) ) ;
#27414 = AXIS2_PLACEMENT_3D ( 'NONE', #12570, #8887, #5235 ) ;
#27415 = CIRCLE ( 'NONE', #5500, 16.00000000000000000 ) ;
#27416 = ORIENTED_EDGE ( 'NONE', *, *, #44489, .F. ) ;
#27417 = ORIENTED_EDGE ( 'NONE', *, *, #35601, .T. ) ;
#27418 = ORIENTED_EDGE ( 'NONE', *, *, #26399, .F. ) ;
#27419 = ORIENTED_EDGE ( 'NONE', *, *, #4442, .T. ) ;
#27420 = EDGE_CURVE ( 'NONE', #37633, #17307, #29368, .T. ) ;
#27421 = EDGE_CURVE ( 'NONE', #23846, #19505, #25437, .T. ) ;
#27422 = EDGE_CURVE ( 'NONE', #3261, #8389, #40635, .T. ) ;
#27423 = CIRCLE ( 'NONE', #40692, 31.99999999999999289 ) ;
#27424 = DIRECTION ( 'NONE',  ( 0.000000000000000000, -0.5877852522924802425, 0.8090169943749422332 ) ) ;
#27425 = ORIENTED_EDGE ( 'NONE', *, *, #36893, .T. ) ;
#27426 = COLOUR_RGB ( '', 0.72549020, 0.75294118, 0.79215686) ;
#27427 = ORIENTED_EDGE ( 'NONE', *, *, #40179, .F. ) ;
#27428 = DIRECTION ( 'NONE',  ( 0.000000000000000000, -0.5877852522924624790, -0.8090169943749553338 ) ) ;
#27429 = VERTEX_POINT ( 'NONE', #28872 ) ;
#27430 = CARTESIAN_POINT ( 'NONE',  ( 5.000000000000000000, -26.79245525562738095, 32.34446384429961796 ) ) ;
#27431 = CARTESIAN_POINT ( 'NONE',  ( -7.893099573151324044, -11.68370571044642503, -1.199999999999999956 ) ) ;
#27432 = DIRECTION ( 'NONE',  ( -1.000000000000000000, -0.000000000000000000, -0.000000000000000000 ) ) ;
#27433 = ORIENTED_EDGE ( 'NONE', *, *, #20225, .T. ) ;
#27434 = CARTESIAN_POINT ( 'NONE',  ( -7.468086116107294004, -12.33868914344945189, 0.000000000000000000 ) ) ;
#27435 = ORIENTED_EDGE ( 'NONE', *, *, #41782, .F. ) ;
#27436 = CARTESIAN_POINT ( 'NONE',  ( 0.000000000000000000, -33.17418723428294669, -17.67226234102862747 ) ) ;
#27437 = DIRECTION ( 'NONE',  ( -1.000000000000000000, -0.000000000000000000, -0.000000000000000000 ) ) ;
#27438 = VERTEX_POINT ( 'NONE', #43807 ) ;
#27439 = DIRECTION ( 'NONE',  ( 0.000000000000000000, 0.000000000000000000, 1.000000000000000000 ) ) ;
#27440 = ORIENTED_EDGE ( 'NONE', *, *, #3488, .T. ) ;
#27441 = ORIENTED_EDGE ( 'NONE', *, *, #46245, .F. ) ;
#27442 = LINE ( 'NONE', #15940, #36953 ) ;
#27443 = FACE_OUTER_BOUND ( 'NONE', #37511, .T. ) ;
#27444 = DIRECTION ( 'NONE',  ( 0.6064928550163524168, 0.7950889364178788110, 0.000000000000000000 ) ) ;
#27445 = DIRECTION ( 'NONE',  ( 0.000000000000000000, -0.07845909572785224328, 0.9969173337331274087 ) ) ;
#27446 = FACE_OUTER_BOUND ( 'NONE', #16593, .T. ) ;
#27447 = CARTESIAN_POINT ( 'NONE',  ( 10.00000000000000000, -76.66974797899844418, 11.30684508768314522 ) ) ;
#27448 = CYLINDRICAL_SURFACE ( 'NONE', #21970, 31.99999999999998579 ) ;
#27450 = CIRCLE ( 'NONE', #44662, 31.99999999999998579 ) ;
#27449 = DIRECTION ( 'NONE',  ( 0.000000000000000000, -0.5877852522924624790, -0.8090169943749553338 ) ) ;
#27451 = AXIS2_PLACEMENT_3D ( 'NONE', #20481, #1416, #16827 ) ;
#27452 = DIRECTION ( 'NONE',  ( 1.000000000000000000, 0.000000000000000000, 0.000000000000000000 ) ) ;
#27453 = DIRECTION ( 'NONE',  ( 1.000000000000000000, 0.000000000000000000, 0.000000000000000000 ) ) ;
#27454 = DIRECTION ( 'NONE',  ( 1.000000000000000000, 0.000000000000000000, 0.000000000000000000 ) ) ;
#27455 = VECTOR ( 'NONE', #20078, 1000.000000000000114 ) ;
#27456 = AXIS2_PLACEMENT_3D ( 'NONE', #35722, #21257, #24712 ) ;
#27457 = CARTESIAN_POINT ( 'NONE',  ( 10.00000000000000000, 35.53030884539084866, 12.26510123303271982 ) ) ;
#27458 = CARTESIAN_POINT ( 'NONE',  ( 10.00000000000000000, 75.16055320797030959, 18.89407956138283851 ) ) ;
#27459 = DIRECTION ( 'NONE',  ( -1.000000000000000000, 0.000000000000000000, 0.000000000000000000 ) ) ;
#27460 = DIRECTION ( 'NONE',  ( 0.000000000000000000, 0.9510565162951503115, 0.3090169943749573878 ) ) ;
#27461 = AXIS2_PLACEMENT_3D ( 'NONE', #33009, #47937, #40604 ) ;
#27462 = ORIENTED_EDGE ( 'NONE', *, *, #6156, .T. ) ;
#27463 = EDGE_CURVE ( 'NONE', #36004, #32527, #19515, .T. ) ;
#27464 = CIRCLE ( 'NONE', #19606, 77.49899999999999523 ) ;
#27465 = ORIENTED_EDGE ( 'NONE', *, *, #37960, .F. ) ;
#27466 = EDGE_CURVE ( 'NONE', #24420, #14894, #8555, .T. ) ;
#27467 = DIRECTION ( 'NONE',  ( -1.000000000000000000, 0.000000000000000000, 0.000000000000000000 ) ) ;
#27468 = MECHANICAL_DESIGN_GEOMETRIC_PRESENTATION_REPRESENTATION (  '', ( #5479 ), #18731 ) ;
#27469 = EDGE_LOOP ( 'NONE', ( #28299, #15199, #12394, #41907 ) ) ;
#27470 = FACE_OUTER_BOUND ( 'NONE', #10844, .T. ) ;
#27471 = EDGE_CURVE ( 'NONE', #16641, #10301, #4624, .T. ) ;
#27472 = PRODUCT_CONTEXT ( 'NONE', #47580, 'mechanical' ) ;
#27473 = DIRECTION ( 'NONE',  ( 0.000000000000000000, 0.3826834323650904479, -0.9238795325112865164 ) ) ;
#27474 = EDGE_CURVE ( 'NONE', #10349, #26114, #22508, .T. ) ;
#27475 = ORIENTED_EDGE ( 'NONE', *, *, #14819, .T. ) ;
#27476 = CARTESIAN_POINT ( 'NONE',  ( 10.00000000000000000, 0.6853352020790449695, 37.58145647212454321 ) ) ;
#27477 = ORIENTED_EDGE ( 'NONE', *, *, #27928, .F. ) ;
#27478 = EDGE_CURVE ( 'NONE', #30509, #38853, #33745, .T. ) ;
#27479 = EDGE_CURVE ( 'NONE', #25392, #43802, #938, .T. ) ;
#27480 = AXIS2_PLACEMENT_3D ( 'NONE', #26243, #10828, #44832 ) ;
#27481 = DIRECTION ( 'NONE',  ( 1.000000000000000000, -0.000000000000000000, 0.000000000000000000 ) ) ;
#27482 = ORIENTED_EDGE ( 'NONE', *, *, #8126, .T. ) ;
#27483 = AXIS2_PLACEMENT_3D ( 'NONE', #19946, #34880, #46149 ) ;
#27484 = DIRECTION ( 'NONE',  ( -0.000000000000000000, -0.7431448254773870277, -0.6691306063588662312 ) ) ;
#27485 = ORIENTED_EDGE ( 'NONE', *, *, #34467, .T. ) ;
#27486 = DIRECTION ( 'NONE',  ( 0.2867529058022011967, -0.9580045777625459946, 0.000000000000000000 ) ) ;
#27487 = AXIS2_PLACEMENT_3D ( 'NONE', #38327, #26102, #41052 ) ;
#27488 = VECTOR ( 'NONE', #12923, 1000.000000000000000 ) ;
#27489 = ORIENTED_EDGE ( 'NONE', *, *, #15325, .F. ) ;
#27490 = ADVANCED_BREP_SHAPE_REPRESENTATION ( '', ( #19494, #11636 ), #12375 ) ;
#27491 = DIRECTION ( 'NONE',  ( 0.2867529058022011967, -0.9580045777625459946, 0.000000000000000000 ) ) ;
#27492 = AXIS2_PLACEMENT_3D ( 'NONE', #32724, #6544, #43031 ) ;
#27493 = DIRECTION ( 'NONE',  ( -1.000000000000000000, 0.000000000000000000, 0.000000000000000000 ) ) ;
#27494 = CARTESIAN_POINT ( 'NONE',  ( 0.000000000000000000, 0.000000000000000000, 0.000000000000000000 ) ) ;
#27495 = FACE_OUTER_BOUND ( 'NONE', #45553, .T. ) ;
#27496 = EDGE_CURVE ( 'NONE', #26808, #8338, #213, .T. ) ;
#27497 = DIRECTION ( 'NONE',  ( -1.000000000000000000, 0.000000000000000000, -0.000000000000000000 ) ) ;
#27498 = ORIENTED_EDGE ( 'NONE', *, *, #21099, .F. ) ;
#27499 = CARTESIAN_POINT ( 'NONE',  ( 10.00000000000000000, -22.74946021919110706, -29.81001611431033282 ) ) ;
#27500 = ORIENTED_EDGE ( 'NONE', *, *, #32356, .F. ) ;
#27501 = VECTOR ( 'NONE', #26530, 1000.000000000000000 ) ;
#27502 = DIRECTION ( 'NONE',  ( 0.000000000000000000, 0.6691306063588569053, -0.7431448254773954654 ) ) ;
#27503 = DIRECTION ( 'NONE',  ( -1.000000000000000000, -0.000000000000000000, 0.000000000000000000 ) ) ;
#27504 = CARTESIAN_POINT ( 'NONE',  ( 10.00000000000000000, 0.000000000000000000, 0.000000000000000000 ) ) ;
#27505 = CARTESIAN_POINT ( 'NONE',  ( 0.000000000000000000, -30.84782396557233142, 21.32104025579104345 ) ) ;
#27506 = EDGE_LOOP ( 'NONE', ( #39170, #28079, #28850, #8674 ) ) ;
#27507 = DIRECTION ( 'NONE',  ( 0.000000000000000000, -0.7604059656000226042, -0.6494480483301934282 ) ) ;
#27508 = FACE_OUTER_BOUND ( 'NONE', #5538, .T. ) ;
#27509 = DIRECTION ( 'NONE',  ( -1.000000000000000000, 0.000000000000000000, -0.000000000000000000 ) ) ;
#27510 = CARTESIAN_POINT ( 'NONE',  ( -6.782329983125267248, 10.49999999999999645, -104.9999999999999858 ) ) ;
#27511 = DIRECTION ( 'NONE',  ( 0.000000000000000000, 0.000000000000000000, 1.000000000000000000 ) ) ;
#27512 = DIRECTION ( 'NONE',  ( 0.000000000000000000, -0.7071067811865389130, -0.7071067811865561215 ) ) ;
#27513 = CARTESIAN_POINT ( 'NONE',  ( 10.00000000000000000, 72.35432306680485226, -20.40083707022909110 ) ) ;
#27514 = DIRECTION ( 'NONE',  ( -1.000000000000000000, -0.000000000000000000, 0.000000000000000000 ) ) ;
#27515 = CARTESIAN_POINT ( 'NONE',  ( 10.00000000000000000, 67.80270845531889279, 46.11716303203210998 ) ) ;
#27516 = CARTESIAN_POINT ( 'NONE',  ( 0.000000000000000000, 0.000000000000000000, 0.000000000000000000 ) ) ;
#27517 = AXIS2_PLACEMENT_3D ( 'NONE', #5653, #29314, #9315 ) ;
#27518 = LINE ( 'NONE', #43421, #41010 ) ;
#27519 = ORIENTED_EDGE ( 'NONE', *, *, #19317, .F. ) ;
#27520 = CARTESIAN_POINT ( 'NONE',  ( 10.00000000000000000, 17.67226234102874116, -33.17418723428288274 ) ) ;
#27521 = CIRCLE ( 'NONE', #29077, 37.49900000000000944 ) ;
#27522 = EDGE_CURVE ( 'NONE', #45508, #18661, #48437, .T. ) ;
#27523 = CARTESIAN_POINT ( 'NONE',  ( 0.000000000000000000, -11.30684508768395524, 76.66974797899831628 ) ) ;
#27524 = EDGE_CURVE ( 'NONE', #38555, #30674, #12489, .T. ) ;
#27525 = CIRCLE ( 'NONE', #25960, 82.00000000000000000 ) ;
#27526 = VERTEX_POINT ( 'NONE', #703 ) ;
#27527 = EDGE_CURVE ( 'NONE', #17470, #37239, #28894, .T. ) ;
#27528 = CIRCLE ( 'NONE', #19675, 31.99999999999999289 ) ;
#27529 = ORIENTED_EDGE ( 'NONE', *, *, #14762, .F. ) ;
#27530 = VERTEX_POINT ( 'NONE', #19064 ) ;
#27531 = EDGE_CURVE ( 'NONE', #48354, #33766, #42186, .T. ) ;
#27532 = PLANE ( 'NONE',  #44052 ) ;
#27533 = ADVANCED_FACE ( 'NONE', ( #26426 ), #19526, .T. ) ;
#27534 = LINE ( 'NONE', #2080, #46907 ) ;
#27535 = FACE_OUTER_BOUND ( 'NONE', #15562, .T. ) ;
#27536 = AXIS2_PLACEMENT_3D ( 'NONE', #24419, #32029, #31802 ) ;
#27537 = ORIENTED_EDGE ( 'NONE', *, *, #41565, .F. ) ;
#27538 = DIRECTION ( 'NONE',  ( 0.000000000000000000, 0.000000000000000000, 1.000000000000000000 ) ) ;
#27539 = ORIENTED_EDGE ( 'NONE', *, *, #44906, .F. ) ;
#27540 = DIRECTION ( 'NONE',  ( -1.000000000000000000, 0.000000000000000000, -0.000000000000000000 ) ) ;
#27541 = DIRECTION ( 'NONE',  ( -1.000000000000000000, -0.000000000000000000, -0.000000000000000000 ) ) ;
#27542 = CARTESIAN_POINT ( 'NONE',  ( -8.637688417678527131, 13.69818742750669394, 52.00000000000002132 ) ) ;
#27543 = VECTOR ( 'NONE', #16078, 1000.000000000000114 ) ;
#27544 = EDGE_CURVE ( 'NONE', #22817, #46629, #30098, .T. ) ;
#27545 = ORIENTED_EDGE ( 'NONE', *, *, #14822, .T. ) ;
#27546 = ORIENTED_EDGE ( 'NONE', *, *, #8906, .F. ) ;
#27547 = EDGE_LOOP ( 'NONE', ( #30127, #5569, #22541, #32881 ) ) ;
#27548 = CARTESIAN_POINT ( 'NONE',  ( 10.00000000000000000, -0.8261519478436571973, 77.49459641780886443 ) ) ;
#27549 = VERTEX_POINT ( 'NONE', #7809 ) ;
#27550 = AXIS2_PLACEMENT_3D ( 'NONE', #29352, #44277, #25655 ) ;
#27551 = CARTESIAN_POINT ( 'NONE',  ( 0.000000000000000000, -68.26794271651239399, -31.47745569255214093 ) ) ;
#27552 = CARTESIAN_POINT ( 'NONE',  ( 11.99999999999999822, -70.52718814184240159, -26.02418014898383802 ) ) ;
#27553 = LINE ( 'NONE', #42235, #8795 ) ;
#27554 = DIRECTION ( 'NONE',  ( -1.000000000000000000, -0.000000000000000000, -0.000000000000000000 ) ) ;
#27555 = CARTESIAN_POINT ( 'NONE',  ( 11.99999999999999822, 28.89263327155746097, 71.91182617369197771 ) ) ;
#27556 = CARTESIAN_POINT ( 'NONE',  ( 4.999999999999999112, 40.98264845739749518, 9.188173127307448951 ) ) ;
#27557 = FACE_OUTER_BOUND ( 'NONE', #4544, .T. ) ;
#27558 = ORIENTED_EDGE ( 'NONE', *, *, #36246, .T. ) ;
#27559 = CARTESIAN_POINT ( 'NONE',  ( 15.00000000000000000, -13.04903810567675393, -19.60159698893424718 ) ) ;
#27560 = DIRECTION ( 'NONE',  ( -1.000000000000000000, 0.000000000000000000, 0.000000000000000000 ) ) ;
#27561 = EDGE_CURVE ( 'NONE', #21422, #1742, #17951, .T. ) ;
#27562 = DIRECTION ( 'NONE',  ( 1.000000000000000000, 0.000000000000000000, 0.000000000000000000 ) ) ;
#27563 = DIRECTION ( 'NONE',  ( -1.000000000000000000, 0.000000000000000000, -0.000000000000000000 ) ) ;
#27564 = ORIENTED_EDGE ( 'NONE', *, *, #31339, .F. ) ;
#27565 = DIRECTION ( 'NONE',  ( -1.000000000000000000, 0.000000000000000000, 0.000000000000000000 ) ) ;
#27566 = CIRCLE ( 'NONE', #10360, 31.99999999999999289 ) ;
#27567 = DIRECTION ( 'NONE',  ( 0.7950889364178798102, -0.6064928550163511956, 0.000000000000000000 ) ) ;
#27568 = LINE ( 'NONE', #4346, #6515 ) ;
#27569 = DIRECTION ( 'NONE',  ( -1.000000000000000000, -0.000000000000000000, -0.000000000000000000 ) ) ;
#27570 = LINE ( 'NONE', #42500, #40487 ) ;
#27571 = VERTEX_POINT ( 'NONE', #8046 ) ;
#27572 = LINE ( 'NONE', #39071, #38062 ) ;
#27573 = FACE_OUTER_BOUND ( 'NONE', #21632, .T. ) ;
#27574 = ORIENTED_EDGE ( 'NONE', *, *, #25461, .F. ) ;
#27575 = EDGE_CURVE ( 'NONE', #5156, #28753, #37921, .T. ) ;
#27576 = VECTOR ( 'NONE', #14677, 1000.000000000000000 ) ;
#27577 = EDGE_CURVE ( 'NONE', #21411, #5642, #48423, .T. ) ;
#27578 = ORIENTED_EDGE ( 'NONE', *, *, #32920, .T. ) ;
#27579 = AXIS2_PLACEMENT_3D ( 'NONE', #36774, #2286, #17205 ) ;
#27580 = DIRECTION ( 'NONE',  ( -1.000000000000000000, 0.000000000000000000, -0.000000000000000000 ) ) ;
#27581 = EDGE_CURVE ( 'NONE', #15507, #27199, #38162, .T. ) ;
#27582 = ORIENTED_EDGE ( 'NONE', *, *, #21673, .F. ) ;
#27583 = EDGE_CURVE ( 'NONE', #22222, #17705, #40058, .T. ) ;
#27584 =( REPRESENTATION_RELATIONSHIP ('NONE','NONE', #5957, #21223 ) REPRESENTATION_RELATIONSHIP_WITH_TRANSFORMATION ( #35530 )SHAPE_REPRESENTATION_RELATIONSHIP( ) );
#27585 = VERTEX_POINT ( 'NONE', #22173 ) ;
#27586 = CIRCLE ( 'NONE', #22887, 31.99999999999998579 ) ;
#27587 = VECTOR ( 'NONE', #33728, 1000.000000000000114 ) ;
#27588 = CARTESIAN_POINT ( 'NONE',  ( 10.00000000000000000, -10.74501242461258244, -35.92658777277521409 ) ) ;
#27589 = ORIENTED_EDGE ( 'NONE', *, *, #18711, .F. ) ;
#27590 = AXIS2_PLACEMENT_3D ( 'NONE', #29549, #3103, #41069 ) ;
#27591 = VECTOR ( 'NONE', #31432, 1000.000000000000000 ) ;
#27592 = CARTESIAN_POINT ( 'NONE',  ( 15.00000000000000000, -22.32062822937469093, 14.36278369418830181 ) ) ;
#27593 = VECTOR ( 'NONE', #35826, 1000.000000000000000 ) ;
#27594 = FACE_OUTER_BOUND ( 'NONE', #33709, .T. ) ;
#27595 = ORIENTED_EDGE ( 'NONE', *, *, #36962, .T. ) ;
#27596 = ORIENTED_EDGE ( 'NONE', *, *, #39351, .T. ) ;
#27597 = CARTESIAN_POINT ( 'NONE',  ( 11.59999999999999787, 1.420590287010929336E-15, 53.20000000000001705 ) ) ;
#27599 = VERTEX_POINT ( 'NONE', #3073 ) ;
#27598 = CARTESIAN_POINT ( 'NONE',  ( 10.00000000000000000, 16.23288003029543347, -33.80338159004267595 ) ) ;
#27600 = EDGE_CURVE ( 'NONE', #24540, #27912, #20294, .T. ) ;
#27601 = PLANE ( 'NONE',  #24328 ) ;
#27602 = VERTEX_POINT ( 'NONE', #14604 ) ;
#27603 = CARTESIAN_POINT ( 'NONE',  ( 0.000000000000000000, 80.28980883073758434, 16.65972982744962749 ) ) ;
#27604 = ORIENTED_EDGE ( 'NONE', *, *, #45262, .F. ) ;
#27605 = ORIENTED_EDGE ( 'NONE', *, *, #20229, .F. ) ;
#27606 = CARTESIAN_POINT ( 'NONE',  ( 0.000000000000000000, 0.000000000000000000, 0.000000000000000000 ) ) ;
#27607 = FACE_OUTER_BOUND ( 'NONE', #21759, .T. ) ;
#27608 = VERTEX_POINT ( 'NONE', #25829 ) ;
#27609 = DIRECTION ( 'NONE',  ( 0.000000000000000000, -0.4539904997395351471, -0.8910065241883737830 ) ) ;
#27610 = DIRECTION ( 'NONE',  ( 0.000000000000000000, -0.8090169943749531134, 0.5877852522924653655 ) ) ;
#27611 = DIRECTION ( 'NONE',  ( -1.000000000000000000, -0.000000000000000000, 0.000000000000000000 ) ) ;
#27612 = EDGE_CURVE ( 'NONE', #6148, #28620, #44681, .T. ) ;
#27613 = ORIENTED_EDGE ( 'NONE', *, *, #20611, .T. ) ;
#27614 = ORIENTED_EDGE ( 'NONE', *, *, #30133, .T. ) ;
#27615 = AXIS2_PLACEMENT_3D ( 'NONE', #28166, #17375, #13956 ) ;
#27616 = CARTESIAN_POINT ( 'NONE',  ( 10.00000000000000000, 75.11725578898472122, -2.956366410619845730 ) ) ;
#27617 = FACE_OUTER_BOUND ( 'NONE', #46193, .T. ) ;
#27618 = VERTEX_POINT ( 'NONE', #3315 ) ;
#27619 = CARTESIAN_POINT ( 'NONE',  ( 6.000000000000000000, -29.01471420065616513, 76.69515212746007649 ) ) ;
#27620 = ORIENTED_EDGE ( 'NONE', *, *, #28693, .F. ) ;
#27621 = VECTOR ( 'NONE', #15569, 1000.000000000000114 ) ;
#27622 = VECTOR ( 'NONE', #4853, 1000.000000000000000 ) ;
#27623 = CARTESIAN_POINT ( 'NONE',  ( 5.000000000000000000, -67.80270845531921964, 46.11716303203163392 ) ) ;
#27624 = VECTOR ( 'NONE', #34164, 1000.000000000000000 ) ;
#27625 = DIRECTION ( 'NONE',  ( 1.000000000000000000, 0.000000000000000000, 0.000000000000000000 ) ) ;
#27626 = DIRECTION ( 'NONE',  ( 0.000000000000000000, 0.3090169943749482839, -0.9510565162951533091 ) ) ;
#27627 = DIRECTION ( 'NONE',  ( 0.000000000000000000, -0.9510565162951500895, -0.3090169943749581649 ) ) ;
#27628 = CIRCLE ( 'NONE', #22161, 12.49999999999999645 ) ;
#27629 = ORIENTED_EDGE ( 'NONE', *, *, #7345, .F. ) ;
#27630 = CARTESIAN_POINT ( 'NONE',  ( -10.43921258969510824, -98.89258801967538659, -5.500000000000000000 ) ) ;
#27631 = CARTESIAN_POINT ( 'NONE',  ( 5.000000000000000000, -32.34446384429989507, 26.79245525562703278 ) ) ;
#27632 = AXIS2_PLACEMENT_3D ( 'NONE', #32411, #47337, #17210 ) ;
#27633 = CIRCLE ( 'NONE', #6517, 42.00000000000000000 ) ;
#27634 = CARTESIAN_POINT ( 'NONE',  ( 11.99999999999999822, 0.000000000000000000, 0.000000000000000000 ) ) ;
#27635 = CARTESIAN_POINT ( 'NONE',  ( 10.00000000000000000, 37.22597642581158084, -5.202137450156524068 ) ) ;
#27636 = ORIENTED_EDGE ( 'NONE', *, *, #42394, .T. ) ;
#27637 = EDGE_CURVE ( 'NONE', #32290, #26557, #6524, .T. ) ;
#27638 = CIRCLE ( 'NONE', #7282, 11.59999999999999787 ) ;
#27639 = DIRECTION ( 'NONE',  ( 0.000000000000000000, 0.000000000000000000, -1.000000000000000000 ) ) ;
#27640 = EDGE_CURVE ( 'NONE', #14073, #371, #33610, .T. ) ;
#27641 = CIRCLE ( 'NONE', #33878, 31.99999999999998579 ) ;
#27642 = ORIENTED_EDGE ( 'NONE', *, *, #43118, .F. ) ;
#27643 = DIRECTION ( 'NONE',  ( -1.000000000000000000, -0.000000000000000000, -0.000000000000000000 ) ) ;
#27644 = EDGE_CURVE ( 'NONE', #10301, #43899, #14837, .T. ) ;
#27645 = ADVANCED_FACE ( 'NONE', ( #29520 ), #29754, .F. ) ;
#27646 = CARTESIAN_POINT ( 'NONE',  ( 10.00000000000000000, 0.000000000000000000, 0.000000000000000000 ) ) ;
#27647 = DIRECTION ( 'NONE',  ( 0.000000000000000000, 0.3826834323650841752, 0.9238795325112891810 ) ) ;
#27648 = ORIENTED_EDGE ( 'NONE', *, *, #11743, .F. ) ;
#27649 = CIRCLE ( 'NONE', #10455, 31.99999999999999289 ) ;
#27650 = EDGE_LOOP ( 'NONE', ( #10689, #10758, #46690, #33183 ) ) ;
#27651 = DIRECTION ( 'NONE',  ( 0.000000000000000000, 0.000000000000000000, 1.000000000000000000 ) ) ;
#27652 = CONICAL_SURFACE ( 'NONE', #17464, 17.45460580326810174, 1.361356816555583826 ) ;
#27653 = AXIS2_PLACEMENT_3D ( 'NONE', #43980, #14621, #40075 ) ;
#27655 = ORIENTED_EDGE ( 'NONE', *, *, #21742, .T. ) ;
#27654 = AXIS2_PLACEMENT_3D ( 'NONE', #20582, #16926, #35277 ) ;
#27656 = ORIENTED_EDGE ( 'NONE', *, *, #43763, .F. ) ;
#27657 = ORIENTED_EDGE ( 'NONE', *, *, #21808, .T. ) ;
#27658 = ORIENTED_EDGE ( 'NONE', *, *, #6102, .F. ) ;
#27659 = CARTESIAN_POINT ( 'NONE',  ( 10.00000000000000000, 0.000000000000000000, 0.000000000000000000 ) ) ;
#27660 = CIRCLE ( 'NONE', #11240, 31.99999999999998579 ) ;
#27661 = CIRCLE ( 'NONE', #32388, 77.49900000000000944 ) ;
#27662 = EDGE_LOOP ( 'NONE', ( #4450, #22901, #32829, #26768 ) ) ;
#27663 = CARTESIAN_POINT ( 'NONE',  ( -1.250000000000000444, -16.78109714094927085, 0.000000000000000000 ) ) ;
#27664 = ORIENTED_EDGE ( 'NONE', *, *, #44818, .F. ) ;
#27665 = VECTOR ( 'NONE', #13006, 1000.000000000000000 ) ;
#27666 = DIRECTION ( 'NONE',  ( 0.000000000000000000, 0.000000000000000000, 1.000000000000000000 ) ) ;
#27667 = VECTOR ( 'NONE', #13744, 1000.000000000000000 ) ;
#27668 = DIRECTION ( 'NONE',  ( 0.000000000000000000, 0.000000000000000000, 1.000000000000000000 ) ) ;
#27669 = FACE_OUTER_BOUND ( 'NONE', #19639, .T. ) ;
#27671 = EDGE_LOOP ( 'NONE', ( #40852, #31044, #27435, #11681 ) ) ;
#27670 = CIRCLE ( 'NONE', #21405, 31.99999999999999289 ) ;
#27672 = CARTESIAN_POINT ( 'NONE',  ( 11.99999999999999822, 0.000000000000000000, 77.49899999999999523 ) ) ;
#27673 = EDGE_LOOP ( 'NONE', ( #10579, #21919, #10499, #27052 ) ) ;
#27674 = VERTEX_POINT ( 'NONE', #3811 ) ;
#27675 = DIRECTION ( 'NONE',  ( -0.000000000000000000, -0.000000000000000000, 1.000000000000000000 ) ) ;
#27676 = CYLINDRICAL_SURFACE ( 'NONE', #28973, 77.49899999999999523 ) ;
#27677 = ORIENTED_EDGE ( 'NONE', *, *, #14370, .T. ) ;
#27678 = CARTESIAN_POINT ( 'NONE',  ( 0.000000000000000000, 0.000000000000000000, 0.000000000000000000 ) ) ;
#27679 = ORIENTED_EDGE ( 'NONE', *, *, #20353, .F. ) ;
#27680 = ORIENTED_EDGE ( 'NONE', *, *, #20213, .T. ) ;
#27681 = DIRECTION ( 'NONE',  ( 0.000000000000000000, 0.5877852522924689183, -0.8090169943749504489 ) ) ;
#27682 = DIRECTION ( 'NONE',  ( -1.000000000000000000, 0.000000000000000000, 0.000000000000000000 ) ) ;
#27683 = EDGE_CURVE ( 'NONE', #41443, #42392, #37100, .T. ) ;
#27684 = CYLINDRICAL_SURFACE ( 'NONE', #45676, 82.00000000000000000 ) ;
#27685 = DIRECTION ( 'NONE',  ( -1.000000000000000000, 0.000000000000000000, 0.000000000000000000 ) ) ;
#27686 = DIRECTION ( 'NONE',  ( -1.000000000000000000, 0.000000000000000000, -0.000000000000000000 ) ) ;
#27687 = ADVANCED_FACE ( 'NONE', ( #40774 ), #21920, .T. ) ;
#27688 = DIRECTION ( 'NONE',  ( 0.000000000000000000, -0.5877852522924779111, -0.8090169943749440096 ) ) ;
#27689 = DIRECTION ( 'NONE',  ( 0.000000000000000000, 0.000000000000000000, 1.000000000000000000 ) ) ;
#27690 = AXIS2_PLACEMENT_3D ( 'NONE', #44978, #11461, #26379 ) ;
#27691 = CARTESIAN_POINT ( 'NONE',  ( 0.000000000000000000, -62.20884554314051229, 46.21855187248609553 ) ) ;
#27692 = EDGE_LOOP ( 'NONE', ( #20059, #21846, #14719, #7849 ) ) ;
#27693 = CIRCLE ( 'NONE', #13600, 16.00000000000000355 ) ;
#27694 = DIRECTION ( 'NONE',  ( 0.000000000000000000, -0.4539904997395351471, -0.8910065241883737830 ) ) ;
#27695 = DIRECTION ( 'NONE',  ( 0.08130631524010117905, -0.9966891607226784355, 0.000000000000000000 ) ) ;
#27696 = DIRECTION ( 'NONE',  ( 1.000000000000000000, 0.000000000000000000, 0.000000000000000000 ) ) ;
#27697 = VECTOR ( 'NONE', #13060, 1000.000000000000000 ) ;
#27698 = AXIS2_PLACEMENT_3D ( 'NONE', #21176, #16555, #9681 ) ;
#27699 = PLANE ( 'NONE',  #17429 ) ;
#27701 = CIRCLE ( 'NONE', #36956, 31.99999999999998579 ) ;
#27700 = DIRECTION ( 'NONE',  ( 0.000000000000000000, -0.8090169943749530024, 0.5877852522924653655 ) ) ;
#27702 = CARTESIAN_POINT ( 'NONE',  ( 11.99999999999999822, -74.65491531819111515, 23.16904090965678265 ) ) ;
#27703 = EDGE_CURVE ( 'NONE', #12027, #12600, #40679, .T. ) ;
#27704 = DIRECTION ( 'NONE',  ( -1.000000000000000000, -0.000000000000000000, -0.000000000000000000 ) ) ;
#27705 = EDGE_CURVE ( 'NONE', #25524, #46560, #2844, .T. ) ;
#27706 = VERTEX_POINT ( 'NONE', #10191 ) ;
#27707 = ADVANCED_FACE ( 'NONE', ( #10433 ), #6996, .T. ) ;
#27708 = VERTEX_POINT ( 'NONE', #17770 ) ;
#27709 = CARTESIAN_POINT ( 'NONE',  ( 10.00000000000000000, 0.000000000000000000, 0.000000000000000000 ) ) ;
#27710 = AXIS2_PLACEMENT_3D ( 'NONE', #6134, #14190, #36694 ) ;
#27711 = FACE_OUTER_BOUND ( 'NONE', #6539, .T. ) ;
#27712 = EDGE_CURVE ( 'NONE', #33012, #962, #29739, .T. ) ;
#27713 = CIRCLE ( 'NONE', #11329, 32.00000000000000000 ) ;
#27714 = APPLICATION_PROTOCOL_DEFINITION ( 'draft international standard', 'automotive_design', 1998, #20072 ) ;
#27715 = EDGE_CURVE ( 'NONE', #5563, #27123, #47626, .T. ) ;
#27716 = DIRECTION ( 'NONE',  ( -1.000000000000000000, -0.000000000000000000, -0.000000000000000000 ) ) ;
#27717 = CIRCLE ( 'NONE', #8172, 31.99999999999997868 ) ;
#27718 = VERTEX_POINT ( 'NONE', #36610 ) ;
#27719 = ORIENTED_EDGE ( 'NONE', *, *, #23530, .T. ) ;
#27720 = DIRECTION ( 'NONE',  ( 0.000000000000000000, 0.8090169943749445647, 0.5877852522924770229 ) ) ;
#27721 = EDGE_CURVE ( 'NONE', #352, #14857, #43961, .T. ) ;
#27722 = ORIENTED_EDGE ( 'NONE', *, *, #48241, .F. ) ;
#27723 = LINE ( 'NONE', #1528, #30526 ) ;
#27724 = CIRCLE ( 'NONE', #17536, 82.00000000000000000 ) ;
#27725 = CARTESIAN_POINT ( 'NONE',  ( 0.000000000000000000, -37.58145647212455032, 0.6853352020789044152 ) ) ;
#27726 = DIRECTION ( 'NONE',  ( -1.000000000000000000, 0.000000000000000000, -0.000000000000000000 ) ) ;
#27727 = EDGE_LOOP ( 'NONE', ( #19811, #46391, #16362, #43021 ) ) ;
#27728 = VECTOR ( 'NONE', #17997, 1000.000000000000114 ) ;
#27729 = CARTESIAN_POINT ( 'NONE',  ( 15.00000000000000000, 5.835314593368777558, 22.81335362449846471 ) ) ;
#27730 = CIRCLE ( 'NONE', #30062, 12.85999999999999943 ) ;
#27731 = VERTEX_POINT ( 'NONE', #29282 ) ;
#27732 = ORIENTED_EDGE ( 'NONE', *, *, #35252, .F. ) ;
#27733 = DIRECTION ( 'NONE',  ( 0.000000000000000000, 0.000000000000000000, 1.000000000000000000 ) ) ;
#27734 = DIRECTION ( 'NONE',  ( -1.000000000000000000, -0.000000000000000000, -0.000000000000000000 ) ) ;
#27735 = CARTESIAN_POINT ( 'NONE',  ( 11.99999999999999822, 64.81221759200417409, -50.23322058963275794 ) ) ;
#27736 = EDGE_CURVE ( 'NONE', #9130, #14954, #2375, .T. ) ;
#27737 = CARTESIAN_POINT ( 'NONE',  ( -12.00000000000000000, 0.000000000000000000, 0.000000000000000000 ) ) ;
#27738 = DIRECTION ( 'NONE',  ( -1.000000000000000000, -0.000000000000000000, 0.000000000000000000 ) ) ;
#27739 = EDGE_CURVE ( 'NONE', #37732, #20800, #15658, .T. ) ;
#27740 = CIRCLE ( 'NONE', #29307, 37.49900000000000944 ) ;
#27741 = CIRCLE ( 'NONE', #5870, 42.00000000000000000 ) ;
#27742 = ORIENTED_EDGE ( 'NONE', *, *, #22979, .F. ) ;
#27743 = DIRECTION ( 'NONE',  ( 1.000000000000000000, 0.000000000000000000, 0.000000000000000000 ) ) ;
#27744 = EDGE_LOOP ( 'NONE', ( #6531, #2193, #9573, #39207 ) ) ;
#27745 = VERTEX_POINT ( 'NONE', #15073 ) ;
#27746 = CIRCLE ( 'NONE', #8972, 12.50000000000000000 ) ;
#27747 = DIRECTION ( 'NONE',  ( 0.000000000000000000, 0.000000000000000000, -1.000000000000000000 ) ) ;
#27748 = AXIS2_PLACEMENT_3D ( 'NONE', #9391, #13810, #20405 ) ;
#27749 = VERTEX_POINT ( 'NONE', #38079 ) ;
#27750 = EDGE_CURVE ( 'NONE', #33596, #17439, #34375, .T. ) ;
#27751 = DIRECTION ( 'NONE',  ( 1.000000000000000000, 0.000000000000000000, 0.000000000000000000 ) ) ;
#27752 = AXIS2_PLACEMENT_3D ( 'NONE', #46823, #5958, #2260 ) ;
#27753 = CARTESIAN_POINT ( 'NONE',  ( 7.001685179585692254, -14.98378029539707512, 0.000000000000000000 ) ) ;
#27754 = DIRECTION ( 'NONE',  ( -1.000000000000000000, -0.000000000000000000, 0.000000000000000000 ) ) ;
#27755 = EDGE_LOOP ( 'NONE', ( #42657, #1400, #4727, #43258 ) ) ;
#27756 = DIRECTION ( 'NONE',  ( -1.000000000000000000, 0.000000000000000000, -0.000000000000000000 ) ) ;
#27757 = EDGE_CURVE ( 'NONE', #37621, #44069, #38309, .T. ) ;
#27758 = AXIS2_PLACEMENT_3D ( 'NONE', #28990, #29245, #43464 ) ;
#27759 = CARTESIAN_POINT ( 'NONE',  ( 0.000000000000000000, 30.84782396557217865, 21.32104025579125306 ) ) ;
#27760 = DIRECTION ( 'NONE',  ( 1.000000000000000000, 0.000000000000000000, 0.000000000000000000 ) ) ;
#27761 = CARTESIAN_POINT ( 'NONE',  ( 5.000000000000000000, 15.48615015657637706, -39.04073710021327770 ) ) ;
#27762 = DIRECTION ( 'NONE',  ( 1.000000000000000000, 0.000000000000000000, 0.000000000000000000 ) ) ;
#27763 = DIRECTION ( 'NONE',  ( 1.000000000000000000, 0.000000000000000000, 0.000000000000000000 ) ) ;
#27764 = FACE_OUTER_BOUND ( 'NONE', #42172, .T. ) ;
#27765 = DIRECTION ( 'NONE',  ( -1.000000000000000000, -0.000000000000000000, 0.000000000000000000 ) ) ;
#27766 = CARTESIAN_POINT ( 'NONE',  ( 12.00000000000000000, 26.49999999999999645, 1.499999999999995781 ) ) ;
#27767 = CARTESIAN_POINT ( 'NONE',  ( 0.000000000000000000, -75.16055320797016748, -18.89407956138335365 ) ) ;
#27768 = EDGE_CURVE ( 'NONE', #47099, #28193, #4722, .T. ) ;
#27769 = ORIENTED_EDGE ( 'NONE', *, *, #29788, .F. ) ;
#27770 = EDGE_CURVE ( 'NONE', #36144, #19393, #27377, .T. ) ;
#27771 = AXIS2_PLACEMENT_3D ( 'NONE', #16600, #46476, #1933 ) ;
#27772 = DIRECTION ( 'NONE',  ( 0.000000000000000000, -0.4067366430758009854, 0.9135454576426004225 ) ) ;
#27773 = ORIENTED_EDGE ( 'NONE', *, *, #5709, .T. ) ;
#27774 = DIRECTION ( 'NONE',  ( 0.000000000000000000, 0.000000000000000000, 1.000000000000000000 ) ) ;
#27775 = AXIS2_PLACEMENT_3D ( 'NONE', #10387, #10644, #25552 ) ;
#27776 = CARTESIAN_POINT ( 'NONE',  ( 0.000000000000000000, 0.000000000000000000, 0.000000000000000000 ) ) ;
#27777 = ORIENTED_EDGE ( 'NONE', *, *, #42164, .F. ) ;
#27778 = ADVANCED_FACE ( 'NONE', ( #852 ), #22648, .T. ) ;
#27779 = VECTOR ( 'NONE', #12854, 999.9999999999998863 ) ;
#27780 = CIRCLE ( 'NONE', #6662, 31.99999999999999289 ) ;
#27781 = CARTESIAN_POINT ( 'NONE',  ( 0.000000000000000000, -50.95692526931286181, -58.39081064771806240 ) ) ;
#27782 = ORIENTED_EDGE ( 'NONE', *, *, #8553, .F. ) ;
#27783 = ORIENTED_EDGE ( 'NONE', *, *, #9893, .F. ) ;
#27784 = AXIS2_PLACEMENT_3D ( 'NONE', #20198, #31476, #12868 ) ;
#27785 = VECTOR ( 'NONE', #28379, 1000.000000000000000 ) ;
#27786 = AXIS2_PLACEMENT_3D ( 'NONE', #24800, #32390, #40457 ) ;
#27787 = DIRECTION ( 'NONE',  ( 1.000000000000000000, 0.000000000000000000, 0.000000000000000000 ) ) ;
#27788 = DIRECTION ( 'NONE',  ( -1.000000000000000000, 0.000000000000000000, 0.000000000000000000 ) ) ;
#27790 = ORIENTED_EDGE ( 'NONE', *, *, #24858, .T. ) ;
#27789 = DIRECTION ( 'NONE',  ( -1.000000000000000000, 0.000000000000000000, 0.000000000000000000 ) ) ;
#27791 = ORIENTED_EDGE ( 'NONE', *, *, #23541, .T. ) ;
#27792 = CARTESIAN_POINT ( 'NONE',  ( 0.000000000000000000, 0.000000000000000000, 125.0000000000000000 ) ) ;
#27793 = VECTOR ( 'NONE', #14197, 1000.000000000000000 ) ;
#27794 = ORIENTED_EDGE ( 'NONE', *, *, #33696, .T. ) ;
#27795 = ORIENTED_EDGE ( 'NONE', *, *, #13114, .T. ) ;
#27796 = DIRECTION ( 'NONE',  ( 1.000000000000000000, -0.000000000000000000, -0.000000000000000000 ) ) ;
#27797 = DIRECTION ( 'NONE',  ( -1.000000000000000000, 0.000000000000000000, 0.000000000000000000 ) ) ;
#27798 = CARTESIAN_POINT ( 'NONE',  ( 10.00000000000000000, 0.000000000000000000, 0.000000000000000000 ) ) ;
#27799 = CIRCLE ( 'NONE', #23871, 37.49900000000000233 ) ;
#27800 = VERTEX_POINT ( 'NONE', #37585 ) ;
#27801 = EDGE_CURVE ( 'NONE', #15279, #13859, #19221, .T. ) ;
#27802 = ORIENTED_EDGE ( 'NONE', *, *, #7204, .F. ) ;
#27803 = ORIENTED_EDGE ( 'NONE', *, *, #35555, .T. ) ;
#27804 = CYLINDRICAL_SURFACE ( 'NONE', #39627, 37.49900000000000233 ) ;
#27805 = EDGE_LOOP ( 'NONE', ( #41403, #41756, #34136, #15444 ) ) ;
#27806 = CARTESIAN_POINT ( 'NONE',  ( 0.000000000000000000, -0.9646360437375307573, 23.52805723605590060 ) ) ;
#27807 = EDGE_CURVE ( 'NONE', #7974, #37702, #10173, .T. ) ;
#27808 = CYLINDRICAL_SURFACE ( 'NONE', #357, 12.49999999999999645 ) ;
#27809 = CYLINDRICAL_SURFACE ( 'NONE', #23659, 31.99999999999999289 ) ;
#27810 = CARTESIAN_POINT ( 'NONE',  ( -11.63999999999999702, 0.000000000000000000, 0.000000000000000000 ) ) ;
#27811 = DIRECTION ( 'NONE',  ( 0.000000000000000000, 0.5877852522924797984, 0.8090169943749426773 ) ) ;
#27812 = CARTESIAN_POINT ( 'NONE',  ( 10.00000000000000000, -33.79645857604525361, 16.45098606841114730 ) ) ;
#27813 = EDGE_CURVE ( 'NONE', #13396, #6444, #28822, .T. ) ;
#27814 = CARTESIAN_POINT ( 'NONE',  ( 10.00000000000000000, 0.000000000000000000, 0.000000000000000000 ) ) ;
#27815 = ORIENTED_EDGE ( 'NONE', *, *, #39649, .F. ) ;
#27816 = CARTESIAN_POINT ( 'NONE',  ( 0.000000000000000000, 24.81905959214261514, 9.408202855044825341 ) ) ;
#27817 = CARTESIAN_POINT ( 'NONE',  ( 10.00000000000000000, -22.74946021919110706, -29.81001611431033282 ) ) ;
#27818 = DIRECTION ( 'NONE',  ( 1.000000000000000000, -0.000000000000000000, -0.000000000000000000 ) ) ;
#27819 = LINE ( 'NONE', #5526, #34784 ) ;
#27820 = VECTOR ( 'NONE', #19391, 1000.000000000000114 ) ;
#27821 = AXIS2_PLACEMENT_3D ( 'NONE', #40197, #14238, #9844 ) ;
#27822 = EDGE_LOOP ( 'NONE', ( #2538, #3677, #16349, #14711 ) ) ;
#27823 = CARTESIAN_POINT ( 'NONE',  ( 10.00000000000000000, -46.21855187248583974, -62.20884554314070414 ) ) ;
#27824 = AXIS2_PLACEMENT_3D ( 'NONE', #17018, #6024, #2328 ) ;
#27825 = DIRECTION ( 'NONE',  ( 0.000000000000000000, 0.000000000000000000, 1.000000000000000000 ) ) ;
#27826 = CARTESIAN_POINT ( 'NONE',  ( 12.00000000000000000, -13.04903810567675393, -19.60159698893424718 ) ) ;
#27827 = EDGE_CURVE ( 'NONE', #28563, #45738, #46941, .T. ) ;
#27828 = ADVANCED_FACE ( 'NONE', ( #45906 ), #4781, .T. ) ;
#27829 = DIRECTION ( 'NONE',  ( 0.000000000000000000, -0.8526401643540970632, 0.5224985647159411384 ) ) ;
#27830 = LINE ( 'NONE', #16553, #39729 ) ;
#27831 = ORIENTED_EDGE ( 'NONE', *, *, #15794, .F. ) ;
#27832 = DIRECTION ( 'NONE',  ( 0.000000000000000000, 0.000000000000000000, 1.000000000000000000 ) ) ;
#27833 = CARTESIAN_POINT ( 'NONE',  ( 0.000000000000000000, 77.19088730480524418, 6.903761155838049390 ) ) ;
#27834 = EDGE_CURVE ( 'NONE', #18858, #7802, #23139, .T. ) ;
#27835 = ORIENTED_EDGE ( 'NONE', *, *, #22543, .F. ) ;
#27836 = DIRECTION ( 'NONE',  ( -0.000000000000000000, -0.000000000000000000, 1.000000000000000000 ) ) ;
#27837 = AXIS2_PLACEMENT_3D ( 'NONE', #42223, #13100, #31957 ) ;
#27838 = VERTEX_POINT ( 'NONE', #42218 ) ;
#27839 =( NAMED_UNIT ( * ) SI_UNIT ( $, .STERADIAN. ) SOLID_ANGLE_UNIT ( ) );
#27840 = AXIS2_PLACEMENT_3D ( 'NONE', #8184, #4033, #33635 ) ;
#27841 = DIRECTION ( 'NONE',  ( -1.000000000000000000, 0.000000000000000000, 0.000000000000000000 ) ) ;
#27842 = ORIENTED_EDGE ( 'NONE', *, *, #20053, .T. ) ;
#27843 = VERTEX_POINT ( 'NONE', #19682 ) ;
#27844 = EDGE_CURVE ( 'NONE', #47293, #7344, #35991, .T. ) ;
#27845 = AXIS2_PLACEMENT_3D ( 'NONE', #38461, #1002, #4924 ) ;
#27846 = EDGE_LOOP ( 'NONE', ( #20989, #32768, #31657, #13871 ) ) ;
#27847 = ORIENTED_EDGE ( 'NONE', *, *, #40960, .F. ) ;
#27848 = CARTESIAN_POINT ( 'NONE',  ( 0.000000000000000000, -50.23322058963393744, 64.81221759200325039 ) ) ;
#27849 =( GEOMETRIC_REPRESENTATION_CONTEXT ( 3 ) GLOBAL_UNCERTAINTY_ASSIGNED_CONTEXT ( ( #25690 ) ) GLOBAL_UNIT_ASSIGNED_CONTEXT ( ( #19970, #35135, #8703 ) ) REPRESENTATION_CONTEXT ( 'NONE', 'WORKASPACE' ) );
#27850 = EDGE_LOOP ( 'NONE', ( #37333, #45411, #32524, #40943 ) ) ;
#27851 = ORIENTED_EDGE ( 'NONE', *, *, #14886, .F. ) ;
#27852 = VECTOR ( 'NONE', #23495, 1000.000000000000000 ) ;
#27853 = LINE ( 'NONE', #34674, #13260 ) ;
#27854 = DIRECTION ( 'NONE',  ( -1.000000000000000000, 0.000000000000000000, -0.000000000000000000 ) ) ;
#27855 = ORIENTED_EDGE ( 'NONE', *, *, #21438, .F. ) ;
#27856 = AXIS2_PLACEMENT_3D ( 'NONE', #45876, #12344, #23577 ) ;
#27857 = ORIENTED_EDGE ( 'NONE', *, *, #10774, .F. ) ;
#27858 = ORIENTED_EDGE ( 'NONE', *, *, #33734, .T. ) ;
#27859 = AXIS2_PLACEMENT_3D ( 'NONE', #26472, #41406, #11782 ) ;
#27860 = LINE ( 'NONE', #5087, #32683 ) ;
#27862 = ORIENTED_EDGE ( 'NONE', *, *, #23862, .F. ) ;
#27861 = CARTESIAN_POINT ( 'NONE',  ( 10.00000000000000000, 62.20884554314020676, 46.21855187248652896 ) ) ;
#27863 = CARTESIAN_POINT ( 'NONE',  ( -10.00000000000000000, 0.000000000000000000, 0.000000000000000000 ) ) ;
#27864 = ORIENTED_EDGE ( 'NONE', *, *, #25962, .T. ) ;
#27865 = DIRECTION ( 'NONE',  ( 0.000000000000000000, 0.1564344650402312298, -0.9876883405951375483 ) ) ;
#27866 = ORIENTED_EDGE ( 'NONE', *, *, #27409, .F. ) ;
#27867 = ORIENTED_EDGE ( 'NONE', *, *, #34817, .F. ) ;
#27868 = CARTESIAN_POINT ( 'NONE',  ( 11.99999999999999822, 73.44644590900061587, 24.73286445877730699 ) ) ;
#27869 = CARTESIAN_POINT ( 'NONE',  ( 11.99999999999999822, 74.65491531819105830, 8.830959090343693418 ) ) ;
#27870 = VERTEX_POINT ( 'NONE', #30002 ) ;
#27871 = EDGE_CURVE ( 'NONE', #3690, #30765, #44935, .T. ) ;
#27872 = CIRCLE ( 'NONE', #34092, 77.49900000000000944 ) ;
#27873 = CARTESIAN_POINT ( 'NONE',  ( 10.00000000000000000, 0.000000000000000000, 0.000000000000000000 ) ) ;
#27874 = DIRECTION ( 'NONE',  ( 1.000000000000000000, 0.000000000000000000, 0.000000000000000000 ) ) ;
#27875 = CARTESIAN_POINT ( 'NONE',  ( 15.00000000000000000, -23.29833615347104470, 3.418703333116808629 ) ) ;
#27876 = AXIS2_PLACEMENT_3D ( 'NONE', #41943, #19631, #1038 ) ;
#27877 = EDGE_CURVE ( 'NONE', #45643, #2188, #34408, .T. ) ;
#27878 = ORIENTED_EDGE ( 'NONE', *, *, #24309, .F. ) ;
#27879 = EDGE_CURVE ( 'NONE', #38615, #13555, #21904, .T. ) ;
#27880 = EDGE_LOOP ( 'NONE', ( #47156, #6580, #35249, #33561 ) ) ;
#27881 = DIRECTION ( 'NONE',  ( -1.000000000000000000, -0.000000000000000000, -0.000000000000000000 ) ) ;
#27882 = AXIS2_PLACEMENT_3D ( 'NONE', #30829, #45754, #26667 ) ;
#27883 = EDGE_CURVE ( 'NONE', #697, #21394, #798, .T. ) ;
#27884 = CARTESIAN_POINT ( 'NONE',  ( -12.50000000000000000, -132.5000000000000000, -40.00000000000000000 ) ) ;
#27886 = EDGE_CURVE ( 'NONE', #34677, #43252, #42209, .T. ) ;
#27885 = ORIENTED_EDGE ( 'NONE', *, *, #140, .F. ) ;
#27887 = VERTEX_POINT ( 'NONE', #1593 ) ;
#27888 = ADVANCED_FACE ( 'NONE', ( #8928 ), #5502, .T. ) ;
#27889 = DIRECTION ( 'NONE',  ( 0.000000000000000000, -0.4067366430758009854, 0.9135454576426004225 ) ) ;
#27890 = ORIENTED_EDGE ( 'NONE', *, *, #17936, .T. ) ;
#27891 = CARTESIAN_POINT ( 'NONE',  ( 11.99999999999999822, 22.90783923731740401, -78.73519480814930205 ) ) ;
#27892 = CARTESIAN_POINT ( 'NONE',  ( 0.000000000000000000, -120.0000000000000000, -2.500000000000000000 ) ) ;
#27893 = DIRECTION ( 'NONE',  ( 0.000000000000000000, 0.000000000000000000, 1.000000000000000000 ) ) ;
#27894 = LINE ( 'NONE', #42809, #2555 ) ;
#27895 = CARTESIAN_POINT ( 'NONE',  ( 0.000000000000000000, -21.53537804866103045, 30.80686688397002371 ) ) ;
#27896 = DIRECTION ( 'NONE',  ( 0.000000000000000000, 0.8090169943749486725, -0.5877852522924713607 ) ) ;
#27897 = AXIS2_PLACEMENT_3D ( 'NONE', #43506, #39834, #28320 ) ;
#27898 = DIRECTION ( 'NONE',  ( 0.000000000000000000, 0.000000000000000000, 1.000000000000000000 ) ) ;
#27899 = DIRECTION ( 'NONE',  ( -1.000000000000000000, -0.000000000000000000, 0.000000000000000000 ) ) ;
#27900 = DIRECTION ( 'NONE',  ( -1.000000000000000000, 0.000000000000000000, -0.000000000000000000 ) ) ;
#27901 = EDGE_CURVE ( 'NONE', #5822, #23903, #47098, .T. ) ;
#27902 = AXIS2_PLACEMENT_3D ( 'NONE', #14442, #29601, #7327 ) ;
#27903 = LINE ( 'NONE', #1944, #9631 ) ;
#27904 = ORIENTED_EDGE ( 'NONE', *, *, #47429, .T. ) ;
#27905 = EDGE_CURVE ( 'NONE', #47056, #38428, #41450, .T. ) ;
#27906 = ORIENTED_EDGE ( 'NONE', *, *, #41058, .T. ) ;
#27907 = CARTESIAN_POINT ( 'NONE',  ( 0.000000000000000000, 16.23288003029543347, -33.80338159004267595 ) ) ;
#27908 = AXIS2_PLACEMENT_3D ( 'NONE', #26121, #10222, #7530 ) ;
#27909 = DIRECTION ( 'NONE',  ( -0.000000000000000000, -0.2079116908177653378, 0.9781476007338044676 ) ) ;
#27910 = ORIENTED_EDGE ( 'NONE', *, *, #1973, .F. ) ;
#27911 = AXIS2_PLACEMENT_3D ( 'NONE', #29792, #15368, #44720 ) ;
#27912 = VERTEX_POINT ( 'NONE', #28508 ) ;
#27913 = EDGE_CURVE ( 'NONE', #39808, #32517, #37529, .T. ) ;
#27914 = CARTESIAN_POINT ( 'NONE',  ( -24.50849501662245800, -109.8101191361138831, 5.500000000000000000 ) ) ;
#27915 = ORIENTED_EDGE ( 'NONE', *, *, #2005, .F. ) ;
#27916 = ORIENTED_EDGE ( 'NONE', *, *, #31750, .F. ) ;
#27917 = ORIENTED_EDGE ( 'NONE', *, *, #25455, .T. ) ;
#27918 = AXIS2_PLACEMENT_3D ( 'NONE', #10887, #22136, #11615 ) ;
#27919 = EDGE_CURVE ( 'NONE', #5925, #21150, #22682, .T. ) ;
#27920 = DIRECTION ( 'NONE',  ( -1.000000000000000000, -0.000000000000000000, 0.000000000000000000 ) ) ;
#27921 = ORIENTED_EDGE ( 'NONE', *, *, #40117, .F. ) ;
#27922 = CARTESIAN_POINT ( 'NONE',  ( 10.00000000000000000, -77.19088730480528682, 6.903761155837488062 ) ) ;
#27923 = ORIENTED_EDGE ( 'NONE', *, *, #46973, .T. ) ;
#27924 = ADVANCED_FACE ( 'NONE', ( #12610 ), #39535, .T. ) ;
#27925 = LINE ( 'NONE', #16888, #1707 ) ;
#27926 = CONICAL_SURFACE ( 'NONE', #39663, 17.30399999999999849, 0.2094395102393129815 ) ;
#27927 = CARTESIAN_POINT ( 'NONE',  ( -23.97194136764370498, -131.3950000906648938, 5.500000000000000000 ) ) ;
#27928 = EDGE_CURVE ( 'NONE', #25303, #39296, #5494, .T. ) ;
#27929 = CARTESIAN_POINT ( 'NONE',  ( 10.00000000000000000, 37.01155633439068282, -6.555932627142014191 ) ) ;
#27930 = ORIENTED_EDGE ( 'NONE', *, *, #33154, .T. ) ;
#27931 = FACE_OUTER_BOUND ( 'NONE', #6897, .T. ) ;
#27932 = ORIENTED_EDGE ( 'NONE', *, *, #8824, .T. ) ;
#27933 = CARTESIAN_POINT ( 'NONE',  ( 10.00000000000000000, -36.13751322684434797, 21.40280677340358295 ) ) ;
#27934 = DIRECTION ( 'NONE',  ( 0.000000000000000000, -6.982962677686267499E-15, 1.000000000000000000 ) ) ;
#27935 = DIRECTION ( 'NONE',  ( 0.000000000000000000, 0.3090169943749480619, -0.9510565162951533091 ) ) ;
#27936 = VERTEX_POINT ( 'NONE', #2083 ) ;
#27937 = VERTEX_POINT ( 'NONE', #31951 ) ;
#27938 = EDGE_CURVE ( 'NONE', #25666, #13717, #13332, .T. ) ;
#27939 = DIRECTION ( 'NONE',  ( 0.000000000000000000, 0.000000000000000000, -1.000000000000000000 ) ) ;
#27940 = LINE ( 'NONE', #21276, #12134 ) ;
#27941 = ORIENTED_EDGE ( 'NONE', *, *, #33364, .T. ) ;
#27942 = PLANE ( 'NONE',  #1124 ) ;
#27943 = CARTESIAN_POINT ( 'NONE',  ( 11.99999999999999822, -70.53064760720336324, 26.01480285779810231 ) ) ;
#27944 = DIRECTION ( 'NONE',  ( 0.000000000000000000, 0.000000000000000000, 1.000000000000000000 ) ) ;
#27945 = CARTESIAN_POINT ( 'NONE',  ( 0.000000000000000000, -120.0000000000000000, 2.500000000000000000 ) ) ;
#27946 = LINE ( 'NONE', #3102, #32202 ) ;
#27947 = CIRCLE ( 'NONE', #43545, 37.49900000000000233 ) ;
#27948 = DIRECTION ( 'NONE',  ( 0.000000000000000000, 0.000000000000000000, 1.000000000000000000 ) ) ;
#27949 = DIRECTION ( 'NONE',  ( -1.000000000000000000, 0.000000000000000000, -0.000000000000000000 ) ) ;
#27950 = DIRECTION ( 'NONE',  ( -1.000000000000000000, 0.000000000000000000, 0.000000000000000000 ) ) ;
#27951 = DIRECTION ( 'NONE',  ( 0.000000000000000000, -0.9969173337331270757, -0.07845909572785580988 ) ) ;
#27952 = CARTESIAN_POINT ( 'NONE',  ( 10.00000000000000000, -26.02418014898260878, -70.52718814184285634 ) ) ;
#27953 = DIRECTION ( 'NONE',  ( -1.000000000000000000, 0.000000000000000000, -0.000000000000000000 ) ) ;
#27954 = FILL_AREA_STYLE ('',( #36229 ) ) ;
#27955 = DIRECTION ( 'NONE',  ( -1.000000000000000000, 0.000000000000000000, 0.000000000000000000 ) ) ;
#27956 = ORIENTED_EDGE ( 'NONE', *, *, #23706, .F. ) ;
#27957 = VECTOR ( 'NONE', #34101, 1000.000000000000000 ) ;
#27958 = CARTESIAN_POINT ( 'NONE',  ( 10.00000000000000000, 10.74501242461333028, -35.92658777277499382 ) ) ;
#27959 = CARTESIAN_POINT ( 'NONE',  ( 0.000000000000000000, -17.67226234102849958, 33.17418723428301774 ) ) ;
#27960 = VECTOR ( 'NONE', #21486, 1000.000000000000000 ) ;
#27961 = CARTESIAN_POINT ( 'NONE',  ( 0.000000000000000000, -36.88895765772628010, -6.736453364083947015 ) ) ;
#27962 = VERTEX_POINT ( 'NONE', #23864 ) ;
#27963 = AXIS2_PLACEMENT_3D ( 'NONE', #41189, #3723, #8113 ) ;
#27964 = CARTESIAN_POINT ( 'NONE',  ( 0.000000000000000000, -0.9646360437375307573, 23.52805723605590060 ) ) ;
#27965 = ORIENTED_EDGE ( 'NONE', *, *, #19931, .T. ) ;
#27966 = DIRECTION ( 'NONE',  ( -1.000000000000000000, 0.000000000000000000, 0.000000000000000000 ) ) ;
#27967 = EDGE_LOOP ( 'NONE', ( #17673, #14663, #28858, #4433 ) ) ;
#27968 = CARTESIAN_POINT ( 'NONE',  ( 10.00000000000000000, 21.53537804866081373, 30.80686688397018358 ) ) ;
#27969 = CIRCLE ( 'NONE', #11541, 77.49899999999999523 ) ;
#27970 = DIRECTION ( 'NONE',  ( 0.000000000000000000, 0.000000000000000000, 1.000000000000000000 ) ) ;
#27971 = DIRECTION ( 'NONE',  ( -1.000000000000000000, 0.000000000000000000, 0.000000000000000000 ) ) ;
#27972 = ORIENTED_EDGE ( 'NONE', *, *, #18523, .F. ) ;
#27973 = ADVANCED_FACE ( 'NONE', ( #38810 ), #39271, .F. ) ;
#27974 = DIRECTION ( 'NONE',  ( 0.000000000000000000, 0.1564344650402243742, 0.9876883405951387696 ) ) ;
#27975 = ORIENTED_EDGE ( 'NONE', *, *, #46910, .F. ) ;
#27976 = EDGE_CURVE ( 'NONE', #39765, #34109, #30539, .T. ) ;
#27977 = LINE ( 'NONE', #23807, #13434 ) ;
#27978 = FACE_OUTER_BOUND ( 'NONE', #45120, .T. ) ;
#27979 = CARTESIAN_POINT ( 'NONE',  ( 0.000000000000000000, 37.48860685352291000, 0.8828120875901893649 ) ) ;
#27980 = CARTESIAN_POINT ( 'NONE',  ( 10.00000000000000000, 50.23322058963440639, -64.81221759200288091 ) ) ;
#27982 = DIRECTION ( 'NONE',  ( 1.000000000000000000, 0.000000000000000000, 0.000000000000000000 ) ) ;
#27981 = CIRCLE ( 'NONE', #10783, 77.49899999999999523 ) ;
#27983 = ORIENTED_EDGE ( 'NONE', *, *, #27637, .F. ) ;
#27984 = DIRECTION ( 'NONE',  ( 0.000000000000000000, 0.000000000000000000, -1.000000000000000000 ) ) ;
#27985 = ORIENTED_EDGE ( 'NONE', *, *, #39829, .F. ) ;
#27986 = VERTEX_POINT ( 'NONE', #28257 ) ;
#27987 = EDGE_CURVE ( 'NONE', #38298, #42647, #43820, .T. ) ;
#27988 = FACE_OUTER_BOUND ( 'NONE', #13096, .T. ) ;
#27989 = VECTOR ( 'NONE', #48275, 1000.000000000000000 ) ;
#27990 = DIRECTION ( 'NONE',  ( 0.000000000000000000, 0.000000000000000000, 1.000000000000000000 ) ) ;
#27991 = ADVANCED_FACE ( 'NONE', ( #24828 ), #31464, .T. ) ;
#27992 = DIRECTION ( 'NONE',  ( -1.000000000000000000, -0.000000000000000000, 0.000000000000000000 ) ) ;
#27993 = DIRECTION ( 'NONE',  ( -1.000000000000000000, 0.000000000000000000, 0.000000000000000000 ) ) ;
#27994 = ORIENTED_EDGE ( 'NONE', *, *, #19126, .T. ) ;
#27995 = CARTESIAN_POINT ( 'NONE',  ( 11.99999999999999822, 17.28742895386189460, -75.54627589209927407 ) ) ;
#27996 = DIRECTION ( 'NONE',  ( -1.000000000000000000, -0.000000000000000000, -0.000000000000000000 ) ) ;
#27997 = FACE_OUTER_BOUND ( 'NONE', #40134, .T. ) ;
#27998 = DIRECTION ( 'NONE',  ( 0.000000000000000000, 0.3090169943749480064, -0.9510565162951534202 ) ) ;
#27999 = PLANE ( 'NONE',  #13004 ) ;
#28000 = DIRECTION ( 'NONE',  ( 0.000000000000000000, 0.8090169943749488946, -0.5877852522924712497 ) ) ;
#28001 = LINE ( 'NONE', #2057, #13436 ) ;
#28002 = LINE ( 'NONE', #39247, #28685 ) ;
#28003 = CARTESIAN_POINT ( 'NONE',  ( 0.000000000000000000, 0.000000000000000000, -1.199999999999999956 ) ) ;
#28004 = PLANE ( 'NONE',  #41741 ) ;
#28005 = COLOUR_RGB ( '', 0.66274510, 0.83137255, 0.94901961) ;
#28006 = ORIENTED_EDGE ( 'NONE', *, *, #2159, .F. ) ;
#28007 = CIRCLE ( 'NONE', #15489, 31.99999999999998934 ) ;
#28008 = LINE ( 'NONE', #39510, #9718 ) ;
#28009 = ORIENTED_EDGE ( 'NONE', *, *, #24502, .T. ) ;
#28010 = LINE ( 'NONE', #9386, #33121 ) ;
#28011 = DIRECTION ( 'NONE',  ( -1.000000000000000000, 0.000000000000000000, 0.000000000000000000 ) ) ;
#28012 = EDGE_LOOP ( 'NONE', ( #45477, #37354, #5146, #7359 ) ) ;
#28013 = EDGE_CURVE ( 'NONE', #16230, #36455, #13568, .T. ) ;
#28014 = EDGE_CURVE ( 'NONE', #20184, #18, #6232, .T. ) ;
#28015 = ADVANCED_FACE ( 'NONE', ( #21141 ), #1356, .F. ) ;
#28016 = DIRECTION ( 'NONE',  ( -1.000000000000000000, -0.000000000000000000, 0.000000000000000000 ) ) ;
#28017 = AXIS2_PLACEMENT_3D ( 'NONE', #42295, #1661, #16839 ) ;
#28018 = ORIENTED_EDGE ( 'NONE', *, *, #32701, .T. ) ;
#28019 = CIRCLE ( 'NONE', #45211, 31.99999999999999645 ) ;
#28020 = ORIENTED_EDGE ( 'NONE', *, *, #41350, .T. ) ;
#28021 = ADVANCED_FACE ( 'NONE', ( #9173 ), #16767, .T. ) ;
#28022 = LINE ( 'NONE', #46368, #24521 ) ;
#28023 = CARTESIAN_POINT ( 'NONE',  ( 0.000000000000000000, 23.50000000000000000, -1.500000000000001332 ) ) ;
#28024 = DIRECTION ( 'NONE',  ( -1.000000000000000000, 0.000000000000000000, 0.000000000000000000 ) ) ;
#28025 = ORIENTED_EDGE ( 'NONE', *, *, #28028, .T. ) ;
#28026 = CARTESIAN_POINT ( 'NONE',  ( 12.69589495141918611, -96.69089767102708777, 5.500000000000000000 ) ) ;
#28027 = AXIS2_PLACEMENT_3D ( 'NONE', #22351, #44856, #11085 ) ;
#28028 = EDGE_CURVE ( 'NONE', #7708, #17290, #33625, .T. ) ;
#28029 = ORIENTED_EDGE ( 'NONE', *, *, #26068, .T. ) ;
#28030 = ADVANCED_FACE ( 'NONE', ( #48319 ), #26298, .T. ) ;
#28031 = ADVANCED_FACE ( 'NONE', ( #7689 ), #29717, .T. ) ;
#28032 = DIRECTION ( 'NONE',  ( 0.000000000000000000, 0.9876883405951381034, -0.1564344650402276216 ) ) ;
#28033 = CARTESIAN_POINT ( 'NONE',  ( 11.41210121379328335, -99.40233154247455616, -5.500000000000000000 ) ) ;
#28034 = DIRECTION ( 'NONE',  ( 1.000000000000000000, -0.000000000000000000, -0.000000000000000000 ) ) ;
#28035 = CIRCLE ( 'NONE', #1448, 77.49899999999999523 ) ;
#28036 = EDGE_LOOP ( 'NONE', ( #37180, #167, #13749, #30423 ) ) ;
#28037 = ORIENTED_EDGE ( 'NONE', *, *, #3950, .F. ) ;
#28038 = CARTESIAN_POINT ( 'NONE',  ( 11.99999999999999822, -65.58780272294100655, 36.73666225445870737 ) ) ;
#28039 = ORIENTED_EDGE ( 'NONE', *, *, #17894, .F. ) ;
#28040 = FACE_BOUND ( 'NONE', #326, .T. ) ;
#28041 = DIRECTION ( 'NONE',  ( 0.000000000000000000, -0.9510565162951500895, -0.3090169943749583870 ) ) ;
#28042 = CARTESIAN_POINT ( 'NONE',  ( 10.00000000000000000, 0.000000000000000000, 0.000000000000000000 ) ) ;
#28043 = CARTESIAN_POINT ( 'NONE',  ( 0.000000000000000000, 67.80270845531887858, 46.11716303203210998 ) ) ;
#28044 = CARTESIAN_POINT ( 'NONE',  ( 11.59999999999999787, 1.420590287010929336E-15, -44.99999999999998579 ) ) ;
#28045 = DIRECTION ( 'NONE',  ( -0.000000000000000000, -0.000000000000000000, -1.000000000000000000 ) ) ;
#28046 = FACE_OUTER_BOUND ( 'NONE', #9944, .T. ) ;
#28047 = ORIENTED_EDGE ( 'NONE', *, *, #19217, .T. ) ;
#28049 = EDGE_CURVE ( 'NONE', #13273, #8092, #4024, .T. ) ;
#28048 = CARTESIAN_POINT ( 'NONE',  ( 10.00000000000000000, 0.000000000000000000, 0.000000000000000000 ) ) ;
#28050 = DIRECTION ( 'NONE',  ( -0.9966891607226785466, -0.08130631524010122069, 0.000000000000000000 ) ) ;
#28051 = CARTESIAN_POINT ( 'NONE',  ( -43.60332556124591008, -123.0000000000000142, 2.500000000000002220 ) ) ;
#28052 = VERTEX_POINT ( 'NONE', #26046 ) ;
#28053 = DIRECTION ( 'NONE',  ( 0.000000000000000000, 0.9876883405951371042, 0.1564344650402346715 ) ) ;
#28054 = AXIS2_PLACEMENT_3D ( 'NONE', #46497, #13198, #20527 ) ;
#28055 = CARTESIAN_POINT ( 'NONE',  ( -13.05994868825747446, -139.5943292883446532, 5.500000000000000000 ) ) ;
#28056 = CARTESIAN_POINT ( 'NONE',  ( -4.653126046682595884, -146.1313684676804314, 5.500000000000000000 ) ) ;
#28057 = AXIS2_PLACEMENT_3D ( 'NONE', #36795, #3262, #14050 ) ;
#28058 = DIRECTION ( 'NONE',  ( 0.000000000000000000, -0.8526401643540859610, -0.5224985647159591240 ) ) ;
#28059 = LINE ( 'NONE', #25514, #3751 ) ;
#28060 = DIRECTION ( 'NONE',  ( 0.000000000000000000, 0.000000000000000000, 1.000000000000000000 ) ) ;
#28061 = LINE ( 'NONE', #42989, #6577 ) ;
#28062 = VERTEX_POINT ( 'NONE', #11610 ) ;
#28063 = DIRECTION ( 'NONE',  ( 1.000000000000000000, 0.000000000000000000, 0.000000000000000000 ) ) ;
#28064 = ORIENTED_EDGE ( 'NONE', *, *, #788, .T. ) ;
#28065 =( NAMED_UNIT ( * ) SI_UNIT ( $, .STERADIAN. ) SOLID_ANGLE_UNIT ( ) );
#28066 = CARTESIAN_POINT ( 'NONE',  ( -10.00000000000000000, 0.000000000000000000, 0.000000000000000000 ) ) ;
#28067 = ORIENTED_EDGE ( 'NONE', *, *, #42753, .T. ) ;
#28068 = VERTEX_POINT ( 'NONE', #11381 ) ;
#28069 = EDGE_CURVE ( 'NONE', #21809, #8377, #18926, .T. ) ;
#28070 = VERTEX_POINT ( 'NONE', #7922 ) ;
#28071 = EDGE_CURVE ( 'NONE', #11938, #35871, #48083, .T. ) ;
#28072 = CARTESIAN_POINT ( 'NONE',  ( 10.00000000000000000, -33.80338159004273280, -16.23288003029533044 ) ) ;
#28073 = ORIENTED_EDGE ( 'NONE', *, *, #41835, .T. ) ;
#28074 = EDGE_CURVE ( 'NONE', #6779, #5309, #22710, .T. ) ;
#28075 = CARTESIAN_POINT ( 'NONE',  ( 11.99999999999999822, -33.71516098798793593, 74.74816331893418919 ) ) ;
#28077 = ORIENTED_EDGE ( 'NONE', *, *, #39812, .F. ) ;
#28076 = LINE ( 'NONE', #43009, #26153 ) ;
#28078 = VECTOR ( 'NONE', #12419, 1000.000000000000114 ) ;
#28079 = ORIENTED_EDGE ( 'NONE', *, *, #2298, .T. ) ;
#28080 = ORIENTED_EDGE ( 'NONE', *, *, #29900, .T. ) ;
#28081 = EDGE_LOOP ( 'NONE', ( #28430, #23135, #46904, #5971 ) ) ;
#28082 = EDGE_CURVE ( 'NONE', #43027, #33430, #11017, .T. ) ;
#28083 = EDGE_CURVE ( 'NONE', #32049, #29568, #37547, .T. ) ;
#28084 = DIRECTION ( 'NONE',  ( -1.000000000000000000, 0.000000000000000000, -0.000000000000000000 ) ) ;
#28086 = ORIENTED_EDGE ( 'NONE', *, *, #17385, .F. ) ;
#28085 = CARTESIAN_POINT ( 'NONE',  ( 0.000000000000000000, -67.80270845531855173, -46.11716303203261447 ) ) ;
#28087 = DIRECTION ( 'NONE',  ( 0.000000000000000000, 0.7071067811865439090, 0.7071067811865512365 ) ) ;
#28088 = ORIENTED_EDGE ( 'NONE', *, *, #36195, .F. ) ;
#28089 = VERTEX_POINT ( 'NONE', #11124 ) ;
#28090 = CARTESIAN_POINT ( 'NONE',  ( 4.999999999999999112, 38.55633173627034438, -16.65560815589369881 ) ) ;
#28091 = ORIENTED_EDGE ( 'NONE', *, *, #9893, .T. ) ;
#28092 = DIRECTION ( 'NONE',  ( -1.000000000000000000, 0.000000000000000000, 0.000000000000000000 ) ) ;
#28093 = LINE ( 'NONE', #43023, #6139 ) ;
#28094 = CARTESIAN_POINT ( 'NONE',  ( 0.000000000000000000, -73.72996012237429397, -14.67089635893794508 ) ) ;
#28095 = DIRECTION ( 'NONE',  ( -1.000000000000000000, 0.000000000000000000, -0.000000000000000000 ) ) ;
#28096 = FACE_OUTER_BOUND ( 'NONE', #16994, .T. ) ;
#28097 = VERTEX_POINT ( 'NONE', #14567 ) ;
#28098 = LINE ( 'NONE', #42304, #47729 ) ;
#28099 = ADVANCED_FACE ( 'NONE', ( #4278 ), #15292, .T. ) ;
#28100 = CARTESIAN_POINT ( 'NONE',  ( 10.00000000000000000, 0.000000000000000000, 0.000000000000000000 ) ) ;
#28101 = ORIENTED_EDGE ( 'NONE', *, *, #21248, .F. ) ;
#28102 = LINE ( 'NONE', #9732, #35057 ) ;
#28103 = ORIENTED_EDGE ( 'NONE', *, *, #15031, .F. ) ;
#28104 = DIRECTION ( 'NONE',  ( -1.000000000000000000, 0.000000000000000000, 0.000000000000000000 ) ) ;
#28105 = FACE_OUTER_BOUND ( 'NONE', #34493, .T. ) ;
#28106 = CARTESIAN_POINT ( 'NONE',  ( 5.000000000000000000, -56.15606465354917276, -59.75363087400133111 ) ) ;
#28107 = CARTESIAN_POINT ( 'NONE',  ( 10.00000000000000000, 33.17418723428307459, 17.67226234102837878 ) ) ;
#28108 = FACE_OUTER_BOUND ( 'NONE', #18663, .T. ) ;
#28109 = CARTESIAN_POINT ( 'NONE',  ( 10.00000000000000000, 65.64334221924909230, 41.19522573413756561 ) ) ;
#28110 = CIRCLE ( 'NONE', #24193, 31.99999999999998579 ) ;
#28111 = VERTEX_POINT ( 'NONE', #45368 ) ;
#28112 = CARTESIAN_POINT ( 'NONE',  ( 10.00000000000000000, -36.13751322684404244, -21.40280677340410165 ) ) ;
#28113 = CARTESIAN_POINT ( 'NONE',  ( 10.00000000000000000, -77.49459641780886443, 0.8261519478428377417 ) ) ;
#28114 = AXIS2_PLACEMENT_3D ( 'NONE', #24389, #39328, #5810 ) ;
#28115 = DIRECTION ( 'NONE',  ( -1.000000000000000000, 0.000000000000000000, 0.000000000000000000 ) ) ;
#28116 = CARTESIAN_POINT ( 'NONE',  ( 0.000000000000000000, -59.46389618801999433, 49.70050353004867816 ) ) ;
#28117 =( NAMED_UNIT ( * ) PLANE_ANGLE_UNIT ( ) SI_UNIT ( $, .RADIAN. ) );
#28118 = ORIENTED_EDGE ( 'NONE', *, *, #42623, .T. ) ;
#28119 = ORIENTED_EDGE ( 'NONE', *, *, #7480, .F. ) ;
#28120 = AXIS2_PLACEMENT_3D ( 'NONE', #38761, #4723, #15990 ) ;
#28121 = ORIENTED_EDGE ( 'NONE', *, *, #14609, .T. ) ;
#28122 = ADVANCED_FACE ( 'NONE', ( #11848, #40505 ), #18694, .F. ) ;
#28123 = CARTESIAN_POINT ( 'NONE',  ( 11.99999999999999822, 20.41045688087930898, -72.35160999960793049 ) ) ;
#28124 = CARTESIAN_POINT ( 'NONE',  ( -1.384174031800281979, -120.5779811845464735, 2.500000000000000000 ) ) ;
#28125 = ORIENTED_EDGE ( 'NONE', *, *, #33376, .T. ) ;
#28126 = EDGE_CURVE ( 'NONE', #46006, #6288, #33867, .T. ) ;
#28127 = EDGE_CURVE ( 'NONE', #35715, #25450, #25794, .T. ) ;
#28128 = PLANE ( 'NONE',  #42216 ) ;
#28129 = CARTESIAN_POINT ( 'NONE',  ( 0.000000000000000000, 0.000000000000000000, 0.000000000000000000 ) ) ;
#28130 = ORIENTED_EDGE ( 'NONE', *, *, #39202, .F. ) ;
#28131 = VERTEX_POINT ( 'NONE', #22131 ) ;
#28132 = ORIENTED_EDGE ( 'NONE', *, *, #44320, .F. ) ;
#28133 = EDGE_CURVE ( 'NONE', #23166, #2611, #29960, .T. ) ;
#28134 = AXIS2_PLACEMENT_3D ( 'NONE', #24244, #24017, #38952 ) ;
#28135 = CARTESIAN_POINT ( 'NONE',  ( -3.000000000000000000, 6.762365576493643893, -25.66652317338391853 ) ) ;
#28137 = ORIENTED_EDGE ( 'NONE', *, *, #28584, .F. ) ;
#28136 = AXIS2_PLACEMENT_3D ( 'NONE', #24589, #2781, #43668 ) ;
#28138 = DIRECTION ( 'NONE',  ( 0.000000000000000000, 0.000000000000000000, 1.000000000000000000 ) ) ;
#28139 = EDGE_CURVE ( 'NONE', #11421, #21809, #3533, .T. ) ;
#28140 = ORIENTED_EDGE ( 'NONE', *, *, #7328, .T. ) ;
#28141 = DIRECTION ( 'NONE',  ( 0.000000000000000000, 0.000000000000000000, 1.000000000000000000 ) ) ;
#28142 = CIRCLE ( 'NONE', #46909, 37.49900000000000944 ) ;
#28143 = CARTESIAN_POINT ( 'NONE',  ( 10.00000000000000000, 37.16516213103285082, -4.992566952384588141 ) ) ;
#28144 = LINE ( 'NONE', #1242, #44729 ) ;
#28145 = EDGE_LOOP ( 'NONE', ( #29096, #2139, #10990, #23249 ) ) ;
#28146 = DIRECTION ( 'NONE',  ( -1.000000000000000000, 0.000000000000000000, 0.000000000000000000 ) ) ;
#28147 = VERTEX_POINT ( 'NONE', #38777 ) ;
#28148 = CARTESIAN_POINT ( 'NONE',  ( 0.000000000000000000, 0.000000000000000000, 0.000000000000000000 ) ) ;
#28149 = EDGE_CURVE ( 'NONE', #35932, #36740, #1625, .T. ) ;
#28150 = CARTESIAN_POINT ( 'NONE',  ( 4.999999999999999112, -2.663952781845850826, -41.91543099594819921 ) ) ;
#28151 = LINE ( 'NONE', #43085, #41295 ) ;
#28152 = ORIENTED_EDGE ( 'NONE', *, *, #20324, .T. ) ;
#28153 = AXIS2_PLACEMENT_3D ( 'NONE', #35790, #39951, #20613 ) ;
#28154 = ORIENTED_EDGE ( 'NONE', *, *, #42836, .T. ) ;
#28155 = DIRECTION ( 'NONE',  ( 1.000000000000000000, -0.000000000000000000, -0.000000000000000000 ) ) ;
#28156 = FACE_OUTER_BOUND ( 'NONE', #37900, .T. ) ;
#28157 = ORIENTED_EDGE ( 'NONE', *, *, #48050, .F. ) ;
#28158 = DIRECTION ( 'NONE',  ( 0.7950889364178788110, -0.6064928550163524168, 0.000000000000000000 ) ) ;
#28159 = DIRECTION ( 'NONE',  ( 0.000000000000000000, 0.000000000000000000, -1.000000000000000000 ) ) ;
#28160 = DIRECTION ( 'NONE',  ( 0.000000000000000000, -0.7431448254773862505, -0.6691306063588671194 ) ) ;
#28161 = FACE_OUTER_BOUND ( 'NONE', #32225, .T. ) ;
#28162 = DIRECTION ( 'NONE',  ( -1.000000000000000000, 0.000000000000000000, 0.000000000000000000 ) ) ;
#28163 = ADVANCED_FACE ( 'NONE', ( #34840 ), #23106, .T. ) ;
#28164 = DIRECTION ( 'NONE',  ( -1.000000000000000000, -0.000000000000000000, -0.000000000000000000 ) ) ;
#28165 = CARTESIAN_POINT ( 'NONE',  ( 10.00000000000000000, 37.58145647212453611, 0.6853352020791767529 ) ) ;
#28166 = CARTESIAN_POINT ( 'NONE',  ( 0.000000000000000000, 14.66109333815460225, 73.73191006444577056 ) ) ;
#28167 = DIRECTION ( 'NONE',  ( -1.000000000000000000, 0.000000000000000000, 0.000000000000000000 ) ) ;
#28168 = LINE ( 'NONE', #39441, #24892 ) ;
#28169 = CARTESIAN_POINT ( 'NONE',  ( -10.00000000000000000, 0.000000000000000000, 0.000000000000000000 ) ) ;
#28170 = DIRECTION ( 'NONE',  ( 1.000000000000000000, 0.000000000000000000, 0.000000000000000000 ) ) ;
#28171 = VERTEX_POINT ( 'NONE', #26772 ) ;
#28172 = ORIENTED_EDGE ( 'NONE', *, *, #9884, .T. ) ;
#28173 = CARTESIAN_POINT ( 'NONE',  ( 10.00000000000000000, -64.81221759200306565, -50.23322058963418613 ) ) ;
#28174 = VECTOR ( 'NONE', #12200, 1000.000000000000000 ) ;
#28175 = EDGE_CURVE ( 'NONE', #38262, #43952, #38372, .T. ) ;
#28176 = DIRECTION ( 'NONE',  ( -1.000000000000000000, 0.000000000000000000, -0.000000000000000000 ) ) ;
#28177 = AXIS2_PLACEMENT_3D ( 'NONE', #15288, #7918, #45137 ) ;
#28178 = AXIS2_PLACEMENT_3D ( 'NONE', #34995, #27920, #12490 ) ;
#28179 = ADVANCED_FACE ( 'NONE', ( #8892 ), #5464, .T. ) ;
#28180 = DIRECTION ( 'NONE',  ( 0.000000000000000000, 0.000000000000000000, -1.000000000000000000 ) ) ;
#28181 = ORIENTED_EDGE ( 'NONE', *, *, #38803, .F. ) ;
#28182 = ADVANCED_FACE ( 'NONE', ( #31433 ), #27266, .T. ) ;
#28183 = CIRCLE ( 'NONE', #7064, 82.00000000000000000 ) ;
#28184 = VECTOR ( 'NONE', #25979, 1000.000000000000000 ) ;
#28185 = EDGE_CURVE ( 'NONE', #13632, #9450, #12559, .T. ) ;
#28186 = DIRECTION ( 'NONE',  ( -1.000000000000000000, -0.000000000000000000, -0.000000000000000000 ) ) ;
#28187 = ORIENTED_EDGE ( 'NONE', *, *, #4641, .F. ) ;
#28188 = LINE ( 'NONE', #24045, #13575 ) ;
#28189 = ORIENTED_EDGE ( 'NONE', *, *, #3804, .F. ) ;
#28190 = DIRECTION ( 'NONE',  ( 0.000000000000000000, 0.9876883405951382144, -0.1564344650402276493 ) ) ;
#28191 = FACE_OUTER_BOUND ( 'NONE', #43016, .T. ) ;
#28192 = CARTESIAN_POINT ( 'NONE',  ( 0.000000000000000000, 0.000000000000000000, -54.99999999999998579 ) ) ;
#28193 = VERTEX_POINT ( 'NONE', #39004 ) ;
#28195 = VERTEX_POINT ( 'NONE', #23834 ) ;
#28194 = DIRECTION ( 'NONE',  ( 0.9580045777625458836, 0.2867529058022011412, 0.000000000000000000 ) ) ;
#28196 = VERTEX_POINT ( 'NONE', #34337 ) ;
#28197 = ORIENTED_EDGE ( 'NONE', *, *, #38354, .F. ) ;
#28198 = FACE_OUTER_BOUND ( 'NONE', #21747, .T. ) ;
#28199 = LINE ( 'NONE', #40434, #24582 ) ;
#28200 = DIRECTION ( 'NONE',  ( -1.000000000000000000, 0.000000000000000000, -0.000000000000000000 ) ) ;
#28201 = CIRCLE ( 'NONE', #45386, 77.49899999999999523 ) ;
#28202 = CARTESIAN_POINT ( 'NONE',  ( -10.00000000000000000, 0.000000000000000000, 0.000000000000000000 ) ) ;
#28203 = LINE ( 'NONE', #28916, #43429 ) ;
#28204 = ORIENTED_EDGE ( 'NONE', *, *, #44715, .T. ) ;
#28205 = AXIS2_PLACEMENT_3D ( 'NONE', #47867, #39828, #36615 ) ;
#28206 = LINE ( 'NONE', #9590, #5304 ) ;
#28207 = ORIENTED_EDGE ( 'NONE', *, *, #27976, .F. ) ;
#28208 = ORIENTED_EDGE ( 'NONE', *, *, #45424, .F. ) ;
#28209 = DIRECTION ( 'NONE',  ( 0.000000000000000000, -0.2334453638559126909, 0.9723699203976748917 ) ) ;
#28210 = VECTOR ( 'NONE', #30445, 1000.000000000000000 ) ;
#28211 = ORIENTED_EDGE ( 'NONE', *, *, #2055, .T. ) ;
#28212 = DIRECTION ( 'NONE',  ( 0.000000000000000000, 0.000000000000000000, 1.000000000000000000 ) ) ;
#28213 = CARTESIAN_POINT ( 'NONE',  ( 0.000000000000000000, 3.894527615419050903, -81.90746397400384637 ) ) ;
#28214 = FACE_OUTER_BOUND ( 'NONE', #46067, .T. ) ;
#28215 = VERTEX_POINT ( 'NONE', #5239 ) ;
#28216 = CARTESIAN_POINT ( 'NONE',  ( 0.000000000000000000, 26.08949754953062694, -27.05870788708203989 ) ) ;
#28217 = DIRECTION ( 'NONE',  ( -1.000000000000000000, 0.000000000000000000, 0.000000000000000000 ) ) ;
#28218 = AXIS2_PLACEMENT_3D ( 'NONE', #20082, #27437, #15683 ) ;
#28219 = CARTESIAN_POINT ( 'NONE',  ( 3.429551818649054340, -146.3199197248623875, 2.500000000000000000 ) ) ;
#28220 = AXIS2_PLACEMENT_3D ( 'NONE', #47244, #39903, #28159 ) ;
#28221 = LINE ( 'NONE', #27761, #16616 ) ;
#28222 = PLANE ( 'NONE',  #4409 ) ;
#28223 = AXIS2_PLACEMENT_3D ( 'NONE', #33497, #22254, #24948 ) ;
#28224 = DIRECTION ( 'NONE',  ( 0.000000000000000000, 0.7604059656000277112, 0.6494480483301875440 ) ) ;
#28225 = DIRECTION ( 'NONE',  ( 0.000000000000000000, 0.5877852522924797984, -0.8090169943749426773 ) ) ;
#28227 = LINE ( 'NONE', #1567, #40426 ) ;
#28226 = APPLICATION_CONTEXT ( 'automotive_design' ) ;
#28228 = CARTESIAN_POINT ( 'NONE',  ( 0.000000000000000000, 0.000000000000000000, 0.000000000000000000 ) ) ;
#28229 = CARTESIAN_POINT ( 'NONE',  ( 10.00000000000000000, 33.80338159004283938, 16.23288003029508886 ) ) ;
#28230 = CARTESIAN_POINT ( 'NONE',  ( 10.00000000000000000, 36.13751322684449718, -21.40280677340333071 ) ) ;
#28231 = ORIENTED_EDGE ( 'NONE', *, *, #25893, .F. ) ;
#28232 = ORIENTED_EDGE ( 'NONE', *, *, #26427, .T. ) ;
#28233 = DIRECTION ( 'NONE',  ( 0.000000000000000000, 0.000000000000000000, -1.000000000000000000 ) ) ;
#28234 = VERTEX_POINT ( 'NONE', #19413 ) ;
#28235 = EDGE_CURVE ( 'NONE', #36392, #42650, #21944, .T. ) ;
#28236 = DIRECTION ( 'NONE',  ( -1.000000000000000000, -0.000000000000000000, 0.000000000000000000 ) ) ;
#28237 = EDGE_CURVE ( 'NONE', #4382, #40081, #21174, .T. ) ;
#28238 = CARTESIAN_POINT ( 'NONE',  ( -4.653126046682595884, -146.1313684676804314, 5.500000000000000000 ) ) ;
#28239 = ORIENTED_EDGE ( 'NONE', *, *, #3992, .F. ) ;
#28240 = AXIS2_PLACEMENT_3D ( 'NONE', #3964, #18871, #33804 ) ;
#28241 = VECTOR ( 'NONE', #14553, 1000.000000000000000 ) ;
#28242 = EDGE_CURVE ( 'NONE', #22951, #33006, #836, .T. ) ;
#28243 = VECTOR ( 'NONE', #16893, 1000.000000000000000 ) ;
#28244 = VECTOR ( 'NONE', #21202, 1000.000000000000114 ) ;
#28245 = CARTESIAN_POINT ( 'NONE',  ( 11.99999999999999822, 44.88180994100376608, 63.18004540533043922 ) ) ;
#28247 = EDGE_CURVE ( 'NONE', #46719, #9902, #42685, .T. ) ;
#28246 = EDGE_LOOP ( 'NONE', ( #1154, #6212, #21268, #18601 ) ) ;
#28248 = VERTEX_POINT ( 'NONE', #38518 ) ;
#28249 = CIRCLE ( 'NONE', #46217, 77.49899999999999523 ) ;
#28250 = ORIENTED_EDGE ( 'NONE', *, *, #36569, .F. ) ;
#28251 = ORIENTED_EDGE ( 'NONE', *, *, #16518, .F. ) ;
#28252 = DIRECTION ( 'NONE',  ( -0.6064928550163533050, -0.7950889364178781449, 0.000000000000000000 ) ) ;
#28253 = CARTESIAN_POINT ( 'NONE',  ( 0.000000000000000000, 0.000000000000000000, 0.000000000000000000 ) ) ;
#28254 = DIRECTION ( 'NONE',  ( 0.000000000000000000, -0.1045284632676429099, -0.9945218953682744001 ) ) ;
#28255 = VECTOR ( 'NONE', #45061, 1000.000000000000114 ) ;
#28256 = ORIENTED_EDGE ( 'NONE', *, *, #40977, .T. ) ;
#28257 = CARTESIAN_POINT ( 'NONE',  ( 0.000000000000000000, -25.60904388321925396, 6.976881207771170601 ) ) ;
#28258 = ORIENTED_EDGE ( 'NONE', *, *, #15878, .T. ) ;
#28259 = DIRECTION ( 'NONE',  ( 0.000000000000000000, 0.000000000000000000, 1.000000000000000000 ) ) ;
#28260 = DIRECTION ( 'NONE',  ( 0.000000000000000000, 0.1564344650402311743, -0.9876883405951377704 ) ) ;
#28261 = CARTESIAN_POINT ( 'NONE',  ( 0.000000000000000000, -55.16347631943085617, 60.67117009219118273 ) ) ;
#28262 = EDGE_LOOP ( 'NONE', ( #33735, #23813, #615, #32586 ) ) ;
#28263 = VERTEX_POINT ( 'NONE', #30687 ) ;
#28264 = CARTESIAN_POINT ( 'NONE',  ( 10.00000000000000000, -16.65560815589439159, 38.55633173627004595 ) ) ;
#28265 = VERTEX_POINT ( 'NONE', #45611 ) ;
#28266 = DIRECTION ( 'NONE',  ( 0.000000000000000000, 0.000000000000000000, 1.000000000000000000 ) ) ;
#28267 = FACE_OUTER_BOUND ( 'NONE', #23163, .T. ) ;
#28268 = LINE ( 'NONE', #9420, #24266 ) ;
#28269 = FACE_OUTER_BOUND ( 'NONE', #36395, .T. ) ;
#28270 = CARTESIAN_POINT ( 'NONE',  ( 4.999999999999999112, 16.65560815589411092, 38.55633173627015253 ) ) ;
#28271 = CARTESIAN_POINT ( 'NONE',  ( 11.99999999999999822, 72.35160999960844208, -20.41045688087747223 ) ) ;
#28272 = DIRECTION ( 'NONE',  ( 0.000000000000000000, 0.9876883405951372152, 0.1564344650402346160 ) ) ;
#28273 = VECTOR ( 'NONE', #40563, 1000.000000000000000 ) ;
#28274 = CARTESIAN_POINT ( 'NONE',  ( 24.95699195200416654, -110.9640411295978595, 5.500000000000000000 ) ) ;
#28275 = CARTESIAN_POINT ( 'NONE',  ( 0.000000000000000000, 14.67089635893819377, -73.72996012237423713 ) ) ;
#28276 = EDGE_CURVE ( 'NONE', #26988, #34677, #25046, .T. ) ;
#28277 = ORIENTED_EDGE ( 'NONE', *, *, #13967, .F. ) ;
#28278 = AXIS2_PLACEMENT_3D ( 'NONE', #12324, #1306, #38991 ) ;
#28279 = FILL_AREA_STYLE_COLOUR ( '', #6729 ) ;
#28280 = EDGE_CURVE ( 'NONE', #25663, #31426, #41963, .T. ) ;
#28281 = FACE_BOUND ( 'NONE', #38155, .T. ) ;
#28282 = CARTESIAN_POINT ( 'NONE',  ( 10.00000000000000000, 0.000000000000000000, 0.000000000000000000 ) ) ;
#28283 = EDGE_CURVE ( 'NONE', #40440, #32991, #1796, .T. ) ;
#28284 = AXIS2_PLACEMENT_3D ( 'NONE', #18025, #32963, #47886 ) ;
#28285 = DIRECTION ( 'NONE',  ( 0.000000000000000000, 1.000000000000000000, -1.224646799147353207E-16 ) ) ;
#28286 = ORIENTED_EDGE ( 'NONE', *, *, #46710, .F. ) ;
#28287 = DIRECTION ( 'NONE',  ( -1.000000000000000000, 0.000000000000000000, -0.000000000000000000 ) ) ;
#28288 = DIRECTION ( 'NONE',  ( -1.000000000000000000, 0.000000000000000000, -0.000000000000000000 ) ) ;
#28289 = ORIENTED_EDGE ( 'NONE', *, *, #25172, .T. ) ;
#28290 = DIRECTION ( 'NONE',  ( 0.000000000000000000, 0.000000000000000000, 1.000000000000000000 ) ) ;
#28291 = CIRCLE ( 'NONE', #34534, 16.00000000000000355 ) ;
#28292 = ORIENTED_EDGE ( 'NONE', *, *, #27640, .T. ) ;
#28293 = EDGE_CURVE ( 'NONE', #15099, #41560, #46599, .T. ) ;
#28294 = CARTESIAN_POINT ( 'NONE',  ( 11.99999999999999822, -71.91182617369167929, -28.89263327155821059 ) ) ;
#28295 = EDGE_CURVE ( 'NONE', #38611, #25752, #47717, .T. ) ;
#28296 = EDGE_CURVE ( 'NONE', #28502, #17893, #5535, .T. ) ;
#28297 = VERTEX_POINT ( 'NONE', #21604 ) ;
#28298 = VERTEX_POINT ( 'NONE', #10099 ) ;
#28299 = ORIENTED_EDGE ( 'NONE', *, *, #30077, .T. ) ;
#28300 = ORIENTED_EDGE ( 'NONE', *, *, #45691, .T. ) ;
#28301 = EDGE_CURVE ( 'NONE', #31941, #15671, #28201, .T. ) ;
#28302 = CARTESIAN_POINT ( 'NONE',  ( 10.00000000000000000, 6.555932627142952995, -37.01155633439051940 ) ) ;
#28303 = ORIENTED_EDGE ( 'NONE', *, *, #23480, .T. ) ;
#28304 = PRODUCT_DEFINITION ( 'UNKNOWN', '', #45220, #18826 ) ;
#28305 = VERTEX_POINT ( 'NONE', #6198 ) ;
#28306 = VECTOR ( 'NONE', #37799, 999.9999999999998863 ) ;
#28307 = DIRECTION ( 'NONE',  ( 0.000000000000000000, 0.000000000000000000, 1.000000000000000000 ) ) ;
#28308 = CIRCLE ( 'NONE', #34547, 16.00000000000000000 ) ;
#28310 = ORIENTED_EDGE ( 'NONE', *, *, #16406, .T. ) ;
#28309 = CARTESIAN_POINT ( 'NONE',  ( -10.00000000000000000, 0.000000000000000000, 0.000000000000000000 ) ) ;
#28311 = EDGE_LOOP ( 'NONE', ( #5784, #5091, #47627, #36628 ) ) ;
#28312 = VERTEX_POINT ( 'NONE', #32386 ) ;
#28313 = EDGE_LOOP ( 'NONE', ( #32693, #27475, #30180, #42268 ) ) ;
#28314 = VECTOR ( 'NONE', #15042, 1000.000000000000000 ) ;
#28315 = DIRECTION ( 'NONE',  ( 0.000000000000000000, -0.7071067811865536790, 0.7071067811865413555 ) ) ;
#28317 = VERTEX_POINT ( 'NONE', #47316 ) ;
#28316 = DIRECTION ( 'NONE',  ( 0.000000000000000000, 0.000000000000000000, 1.000000000000000000 ) ) ;
#28318 = DIRECTION ( 'NONE',  ( 0.000000000000000000, 0.000000000000000000, -1.000000000000000000 ) ) ;
#28319 = VERTEX_POINT ( 'NONE', #13787 ) ;
#28320 = DIRECTION ( 'NONE',  ( 0.000000000000000000, 0.000000000000000000, -1.000000000000000000 ) ) ;
#28321 = FACE_OUTER_BOUND ( 'NONE', #23031, .T. ) ;
#28322 = DIRECTION ( 'NONE',  ( -1.000000000000000000, 0.000000000000000000, -0.000000000000000000 ) ) ;
#28323 = AXIS2_PLACEMENT_3D ( 'NONE', #36363, #2829, #46675 ) ;
#28324 = CARTESIAN_POINT ( 'NONE',  ( 0.000000000000000000, -62.50329211542465657, 41.76937507738766442 ) ) ;
#28325 = DIRECTION ( 'NONE',  ( -1.000000000000000000, -0.000000000000000000, -0.000000000000000000 ) ) ;
#28326 = CARTESIAN_POINT ( 'NONE',  ( 11.99999999999999822, 0.000000000000000000, 0.000000000000000000 ) ) ;
#28327 = EDGE_CURVE ( 'NONE', #34848, #22027, #2052, .T. ) ;
#28328 = CYLINDRICAL_SURFACE ( 'NONE', #38394, 16.00000000000000355 ) ;
#28329 = DIRECTION ( 'NONE',  ( -1.000000000000000000, -0.000000000000000000, 0.000000000000000000 ) ) ;
#28330 = ADVANCED_FACE ( 'NONE', ( #43157 ), #20884, .F. ) ;
#28331 = VERTEX_POINT ( 'NONE', #25020 ) ;
#28332 = LINE ( 'NONE', #13174, #17347 ) ;
#28333 = ORIENTED_EDGE ( 'NONE', *, *, #35915, .F. ) ;
#28334 = ADVANCED_FACE ( 'NONE', ( #39974 ), #28712, .F. ) ;
#28335 = DIRECTION ( 'NONE',  ( 0.000000000000000000, -0.1045284632676578285, 0.9945218953682729568 ) ) ;
#28336 = CARTESIAN_POINT ( 'NONE',  ( 6.000000000000000000, 2.543863470249533965, -81.96053171279901051 ) ) ;
#28337 = PLANE ( 'NONE',  #24587 ) ;
#28338 = DIRECTION ( 'NONE',  ( -1.000000000000000000, 0.000000000000000000, 0.000000000000000000 ) ) ;
#28339 = EDGE_CURVE ( 'NONE', #32136, #11391, #43635, .T. ) ;
#28340 = FACE_OUTER_BOUND ( 'NONE', #22454, .T. ) ;
#28342 = VECTOR ( 'NONE', #34590, 1000.000000000000000 ) ;
#28341 = DIRECTION ( 'NONE',  ( -1.000000000000000000, -0.000000000000000000, -0.000000000000000000 ) ) ;
#28343 = EDGE_LOOP ( 'NONE', ( #9688, #6122, #24341, #23978 ) ) ;
#28344 = DIRECTION ( 'NONE',  ( 1.000000000000000000, -0.000000000000000000, -0.000000000000000000 ) ) ;
#28345 = DIRECTION ( 'NONE',  ( 0.000000000000000000, 0.5224985647159441360, 0.8526401643540952868 ) ) ;
#28346 = DIRECTION ( 'NONE',  ( 0.000000000000000000, 0.3090169943749482839, -0.9510565162951533091 ) ) ;
#28347 = ORIENTED_EDGE ( 'NONE', *, *, #12425, .T. ) ;
#28348 = AXIS2_PLACEMENT_3D ( 'NONE', #31542, #23443, #46462 ) ;
#28349 = VECTOR ( 'NONE', #20984, 1000.000000000000000 ) ;
#28350 = CARTESIAN_POINT ( 'NONE',  ( -8.637688417678527131, 13.69818742750669394, 32.98187577049606745 ) ) ;
#28351 = SURFACE_STYLE_USAGE ( .BOTH. , #47200 ) ;
#28352 = CIRCLE ( 'NONE', #43964, 16.00000000000000000 ) ;
#28353 = EDGE_CURVE ( 'NONE', #34027, #1594, #36823, .T. ) ;
#28354 = EDGE_CURVE ( 'NONE', #43524, #33083, #36286, .T. ) ;
#28355 = ORIENTED_EDGE ( 'NONE', *, *, #41444, .F. ) ;
#28356 = EDGE_LOOP ( 'NONE', ( #11351, #12449, #36069, #39028 ) ) ;
#28357 = CIRCLE ( 'NONE', #18171, 42.00000000000000000 ) ;
#28358 = VERTEX_POINT ( 'NONE', #28219 ) ;
#28359 = VECTOR ( 'NONE', #43892, 1000.000000000000000 ) ;
#28360 = CARTESIAN_POINT ( 'NONE',  ( 0.000000000000000000, -62.20884554313985149, -46.21855187248698371 ) ) ;
#28361 = CARTESIAN_POINT ( 'NONE',  ( -12.50000000000000000, -107.5000000000000000, -40.00000000000000000 ) ) ;
#28362 = EDGE_LOOP ( 'NONE', ( #32528, #23435, #20168, #10442 ) ) ;
#28363 = EDGE_CURVE ( 'NONE', #27745, #42340, #13392, .T. ) ;
#28364 = ORIENTED_EDGE ( 'NONE', *, *, #28636, .T. ) ;
#28365 = DIRECTION ( 'NONE',  ( 0.000000000000000000, 0.000000000000000000, 1.000000000000000000 ) ) ;
#28366 = ORIENTED_EDGE ( 'NONE', *, *, #35912, .F. ) ;
#28367 = ORIENTED_EDGE ( 'NONE', *, *, #16583, .F. ) ;
#28368 = ORIENTED_EDGE ( 'NONE', *, *, #2628, .T. ) ;
#28369 = AXIS2_PLACEMENT_3D ( 'NONE', #46543, #42380, #8589 ) ;
#28370 = AXIS2_PLACEMENT_3D ( 'NONE', #1491, #15689, #23280 ) ;
#28371 = LINE ( 'NONE', #47220, #43825 ) ;
#28372 = ORIENTED_EDGE ( 'NONE', *, *, #32925, .F. ) ;
#28373 = DIRECTION ( 'NONE',  ( -0.000000000000000000, 0.4999999999999919509, 0.8660254037844432595 ) ) ;
#28374 = VERTEX_POINT ( 'NONE', #28929 ) ;
#28375 = CARTESIAN_POINT ( 'NONE',  ( 0.000000000000000000, 77.32052557432849937, -5.256550761632002633 ) ) ;
#28376 = AXIS2_PLACEMENT_3D ( 'NONE', #41053, #37845, #29537 ) ;
#28377 = CIRCLE ( 'NONE', #31552, 16.00000000000000000 ) ;
#28378 = AXIS2_PLACEMENT_3D ( 'NONE', #4326, #637, #26349 ) ;
#28379 = DIRECTION ( 'NONE',  ( -1.000000000000000000, 0.000000000000000000, -0.000000000000000000 ) ) ;
#28380 = CARTESIAN_POINT ( 'NONE',  ( 10.00000000000000000, 0.000000000000000000, 0.000000000000000000 ) ) ;
#28381 = ORIENTED_EDGE ( 'NONE', *, *, #22695, .T. ) ;
#28382 = FACE_OUTER_BOUND ( 'NONE', #37343, .T. ) ;
#28383 = VERTEX_POINT ( 'NONE', #17912 ) ;
#28384 = CARTESIAN_POINT ( 'NONE',  ( 11.99999999999999822, 0.000000000000000000, 0.000000000000000000 ) ) ;
#28385 = CYLINDRICAL_SURFACE ( 'NONE', #20410, 31.99999999999998579 ) ;
#28386 = AXIS2_PLACEMENT_3D ( 'NONE', #23831, #45364, #46104 ) ;
#28387 = ORIENTED_EDGE ( 'NONE', *, *, #20264, .F. ) ;
#28388 = EDGE_LOOP ( 'NONE', ( #47526, #7903, #47217, #46820 ) ) ;
#28389 = DIRECTION ( 'NONE',  ( 0.000000000000000000, 0.000000000000000000, 1.000000000000000000 ) ) ;
#28390 = DIRECTION ( 'NONE',  ( -1.000000000000000000, 0.000000000000000000, 0.000000000000000000 ) ) ;
#28391 = ORIENTED_EDGE ( 'NONE', *, *, #782, .T. ) ;
#28392 = VECTOR ( 'NONE', #26266, 1000.000000000000000 ) ;
#28393 = EDGE_CURVE ( 'NONE', #46139, #40664, #8696, .T. ) ;
#28394 = CARTESIAN_POINT ( 'NONE',  ( 10.00000000000000000, 0.000000000000000000, 0.000000000000000000 ) ) ;
#28395 = DIRECTION ( 'NONE',  ( -1.000000000000000000, 0.000000000000000000, 0.000000000000000000 ) ) ;
#28396 = DIRECTION ( 'NONE',  ( -1.000000000000000000, 0.000000000000000000, 0.000000000000000000 ) ) ;
#28397 = CARTESIAN_POINT ( 'NONE',  ( 15.00000000000000000, 9.615535125378766423, -24.73947219025917121 ) ) ;
#28398 = EDGE_CURVE ( 'NONE', #45904, #15507, #32613, .T. ) ;
#28399 = CIRCLE ( 'NONE', #19787, 37.49900000000000233 ) ;
#28400 = CARTESIAN_POINT ( 'NONE',  ( 119.3426274441929280, -132.5434155921172419, -5.500000000000000000 ) ) ;
#28401 = CARTESIAN_POINT ( 'NONE',  ( 4.999999999999999112, 9.188173127307898369, -40.98264845739739570 ) ) ;
#28402 = CARTESIAN_POINT ( 'NONE',  ( 0.000000000000000000, -26.02418014898359289, 70.52718814184250107 ) ) ;
#28403 = CARTESIAN_POINT ( 'NONE',  ( 12.00000000000000000, -23.29833615347104470, 3.418703333116808629 ) ) ;
#28404 = CYLINDRICAL_SURFACE ( 'NONE', #7399, 82.00000000000000000 ) ;
#28406 = VECTOR ( 'NONE', #13741, 1000.000000000000000 ) ;
#28405 = CARTESIAN_POINT ( 'NONE',  ( 10.00000000000000000, 73.44644590900094272, -24.73286445877628026 ) ) ;
#28407 = DIRECTION ( 'NONE',  ( 0.000000000000000000, 0.2079116908177532363, -0.9781476007338069101 ) ) ;
#28408 = CARTESIAN_POINT ( 'NONE',  ( 10.00000000000000000, 0.000000000000000000, 0.000000000000000000 ) ) ;
#28409 = VERTEX_POINT ( 'NONE', #43870 ) ;
#28410 = EDGE_CURVE ( 'NONE', #35941, #5623, #38410, .T. ) ;
#28411 = EDGE_CURVE ( 'NONE', #34606, #36756, #3202, .T. ) ;
#28412 = CIRCLE ( 'NONE', #7295, 37.49900000000000233 ) ;
#28413 = ORIENTED_EDGE ( 'NONE', *, *, #5698, .F. ) ;
#28414 = ORIENTED_EDGE ( 'NONE', *, *, #26841, .T. ) ;
#28415 = DIRECTION ( 'NONE',  ( -1.000000000000000000, -0.000000000000000000, -0.000000000000000000 ) ) ;
#28416 = ADVANCED_FACE ( 'NONE', ( #39495 ), #2504, .T. ) ;
#28417 = CYLINDRICAL_SURFACE ( 'NONE', #33844, 31.99999999999999289 ) ;
#28418 = CIRCLE ( 'NONE', #15907, 42.00000000000000000 ) ;
#28419 = AXIS2_PLACEMENT_3D ( 'NONE', #891, #45447, #4581 ) ;
#28420 = CONTEXT_DEPENDENT_SHAPE_REPRESENTATION ( #20721, #26555 ) ;
#28421 = AXIS2_PLACEMENT_3D ( 'NONE', #44276, #10506, #48418 ) ;
#28422 = LINE ( 'NONE', #35279, #4189 ) ;
#28423 = VERTEX_POINT ( 'NONE', #2271 ) ;
#28424 = EDGE_CURVE ( 'NONE', #43507, #19471, #17188, .T. ) ;
#28425 = TOROIDAL_SURFACE ( 'NONE', #19807, 12.80000000000000071, 0.2999999999999999334 ) ;
#28426 = CIRCLE ( 'NONE', #24513, 42.00000000000000000 ) ;
#28427 = CIRCLE ( 'NONE', #14345, 31.99999999999998224 ) ;
#28428 = DIRECTION ( 'NONE',  ( -1.000000000000000000, 0.000000000000000000, 0.000000000000000000 ) ) ;
#28429 = DIRECTION ( 'NONE',  ( 0.000000000000000000, 0.000000000000000000, 1.000000000000000000 ) ) ;
#28430 = ORIENTED_EDGE ( 'NONE', *, *, #36902, .T. ) ;
#28431 = DIRECTION ( 'NONE',  ( -1.000000000000000000, 0.000000000000000000, -0.000000000000000000 ) ) ;
#28432 = AXIS2_PLACEMENT_3D ( 'NONE', #27725, #42157, #9111 ) ;
#28433 = DIRECTION ( 'NONE',  ( -1.000000000000000000, -0.000000000000000000, -0.000000000000000000 ) ) ;
#28434 = DIRECTION ( 'NONE',  ( -1.000000000000000000, -0.000000000000000000, -0.000000000000000000 ) ) ;
#28435 = ORIENTED_EDGE ( 'NONE', *, *, #9385, .F. ) ;
#28436 = CARTESIAN_POINT ( 'NONE',  ( -18.12185313557659683, -104.9634299478706794, -2.500000000000000000 ) ) ;
#28437 = ORIENTED_EDGE ( 'NONE', *, *, #6794, .F. ) ;
#28438 = ORIENTED_EDGE ( 'NONE', *, *, #5528, .F. ) ;
#28439 = DIRECTION ( 'NONE',  ( -1.000000000000000000, -0.000000000000000000, -0.000000000000000000 ) ) ;
#28440 = VERTEX_POINT ( 'NONE', #24795 ) ;
#28441 = CARTESIAN_POINT ( 'NONE',  ( 11.99999999999999822, -41.76937507738745836, -62.50329211542482710 ) ) ;
#28442 = DIRECTION ( 'NONE',  ( -1.000000000000000000, -0.000000000000000000, 0.000000000000000000 ) ) ;
#28443 = VECTOR ( 'NONE', #32736, 1000.000000000000000 ) ;
#28444 = CARTESIAN_POINT ( 'NONE',  ( 10.00000000000000000, 77.32052557432849937, -5.256550761632002633 ) ) ;
#28445 = AXIS2_PLACEMENT_3D ( 'NONE', #46099, #42421, #8885 ) ;
#28446 = CARTESIAN_POINT ( 'NONE',  ( 0.000000000000000000, 35.91791733033570466, -68.67312586194960033 ) ) ;
#28447 = VERTEX_POINT ( 'NONE', #13065 ) ;
#28448 = CARTESIAN_POINT ( 'NONE',  ( 10.00000000000000000, -65.58780272294100655, 36.73666225445870737 ) ) ;
#28449 = ORIENTED_EDGE ( 'NONE', *, *, #33105, .F. ) ;
#28450 = ORIENTED_EDGE ( 'NONE', *, *, #14878, .T. ) ;
#28451 = ADVANCED_FACE ( 'NONE', ( #27997 ), #39737, .T. ) ;
#28452 = CIRCLE ( 'NONE', #15955, 11.59999999999999964 ) ;
#28453 = CARTESIAN_POINT ( 'NONE',  ( 12.00000000000000000, 26.49999999999999645, 1.499999999999995781 ) ) ;
#28454 = CIRCLE ( 'NONE', #1085, 31.99999999999999289 ) ;
#28455 = ADVANCED_FACE ( 'NONE', ( #25737 ), #11065, .F. ) ;
#28456 = DIRECTION ( 'NONE',  ( 0.000000000000000000, 0.000000000000000000, 1.000000000000000000 ) ) ;
#28457 = CARTESIAN_POINT ( 'NONE',  ( -42.50000000000000000, 0.000000000000000000, -12.50000000000000000 ) ) ;
#28458 = LINE ( 'NONE', #5962, #29780 ) ;
#28459 = ORIENTED_EDGE ( 'NONE', *, *, #28354, .T. ) ;
#28460 = CARTESIAN_POINT ( 'NONE',  ( 11.99999999999999822, 75.11725578898467859, 2.956366410620910656 ) ) ;
#28461 = PRODUCT_DEFINITION_SHAPE ( 'NONE', 'NONE',  #24442 ) ;
#28462 = DIRECTION ( 'NONE',  ( -1.000000000000000000, 0.000000000000000000, -0.000000000000000000 ) ) ;
#28463 = EDGE_CURVE ( 'NONE', #12730, #2585, #10594, .T. ) ;
#28464 = DIRECTION ( 'NONE',  ( 1.000000000000000000, 0.000000000000000000, 0.000000000000000000 ) ) ;
#28465 = CARTESIAN_POINT ( 'NONE',  ( 10.00000000000000000, -80.55351364060599906, 15.33399622253456940 ) ) ;
#28466 = EDGE_CURVE ( 'NONE', #37765, #28782, #23547, .T. ) ;
#28467 = DIRECTION ( 'NONE',  ( -1.000000000000000000, 0.000000000000000000, 0.000000000000000000 ) ) ;
#28468 = ORIENTED_EDGE ( 'NONE', *, *, #21683, .F. ) ;
#28469 = AXIS2_PLACEMENT_3D ( 'NONE', #35702, #46730, #2172 ) ;
#28470 = CIRCLE ( 'NONE', #17518, 42.00000000000000000 ) ;
#28471 = EDGE_CURVE ( 'NONE', #25264, #31943, #18824, .T. ) ;
#28472 = DIRECTION ( 'NONE',  ( -1.000000000000000000, 0.000000000000000000, 0.000000000000000000 ) ) ;
#28474 = EDGE_CURVE ( 'NONE', #48127, #13412, #25505, .T. ) ;
#28473 = LINE ( 'NONE', #14258, #40297 ) ;
#28475 = DIRECTION ( 'NONE',  ( 0.000000000000000000, 0.3826834323650841752, 0.9238795325112891810 ) ) ;
#28477 = CIRCLE ( 'NONE', #4265, 42.00000000000000000 ) ;
#28476 = DIRECTION ( 'NONE',  ( -1.000000000000000000, 0.000000000000000000, 0.000000000000000000 ) ) ;
#28478 = AXIS2_PLACEMENT_3D ( 'NONE', #20528, #8785, #20785 ) ;
#28479 = CARTESIAN_POINT ( 'NONE',  ( 0.000000000000000000, 0.000000000000000000, 0.000000000000000000 ) ) ;
#28480 = FACE_OUTER_BOUND ( 'NONE', #24387, .T. ) ;
#28481 = CIRCLE ( 'NONE', #9742, 82.00000000000000000 ) ;
#28482 = EDGE_LOOP ( 'NONE', ( #7834, #21700, #6567, #16435 ) ) ;
#28483 = DIRECTION ( 'NONE',  ( 1.000000000000000000, -0.000000000000000000, -0.000000000000000000 ) ) ;
#28484 = ORIENTED_EDGE ( 'NONE', *, *, #43811, .T. ) ;
#28485 = CARTESIAN_POINT ( 'NONE',  ( 0.000000000000000000, 0.000000000000000000, 0.000000000000000000 ) ) ;
#28486 = DIRECTION ( 'NONE',  ( -1.000000000000000000, -0.000000000000000000, -0.000000000000000000 ) ) ;
#28487 = VERTEX_POINT ( 'NONE', #11558 ) ;
#28488 = ORIENTED_EDGE ( 'NONE', *, *, #43550, .T. ) ;
#28489 = ADVANCED_FACE ( 'NONE', ( #7635 ), #33341, .T. ) ;
#28490 = AXIS2_PLACEMENT_3D ( 'NONE', #18638, #11784, #33568 ) ;
#28491 = CIRCLE ( 'NONE', #44179, 16.00000000000000000 ) ;
#28492 = AXIS2_PLACEMENT_3D ( 'NONE', #5251, #9876, #23845 ) ;
#28493 = DIRECTION ( 'NONE',  ( -1.000000000000000000, -0.000000000000000000, 0.000000000000000000 ) ) ;
#28494 = ORIENTED_EDGE ( 'NONE', *, *, #46359, .T. ) ;
#28495 = AXIS2_PLACEMENT_3D ( 'NONE', #12322, #27734, #42666 ) ;
#28496 = VERTEX_POINT ( 'NONE', #22333 ) ;
#28497 = ADVANCED_FACE ( 'NONE', ( #3220 ), #26482, .T. ) ;
#28498 = ORIENTED_EDGE ( 'NONE', *, *, #19727, .T. ) ;
#28499 = AXIS2_PLACEMENT_3D ( 'NONE', #40772, #7491, #40534 ) ;
#28500 = VECTOR ( 'NONE', #19848, 1000.000000000000114 ) ;
#28501 = DIRECTION ( 'NONE',  ( -1.000000000000000000, 0.000000000000000000, 0.000000000000000000 ) ) ;
#28502 = VERTEX_POINT ( 'NONE', #4211 ) ;
#28503 = AXIS2_PLACEMENT_3D ( 'NONE', #36641, #6799, #29313 ) ;
#28504 = CARTESIAN_POINT ( 'NONE',  ( 0.000000000000000000, 0.000000000000000000, 0.000000000000000000 ) ) ;
#28505 = VECTOR ( 'NONE', #1026, 1000.000000000000000 ) ;
#28506 = CARTESIAN_POINT ( 'NONE',  ( 0.000000000000000000, -33.79645857604525361, 16.45098606841114730 ) ) ;
#28507 = EDGE_LOOP ( 'NONE', ( #44194, #8445, #8269, #29123 ) ) ;
#28508 = CARTESIAN_POINT ( 'NONE',  ( 0.000000000000000000, 81.34940948281351325, -10.30890764327295450 ) ) ;
#28509 = EDGE_LOOP ( 'NONE', ( #18177, #45969, #12171, #1209 ) ) ;
#28510 = VERTEX_POINT ( 'NONE', #37730 ) ;
#28511 = AXIS2_PLACEMENT_3D ( 'NONE', #29773, #44707, #19245 ) ;
#28512 = DIRECTION ( 'NONE',  ( -1.000000000000000000, -0.000000000000000000, 0.000000000000000000 ) ) ;
#28513 = DIRECTION ( 'NONE',  ( 0.000000000000000000, -0.000000000000000000, 1.000000000000000000 ) ) ;
#28514 = CARTESIAN_POINT ( 'NONE',  ( 10.00000000000000000, -12.26510123303284594, 35.53030884539080603 ) ) ;
#28515 = ADVANCED_FACE ( 'NONE', ( #25983 ), #22067, .F. ) ;
#28516 = ORIENTED_EDGE ( 'NONE', *, *, #3265, .F. ) ;
#28517 = PLANE ( 'NONE',  #14638 ) ;
#28518 = ORIENTED_EDGE ( 'NONE', *, *, #17472, .T. ) ;
#28519 = EDGE_CURVE ( 'NONE', #4582, #17307, #11047, .T. ) ;
#28520 = LINE ( 'NONE', #17483, #15272 ) ;
#28521 = CARTESIAN_POINT ( 'NONE',  ( 10.00000000000000000, 41.91543099594818500, -2.663952781846293139 ) ) ;
#28522 = DIRECTION ( 'NONE',  ( -1.000000000000000000, 0.000000000000000000, -0.000000000000000000 ) ) ;
#28523 = DIRECTION ( 'NONE',  ( 0.000000000000000000, 0.000000000000000000, -1.000000000000000000 ) ) ;
#28524 = EDGE_CURVE ( 'NONE', #8199, #46824, #44355, .T. ) ;
#28525 = DIRECTION ( 'NONE',  ( 0.000000000000000000, -0.9876883405951359940, -0.1564344650402420267 ) ) ;
#28526 = CARTESIAN_POINT ( 'NONE',  ( 10.00000000000000000, 0.000000000000000000, 0.000000000000000000 ) ) ;
#28527 = CARTESIAN_POINT ( 'NONE',  ( 0.000000000000000000, -37.48860685352290290, -0.8828120875904512665 ) ) ;
#28528 = CARTESIAN_POINT ( 'NONE',  ( 2.500000000000000000, 16.00000000000000000, -10.00000000000000178 ) ) ;
#28529 = CARTESIAN_POINT ( 'NONE',  ( -35.50000000000000711, -120.0000000000000000, 5.500000000000000000 ) ) ;
#28530 = CARTESIAN_POINT ( 'NONE',  ( 11.99999999999999822, -44.88180994100419952, 63.18004540533013369 ) ) ;
#28531 = ORIENTED_EDGE ( 'NONE', *, *, #21101, .F. ) ;
#28532 = ORIENTED_EDGE ( 'NONE', *, *, #11115, .F. ) ;
#28534 = EDGE_CURVE ( 'NONE', #44380, #30662, #45084, .T. ) ;
#28533 = DIRECTION ( 'NONE',  ( 0.000000000000000000, 0.000000000000000000, -1.000000000000000000 ) ) ;
#28535 = AXIS2_PLACEMENT_3D ( 'NONE', #4270, #41956, #38510 ) ;
#28536 = CARTESIAN_POINT ( 'NONE',  ( 10.00000000000000000, 0.000000000000000000, 0.000000000000000000 ) ) ;
#28537 = DIRECTION ( 'NONE',  ( 1.000000000000000000, 0.000000000000000000, 0.000000000000000000 ) ) ;
#28538 = CARTESIAN_POINT ( 'NONE',  ( 11.99999999999999822, -59.03961581697367933, -46.53671651294010303 ) ) ;
#28539 = AXIS2_PLACEMENT_3D ( 'NONE', #20669, #6230, #35348 ) ;
#28540 = CIRCLE ( 'NONE', #8196, 31.99999999999998934 ) ;
#28541 = FACE_OUTER_BOUND ( 'NONE', #47388, .T. ) ;
#28542 = DIRECTION ( 'NONE',  ( -0.000000000000000000, -0.000000000000000000, -1.000000000000000000 ) ) ;
#28543 = ORIENTED_EDGE ( 'NONE', *, *, #39208, .T. ) ;
#28544 = CARTESIAN_POINT ( 'NONE',  ( 10.00000000000000000, 0.000000000000000000, 0.000000000000000000 ) ) ;
#28545 = AXIS2_PLACEMENT_3D ( 'NONE', #20209, #27563, #42491 ) ;
#28546 = ORIENTED_EDGE ( 'NONE', *, *, #36974, .T. ) ;
#28547 = DIRECTION ( 'NONE',  ( 0.000000000000000000, 0.000000000000000000, 1.000000000000000000 ) ) ;
#28548 = VECTOR ( 'NONE', #48131, 1000.000000000000000 ) ;
#28549 = ORIENTED_EDGE ( 'NONE', *, *, #6913, .T. ) ;
#28550 = ORIENTED_EDGE ( 'NONE', *, *, #28755, .T. ) ;
#28551 = ORIENTED_EDGE ( 'NONE', *, *, #22490, .F. ) ;
#28552 = VERTEX_POINT ( 'NONE', #36996 ) ;
#28553 = AXIS2_PLACEMENT_3D ( 'NONE', #4155, #7330, #18816 ) ;
#28554 = DIRECTION ( 'NONE',  ( -1.000000000000000000, 0.000000000000000000, -0.000000000000000000 ) ) ;
#28555 = ORIENTED_EDGE ( 'NONE', *, *, #43492, .F. ) ;
#28556 = ORIENTED_EDGE ( 'NONE', *, *, #7394, .T. ) ;
#28557 = CIRCLE ( 'NONE', #2018, 77.49900000000000944 ) ;
#28558 = ADVANCED_FACE ( 'NONE', ( #14506 ), #29432, .F. ) ;
#28559 = FACE_OUTER_BOUND ( 'NONE', #26950, .T. ) ;
#28560 = AXIS2_PLACEMENT_3D ( 'NONE', #40447, #21598, #6903 ) ;
#28561 = LINE ( 'NONE', #24160, #34736 ) ;
#28562 = EDGE_CURVE ( 'NONE', #41259, #23903, #47764, .T. ) ;
#28563 = VERTEX_POINT ( 'NONE', #18410 ) ;
#28564 = ORIENTED_EDGE ( 'NONE', *, *, #45513, .F. ) ;
#28565 = VERTEX_POINT ( 'NONE', #44590 ) ;
#28566 = CARTESIAN_POINT ( 'NONE',  ( 0.000000000000000000, 0.000000000000000000, 0.000000000000000000 ) ) ;
#28567 = DIRECTION ( 'NONE',  ( -1.000000000000000000, 0.000000000000000000, 0.000000000000000000 ) ) ;
#28568 = DIRECTION ( 'NONE',  ( 0.000000000000000000, -0.9510565162951543083, -0.3090169943749448977 ) ) ;
#28569 = AXIS2_PLACEMENT_3D ( 'NONE', #45340, #41441, #11821 ) ;
#28570 = AXIS2_PLACEMENT_3D ( 'NONE', #43852, #13997, #25234 ) ;
#28571 = ORIENTED_EDGE ( 'NONE', *, *, #28295, .T. ) ;
#28572 = ORIENTED_EDGE ( 'NONE', *, *, #37247, .F. ) ;
#28573 = DIRECTION ( 'NONE',  ( 0.000000000000000000, 0.000000000000000000, 1.000000000000000000 ) ) ;
#28574 = ORIENTED_EDGE ( 'NONE', *, *, #41729, .T. ) ;
#28575 = CYLINDRICAL_SURFACE ( 'NONE', #32784, 31.99999999999998579 ) ;
#28576 = CARTESIAN_POINT ( 'NONE',  ( 0.000000000000000000, -120.0000000000000000, 102.9091629284897493 ) ) ;
#28577 = VECTOR ( 'NONE', #47592, 1000.000000000000000 ) ;
#28578 = CARTESIAN_POINT ( 'NONE',  ( 12.50000000000000000, -107.5000000000000000, -2.500000000000000000 ) ) ;
#28579 = LINE ( 'NONE', #8754, #43274 ) ;
#28580 = EDGE_CURVE ( 'NONE', #28248, #20499, #14986, .T. ) ;
#28581 = FACE_OUTER_BOUND ( 'NONE', #19092, .T. ) ;
#28582 = CIRCLE ( 'NONE', #24668, 31.99999999999999289 ) ;
#28583 = VECTOR ( 'NONE', #42602, 1000.000000000000000 ) ;
#28584 = EDGE_CURVE ( 'NONE', #35947, #5318, #15727, .T. ) ;
#28586 = ADVANCED_FACE ( 'NONE', ( #27209 ), #27448, .T. ) ;
#28585 = DIRECTION ( 'NONE',  ( -1.000000000000000000, 0.000000000000000000, 0.000000000000000000 ) ) ;
#28587 = DIRECTION ( 'NONE',  ( -1.000000000000000000, -0.000000000000000000, 0.000000000000000000 ) ) ;
#28588 = ORIENTED_EDGE ( 'NONE', *, *, #29218, .F. ) ;
#28590 = EDGE_CURVE ( 'NONE', #18006, #6864, #17286, .T. ) ;
#28589 = CARTESIAN_POINT ( 'NONE',  ( 11.99999999999999822, -74.18225833017864090, -34.94270380257717790 ) ) ;
#28591 = EDGE_LOOP ( 'NONE', ( #46623, #47569, #16530, #4449 ) ) ;
#28592 = CARTESIAN_POINT ( 'NONE',  ( 0.000000000000000000, -25.88420570971419821, 27.13269053701087330 ) ) ;
#28593 = CARTESIAN_POINT ( 'NONE',  ( 10.00000000000000000, -77.32052557432837148, -5.256550761633697277 ) ) ;
#28594 = CARTESIAN_POINT ( 'NONE',  ( 1.250000000000000000, -12.36245420541525597, 0.000000000000000000 ) ) ;
#28595 = CIRCLE ( 'NONE', #21560, 16.00000000000000000 ) ;
#28596 = EDGE_CURVE ( 'NONE', #24462, #2149, #27450, .T. ) ;
#28597 = PLANE ( 'NONE',  #1022 ) ;
#28598 = VECTOR ( 'NONE', #41247, 1000.000000000000000 ) ;
#28599 = VERTEX_POINT ( 'NONE', #19362 ) ;
#28600 = DIRECTION ( 'NONE',  ( 0.000000000000000000, -0.5877852522924689183, -0.8090169943749504489 ) ) ;
#28601 = DIRECTION ( 'NONE',  ( 0.000000000000000000, 0.000000000000000000, 1.000000000000000000 ) ) ;
#28602 = CIRCLE ( 'NONE', #45014, 16.00000000000000355 ) ;
#28603 = ORIENTED_EDGE ( 'NONE', *, *, #37957, .T. ) ;
#28604 = CARTESIAN_POINT ( 'NONE',  ( 10.00000000000000000, 21.40280677340372151, 36.13751322684426981 ) ) ;
#28605 = LINE ( 'NONE', #31816, #33938 ) ;
#28606 = DIRECTION ( 'NONE',  ( 0.000000000000000000, -0.1564344650402381687, 0.9876883405951365491 ) ) ;
#28607 = CARTESIAN_POINT ( 'NONE',  ( -7.670864526094547386, -97.73662565058241114, -2.500000000000000000 ) ) ;
#28608 = ORIENTED_EDGE ( 'NONE', *, *, #31766, .F. ) ;
#28609 = VERTEX_POINT ( 'NONE', #4921 ) ;
#28610 = ORIENTED_EDGE ( 'NONE', *, *, #43769, .T. ) ;
#28611 = CIRCLE ( 'NONE', #2810, 16.00000000000000355 ) ;
#28612 = CIRCLE ( 'NONE', #16110, 21.00000000000000000 ) ;
#28613 = LINE ( 'NONE', #28837, #6936 ) ;
#28614 = CARTESIAN_POINT ( 'NONE',  ( 0.000000000000000000, 63.18004540533092239, -44.88180994100307686 ) ) ;
#28615 = VERTEX_POINT ( 'NONE', #12755 ) ;
#28616 = EDGE_CURVE ( 'NONE', #8291, #451, #3996, .T. ) ;
#28617 = DIRECTION ( 'NONE',  ( 0.000000000000000000, 0.000000000000000000, 1.000000000000000000 ) ) ;
#28618 = EDGE_CURVE ( 'NONE', #22486, #27674, #34776, .T. ) ;
#28619 = VERTEX_POINT ( 'NONE', #19837 ) ;
#28620 = VERTEX_POINT ( 'NONE', #38459 ) ;
#28621 = AXIS2_PLACEMENT_3D ( 'NONE', #7641, #4218, #40935 ) ;
#28622 = ORIENTED_EDGE ( 'NONE', *, *, #4645, .F. ) ;
#28623 = CIRCLE ( 'NONE', #30175, 31.99999999999998224 ) ;
#28624 = EDGE_CURVE ( 'NONE', #39725, #4261, #1502, .T. ) ;
#28625 = AXIS2_PLACEMENT_3D ( 'NONE', #3903, #37674, #18815 ) ;
#28626 = DIRECTION ( 'NONE',  ( 0.000000000000000000, 0.000000000000000000, 1.000000000000000000 ) ) ;
#28627 = ORIENTED_EDGE ( 'NONE', *, *, #3798, .T. ) ;
#28628 = CARTESIAN_POINT ( 'NONE',  ( -10.00000000000000000, 0.000000000000000000, 0.000000000000000000 ) ) ;
#28629 = ORIENTED_EDGE ( 'NONE', *, *, #22500, .F. ) ;
#28630 = DIRECTION ( 'NONE',  ( -0.5687579148473752566, 0.8225049752423786442, 0.000000000000000000 ) ) ;
#28631 = DIRECTION ( 'NONE',  ( -1.000000000000000000, -0.000000000000000000, 0.000000000000000000 ) ) ;
#28632 = DIRECTION ( 'NONE',  ( -1.000000000000000000, 0.000000000000000000, -0.000000000000000000 ) ) ;
#28633 = EDGE_LOOP ( 'NONE', ( #20547, #24117, #38265, #11912 ) ) ;
#28634 = ADVANCED_FACE ( 'NONE', ( #8584 ), #9086, .T. ) ;
#28635 = CARTESIAN_POINT ( 'NONE',  ( 10.00000000000000000, -6.736453364083817341, 36.88895765772630142 ) ) ;
#28636 = EDGE_CURVE ( 'NONE', #45971, #47873, #16196, .T. ) ;
#28637 = EDGE_LOOP ( 'NONE', ( #11217, #26508, #39865, #31643 ) ) ;
#28638 = CARTESIAN_POINT ( 'NONE',  ( 11.99999999999999822, -23.16143007188479430, 73.95703589263968070 ) ) ;
#28639 = CARTESIAN_POINT ( 'NONE',  ( 15.00000000000000000, -18.13022148937263012, -15.02647892043543898 ) ) ;
#28640 = VERTEX_POINT ( 'NONE', #37981 ) ;
#28641 = ORIENTED_EDGE ( 'NONE', *, *, #10167, .T. ) ;
#28642 = PLANE ( 'NONE',  #29132 ) ;
#28643 = DIRECTION ( 'NONE',  ( 0.000000000000000000, 0.000000000000000000, 1.000000000000000000 ) ) ;
#28644 = ORIENTED_EDGE ( 'NONE', *, *, #15817, .F. ) ;
#28645 = VERTEX_POINT ( 'NONE', #12042 ) ;
#28646 = CARTESIAN_POINT ( 'NONE',  ( -1.734723475976807094E-14, 1.040834085586084257E-14, -45.00000000000000000 ) ) ;
#28647 = CIRCLE ( 'NONE', #31000, 31.99999999999998579 ) ;
#28648 = CYLINDRICAL_SURFACE ( 'NONE', #24307, 16.00000000000000000 ) ;
#28649 = CYLINDRICAL_SURFACE ( 'NONE', #7353, 82.00000000000000000 ) ;
#28650 = DIRECTION ( 'NONE',  ( -0.000000000000000000, -0.000000000000000000, -1.000000000000000000 ) ) ;
#28651 = EDGE_CURVE ( 'NONE', #40154, #16137, #33684, .T. ) ;
#28652 = FACE_OUTER_BOUND ( 'NONE', #23094, .T. ) ;
#28653 = ORIENTED_EDGE ( 'NONE', *, *, #8512, .T. ) ;
#28654 = CIRCLE ( 'NONE', #7548, 32.00000000000000000 ) ;
#28655 = DIRECTION ( 'NONE',  ( 1.000000000000000000, 0.000000000000000000, 0.000000000000000000 ) ) ;
#28656 = CARTESIAN_POINT ( 'NONE',  ( 15.00000000000000000, 22.07842321921492612, 8.187992925817123790 ) ) ;
#28657 = CARTESIAN_POINT ( 'NONE',  ( 0.000000000000000000, 16.83928648764923253, 16.46020748918050458 ) ) ;
#28658 = DIRECTION ( 'NONE',  ( 0.000000000000000000, 0.000000000000000000, 1.000000000000000000 ) ) ;
#28659 = CARTESIAN_POINT ( 'NONE',  ( 11.99999999999999822, -64.81221759200380461, 50.23322058963326242 ) ) ;
#28660 = CIRCLE ( 'NONE', #37248, 77.49900000000000944 ) ;
#28661 = DIRECTION ( 'NONE',  ( -1.000000000000000000, 0.000000000000000000, 0.000000000000000000 ) ) ;
#28662 = DIRECTION ( 'NONE',  ( 1.000000000000000000, -0.000000000000000000, -0.000000000000000000 ) ) ;
#28663 = VERTEX_POINT ( 'NONE', #20095 ) ;
#28664 = VERTEX_POINT ( 'NONE', #16424 ) ;
#28665 = VERTEX_POINT ( 'NONE', #34055 ) ;
#28666 = AXIS2_PLACEMENT_3D ( 'NONE', #19258, #22684, #18539 ) ;
#28667 = FACE_OUTER_BOUND ( 'NONE', #48232, .T. ) ;
#28668 = ITEM_DEFINED_TRANSFORMATION ( 'NONE', 'NONE', #38971,  #11636 ) ;
#28669 = FACE_OUTER_BOUND ( 'NONE', #8439, .T. ) ;
#28670 = CIRCLE ( 'NONE', #5333, 37.49900000000000944 ) ;
#28671 = ORIENTED_EDGE ( 'NONE', *, *, #34576, .F. ) ;
#28672 = CIRCLE ( 'NONE', #26328, 77.49899999999999523 ) ;
#28673 = CIRCLE ( 'NONE', #4430, 77.49899999999999523 ) ;
#28674 = EDGE_CURVE ( 'NONE', #18434, #43657, #22748, .T. ) ;
#28675 = PLANE ( 'NONE',  #42190 ) ;
#28676 = ORIENTED_EDGE ( 'NONE', *, *, #34237, .T. ) ;
#28677 = CYLINDRICAL_SURFACE ( 'NONE', #30778, 16.00000000000000000 ) ;
#28678 = ADVANCED_FACE ( 'NONE', ( #41646 ), #15466, .T. ) ;
#28679 = VECTOR ( 'NONE', #6323, 1000.000000000000000 ) ;
#28680 = ORIENTED_EDGE ( 'NONE', *, *, #14208, .T. ) ;
#28681 = DIRECTION ( 'NONE',  ( -1.000000000000000000, 0.000000000000000000, -0.000000000000000000 ) ) ;
#28682 = ADVANCED_FACE ( 'NONE', ( #45311 ), #11789, .T. ) ;
#28683 = VERTEX_POINT ( 'NONE', #758 ) ;
#28684 = CARTESIAN_POINT ( 'NONE',  ( 0.000000000000000000, -37.01155633439063308, 6.555932627142289526 ) ) ;
#28685 = VECTOR ( 'NONE', #42926, 1000.000000000000000 ) ;
#28686 = DIRECTION ( 'NONE',  ( -1.000000000000000000, 0.000000000000000000, 0.000000000000000000 ) ) ;
#28687 = ORIENTED_EDGE ( 'NONE', *, *, #23480, .F. ) ;
#28688 = FACE_OUTER_BOUND ( 'NONE', #36890, .T. ) ;
#28689 = ORIENTED_EDGE ( 'NONE', *, *, #10868, .T. ) ;
#28690 = VERTEX_POINT ( 'NONE', #12287 ) ;
#28691 = AXIS2_PLACEMENT_3D ( 'NONE', #1870, #28285, #12890 ) ;
#28692 = CARTESIAN_POINT ( 'NONE',  ( 10.00000000000000000, -17.28742895386139722, 75.54627589209937355 ) ) ;
#28693 = EDGE_CURVE ( 'NONE', #45549, #42124, #5564, .T. ) ;
#28694 = DIRECTION ( 'NONE',  ( -1.000000000000000000, 0.000000000000000000, -0.000000000000000000 ) ) ;
#28695 = FACE_OUTER_BOUND ( 'NONE', #12905, .T. ) ;
#28696 = ADVANCED_FACE ( 'NONE', ( #34526 ), #1000, .T. ) ;
#28697 = CARTESIAN_POINT ( 'NONE',  ( 0.000000000000000000, 72.35160999960844208, -20.41045688087747223 ) ) ;
#28698 = DIRECTION ( 'NONE',  ( -1.000000000000000000, 0.000000000000000000, 0.000000000000000000 ) ) ;
#28699 = ORIENTED_EDGE ( 'NONE', *, *, #33866, .F. ) ;
#28700 = CARTESIAN_POINT ( 'NONE',  ( 10.00000000000000000, 17.80606268964540462, 33.00180498840053644 ) ) ;
#28701 = ORIENTED_EDGE ( 'NONE', *, *, #34719, .T. ) ;
#28702 = VERTEX_POINT ( 'NONE', #33222 ) ;
#28703 = EDGE_CURVE ( 'NONE', #18490, #18399, #33748, .T. ) ;
#28704 = CYLINDRICAL_SURFACE ( 'NONE', #24699, 82.00000000000000000 ) ;
#28705 = ORIENTED_EDGE ( 'NONE', *, *, #37922, .T. ) ;
#28706 = CYLINDRICAL_SURFACE ( 'NONE', #307, 77.49899999999999523 ) ;
#28707 = FACE_OUTER_BOUND ( 'NONE', #1550, .T. ) ;
#28708 = DIRECTION ( 'NONE',  ( 0.000000000000000000, -0.1564344650402172410, -0.9876883405951399908 ) ) ;
#28709 = VERTEX_POINT ( 'NONE', #43751 ) ;
#28710 = DIRECTION ( 'NONE',  ( -1.000000000000000000, -0.000000000000000000, -0.000000000000000000 ) ) ;
#28711 = CYLINDRICAL_SURFACE ( 'NONE', #10400, 77.49899999999999523 ) ;
#28712 = PLANE ( 'NONE',  #47008 ) ;
#28713 = EDGE_CURVE ( 'NONE', #14416, #40294, #26705, .T. ) ;
#28714 = DIRECTION ( 'NONE',  ( -1.000000000000000000, -0.000000000000000000, -0.000000000000000000 ) ) ;
#28715 = CIRCLE ( 'NONE', #26373, 77.49899999999999523 ) ;
#28716 = CARTESIAN_POINT ( 'NONE',  ( 10.00000000000000000, 33.79645857604513992, 16.45098606841138178 ) ) ;
#28717 = DIRECTION ( 'NONE',  ( -1.000000000000000000, 0.000000000000000000, 0.000000000000000000 ) ) ;
#28718 = CARTESIAN_POINT ( 'NONE',  ( 5.000000000000002665, -39.47590169984897557, 71.87247863392401825 ) ) ;
#28719 = CARTESIAN_POINT ( 'NONE',  ( 10.00000000000000000, -41.76106447765443619, -62.50884508063471401 ) ) ;
#28720 = AXIS2_PLACEMENT_3D ( 'NONE', #19718, #22681, #30289 ) ;
#28721 = DIRECTION ( 'NONE',  ( 0.000000000000000000, 0.000000000000000000, 1.000000000000000000 ) ) ;
#28722 = CARTESIAN_POINT ( 'NONE',  ( -2.981742216678212820, 1.885622467846870828E-15, 15.39727592608509177 ) ) ;
#28723 = VERTEX_POINT ( 'NONE', #48149 ) ;
#28724 = DIRECTION ( 'NONE',  ( -1.000000000000000000, -0.000000000000000000, -0.000000000000000000 ) ) ;
#28725 = AXIS2_PLACEMENT_3D ( 'NONE', #22807, #33811, #44598 ) ;
#28726 = VERTEX_POINT ( 'NONE', #14634 ) ;
#28727 = CARTESIAN_POINT ( 'NONE',  ( 0.000000000000000000, 40.68715046381927891, 10.41901085202092858 ) ) ;
#28728 = CARTESIAN_POINT ( 'NONE',  ( 11.99999999999999822, 0.000000000000000000, 0.000000000000000000 ) ) ;
#28729 = ORIENTED_EDGE ( 'NONE', *, *, #8183, .T. ) ;
#28730 = CIRCLE ( 'NONE', #7620, 12.50000000000000000 ) ;
#28731 = CARTESIAN_POINT ( 'NONE',  ( 26.47460221209471598, -121.8961639463267090, 5.500000000000000000 ) ) ;
#28732 = EDGE_CURVE ( 'NONE', #2823, #3259, #36855, .T. ) ;
#28733 = ORIENTED_EDGE ( 'NONE', *, *, #10103, .T. ) ;
#28734 = EDGE_LOOP ( 'NONE', ( #48185, #36382, #14095, #10007 ) ) ;
#28735 = EDGE_CURVE ( 'NONE', #28861, #11806, #32943, .T. ) ;
#28736 = ORIENTED_EDGE ( 'NONE', *, *, #47501, .T. ) ;
#28737 = ADVANCED_FACE ( 'NONE', ( #25862 ), #18034, .T. ) ;
#28738 = FACE_OUTER_BOUND ( 'NONE', #38364, .T. ) ;
#28739 = EDGE_LOOP ( 'NONE', ( #46930, #37967, #3865, #45006 ) ) ;
#28740 = ADVANCED_FACE ( 'NONE', ( #21481 ), #47893, .T. ) ;
#28741 = DIRECTION ( 'NONE',  ( -1.000000000000000000, 0.000000000000000000, -0.000000000000000000 ) ) ;
#28742 = LINE ( 'NONE', #24825, #42627 ) ;
#28743 = VERTEX_POINT ( 'NONE', #24245 ) ;
#28744 = CIRCLE ( 'NONE', #21717, 16.00000000000000000 ) ;
#28745 = DIRECTION ( 'NONE',  ( -1.000000000000000000, -0.000000000000000000, -0.000000000000000000 ) ) ;
#28746 = ORIENTED_EDGE ( 'NONE', *, *, #25222, .F. ) ;
#28747 = CARTESIAN_POINT ( 'NONE',  ( 10.00000000000000000, 0.000000000000000000, 0.000000000000000000 ) ) ;
#28748 = CYLINDRICAL_SURFACE ( 'NONE', #40584, 16.00000000000000000 ) ;
#28749 = EDGE_CURVE ( 'NONE', #22296, #38875, #27946, .T. ) ;
#28750 = DIRECTION ( 'NONE',  ( -1.000000000000000000, -0.000000000000000000, -0.000000000000000000 ) ) ;
#28751 = ORIENTED_EDGE ( 'NONE', *, *, #15469, .F. ) ;
#28752 = CARTESIAN_POINT ( 'NONE',  ( -7.572224309238338336, -145.4393675041377492, 5.500000000000000000 ) ) ;
#28753 = VERTEX_POINT ( 'NONE', #35260 ) ;
#28754 = ORIENTED_EDGE ( 'NONE', *, *, #39262, .T. ) ;
#28755 = EDGE_CURVE ( 'NONE', #24623, #28899, #32728, .T. ) ;
#28756 = FACE_BOUND ( 'NONE', #30903, .T. ) ;
#28757 = DIRECTION ( 'NONE',  ( 0.000000000000000000, 0.000000000000000000, 1.000000000000000000 ) ) ;
#28758 = DIRECTION ( 'NONE',  ( -1.000000000000000000, -0.000000000000000000, 0.000000000000000000 ) ) ;
#28759 = DIRECTION ( 'NONE',  ( 0.000000000000000000, 0.000000000000000000, 1.000000000000000000 ) ) ;
#28760 = FACE_OUTER_BOUND ( 'NONE', #15407, .T. ) ;
#28761 = LINE ( 'NONE', #28270, #30704 ) ;
#28762 = FACE_OUTER_BOUND ( 'NONE', #15019, .T. ) ;
#28763 = DIRECTION ( 'NONE',  ( 0.000000000000000000, -0.9876883405951393247, 0.1564344650402205161 ) ) ;
#28764 = DIRECTION ( 'NONE',  ( 1.000000000000000000, -0.000000000000000000, -0.000000000000000000 ) ) ;
#28765 = ADVANCED_FACE ( 'NONE', ( #10944 ), #40805, .T. ) ;
#28766 = FACE_OUTER_BOUND ( 'NONE', #452, .T. ) ;
#28767 = ORIENTED_EDGE ( 'NONE', *, *, #27098, .T. ) ;
#28768 = ORIENTED_EDGE ( 'NONE', *, *, #36720, .F. ) ;
#28769 = FACE_OUTER_BOUND ( 'NONE', #8340, .T. ) ;
#28770 = CARTESIAN_POINT ( 'NONE',  ( 10.00000000000000000, 46.53671651294032330, -59.03961581697353012 ) ) ;
#28771 = CARTESIAN_POINT ( 'NONE',  ( 0.000000000000000000, 22.07842321921492612, -8.187992925817130896 ) ) ;
#28772 = CARTESIAN_POINT ( 'NONE',  ( -1.192633404626841198, -119.0902607174754451, 2.500000000000000000 ) ) ;
#28773 = EDGE_CURVE ( 'NONE', #34988, #19466, #45455, .T. ) ;
#28774 = DIRECTION ( 'NONE',  ( -0.000000000000000000, 0.9781476007338067991, 0.2079116908177533474 ) ) ;
#28775 = DIRECTION ( 'NONE',  ( 1.000000000000000000, 0.000000000000000000, 0.000000000000000000 ) ) ;
#28776 = ORIENTED_EDGE ( 'NONE', *, *, #28616, .F. ) ;
#28777 = DIRECTION ( 'NONE',  ( -1.000000000000000000, -0.000000000000000000, 0.000000000000000000 ) ) ;
#28778 = AXIS2_PLACEMENT_3D ( 'NONE', #33101, #48033, #15960 ) ;
#28779 = AXIS2_PLACEMENT_3D ( 'NONE', #33437, #37831, #30486 ) ;
#28780 = CARTESIAN_POINT ( 'NONE',  ( 12.00000000000000000, -19.89357724625003598, -12.59942793731059041 ) ) ;
#28781 = ORIENTED_EDGE ( 'NONE', *, *, #45056, .F. ) ;
#28782 = VERTEX_POINT ( 'NONE', #17561 ) ;
#28783 = ORIENTED_EDGE ( 'NONE', *, *, #22914, .T. ) ;
#28784 = EDGE_CURVE ( 'NONE', #25492, #22951, #7025, .T. ) ;
#28785 = ORIENTED_EDGE ( 'NONE', *, *, #28301, .T. ) ;
#28786 = EDGE_CURVE ( 'NONE', #32136, #39596, #131, .T. ) ;
#28787 = CARTESIAN_POINT ( 'NONE',  ( 10.00000000000000000, 12.26510123303259725, 35.53030884539089840 ) ) ;
#28788 = ORIENTED_EDGE ( 'NONE', *, *, #6394, .F. ) ;
#28789 = EDGE_CURVE ( 'NONE', #41579, #35990, #15008, .T. ) ;
#28790 = CIRCLE ( 'NONE', #20193, 77.49899999999999523 ) ;
#28791 = VERTEX_POINT ( 'NONE', #46536 ) ;
#28792 = EDGE_CURVE ( 'NONE', #20404, #7367, #5610, .T. ) ;
#28793 = DIRECTION ( 'NONE',  ( 0.000000000000000000, 0.000000000000000000, 1.000000000000000000 ) ) ;
#28795 = ORIENTED_EDGE ( 'NONE', *, *, #45820, .F. ) ;
#28794 = DIRECTION ( 'NONE',  ( 0.000000000000000000, 0.000000000000000000, 1.000000000000000000 ) ) ;
#28796 = EDGE_LOOP ( 'NONE', ( #23372, #36026, #18552, #41513 ) ) ;
#28797 = DIRECTION ( 'NONE',  ( -1.000000000000000000, -0.000000000000000000, -0.000000000000000000 ) ) ;
#28798 = ORIENTED_EDGE ( 'NONE', *, *, #16573, .F. ) ;
#28799 = ORIENTED_EDGE ( 'NONE', *, *, #44864, .T. ) ;
#28800 = FACE_OUTER_BOUND ( 'NONE', #22232, .T. ) ;
#28802 = EDGE_LOOP ( 'NONE', ( #23073, #26009, #8101, #38993 ) ) ;
#28801 = CARTESIAN_POINT ( 'NONE',  ( 11.41210121379328335, -99.40233154247455616, -5.500000000000000000 ) ) ;
#28803 = DIRECTION ( 'NONE',  ( 0.000000000000000000, 0.000000000000000000, -1.000000000000000000 ) ) ;
#28804 = VERTEX_POINT ( 'NONE', #47431 ) ;
#28805 = EDGE_LOOP ( 'NONE', ( #15880, #31307, #4611, #15954 ) ) ;
#28806 = VERTEX_POINT ( 'NONE', #25141 ) ;
#28807 = DIRECTION ( 'NONE',  ( -1.000000000000000000, -0.000000000000000000, 0.000000000000000000 ) ) ;
#28808 = VERTEX_POINT ( 'NONE', #28821 ) ;
#28809 = CARTESIAN_POINT ( 'NONE',  ( 11.99999999999999822, 12.93880638057426502, -76.41127070299258150 ) ) ;
#28810 = CARTESIAN_POINT ( 'NONE',  ( 10.00000000000000000, -37.22597642581153821, -5.202137450156795850 ) ) ;
#28811 = LINE ( 'NONE', #32491, #11231 ) ;
#28812 = CARTESIAN_POINT ( 'NONE',  ( 0.000000000000000000, -21.60688246758642705, 79.10210256391360417 ) ) ;
#28813 = AXIS2_PLACEMENT_3D ( 'NONE', #34379, #37348, #129 ) ;
#28814 = SURFACE_STYLE_USAGE ( .BOTH. , #43744 ) ;
#28815 = DIRECTION ( 'NONE',  ( 1.000000000000000000, 0.000000000000000000, 0.000000000000000000 ) ) ;
#28816 = ORIENTED_EDGE ( 'NONE', *, *, #11357, .T. ) ;
#28817 = CYLINDRICAL_SURFACE ( 'NONE', #42131, 16.00000000000000000 ) ;
#28818 = ORIENTED_EDGE ( 'NONE', *, *, #9482, .F. ) ;
#28819 = DIRECTION ( 'NONE',  ( -1.000000000000000000, 0.000000000000000000, 0.000000000000000000 ) ) ;
#28820 = VERTEX_POINT ( 'NONE', #10465 ) ;
#28821 = CARTESIAN_POINT ( 'NONE',  ( 11.99999999999999822, -80.55351364060578589, -15.33399622253569383 ) ) ;
#28822 = CIRCLE ( 'NONE', #8623, 16.00000000000000000 ) ;
#28823 = LINE ( 'NONE', #17084, #38531 ) ;
#28824 = DIRECTION ( 'NONE',  ( -0.000000000000000000, -0.000000000000000000, 1.000000000000000000 ) ) ;
#28825 = COLOUR_RGB ( '', 0.08235294, 0.09019608, 0.10196078) ;
#28826 = DIRECTION ( 'NONE',  ( 0.02332147558787822997, 0.9997280174009349762, 0.000000000000000000 ) ) ;
#28827 = CARTESIAN_POINT ( 'NONE',  ( 11.99999999999999822, 6.903761155838878061, -77.19088730480517313 ) ) ;
#28828 = CARTESIAN_POINT ( 'NONE',  ( 0.000000000000000000, 74.65491531819118620, 23.16904090965733332 ) ) ;
#28829 = CARTESIAN_POINT ( 'NONE',  ( -10.00000000000000000, 0.000000000000000000, 0.000000000000000000 ) ) ;
#28830 = DIRECTION ( 'NONE',  ( -1.000000000000000000, -0.000000000000000000, -0.000000000000000000 ) ) ;
#28831 = ORIENTED_EDGE ( 'NONE', *, *, #30432, .T. ) ;
#28832 = ORIENTED_EDGE ( 'NONE', *, *, #5528, .T. ) ;
#28833 = CIRCLE ( 'NONE', #19453, 0.5000000000000004441 ) ;
#28834 = ADVANCED_FACE ( 'NONE', ( #40086 ), #29061, .F. ) ;
#28835 = CIRCLE ( 'NONE', #31978, 77.49899999999999523 ) ;
#28836 = CIRCLE ( 'NONE', #6175, 16.00000000000000355 ) ;
#28837 = CARTESIAN_POINT ( 'NONE',  ( 11.99999999999999822, 55.38113227695858143, -54.21277698773617715 ) ) ;
#28838 = EDGE_CURVE ( 'NONE', #41574, #35415, #17324, .T. ) ;
#28839 = CARTESIAN_POINT ( 'NONE',  ( -5.565113727472255967, 10.17789316117534248, -44.99999999999998579 ) ) ;
#28840 = AXIS2_PLACEMENT_3D ( 'NONE', #10866, #26284, #7673 ) ;
#28841 = ORIENTED_EDGE ( 'NONE', *, *, #29787, .F. ) ;
#28842 = ADVANCED_FACE ( 'NONE', ( #19252 ), #11190, .T. ) ;
#28843 = CARTESIAN_POINT ( 'NONE',  ( 10.00000000000000000, 40.98264845739749518, 9.188173127307441845 ) ) ;
#28844 = EDGE_LOOP ( 'NONE', ( #11103, #21154, #44471, #46943 ) ) ;
#28845 = ORIENTED_EDGE ( 'NONE', *, *, #41012, .F. ) ;
#28846 = EDGE_CURVE ( 'NONE', #25961, #5367, #13432, .T. ) ;
#28847 = ORIENTED_EDGE ( 'NONE', *, *, #11908, .T. ) ;
#28848 = MECHANICAL_DESIGN_GEOMETRIC_PRESENTATION_REPRESENTATION (  '', ( #15484 ), #38160 ) ;
#28849 = CYLINDRICAL_SURFACE ( 'NONE', #43862, 16.00000000000000000 ) ;
#28850 = ORIENTED_EDGE ( 'NONE', *, *, #7948, .T. ) ;
#28851 = DIRECTION ( 'NONE',  ( 1.000000000000000000, 0.000000000000000000, 0.000000000000000000 ) ) ;
#28852 = ORIENTED_EDGE ( 'NONE', *, *, #40404, .T. ) ;
#28853 = CARTESIAN_POINT ( 'NONE',  ( 10.00000000000000000, 0.000000000000000000, 0.000000000000000000 ) ) ;
#28854 = CARTESIAN_POINT ( 'NONE',  ( 10.00000000000000000, 30.80686688397010542, 21.53537804866092387 ) ) ;
#28855 = DIRECTION ( 'NONE',  ( -1.000000000000000000, 0.000000000000000000, 0.000000000000000000 ) ) ;
#28856 = ORIENTED_EDGE ( 'NONE', *, *, #22050, .F. ) ;
#28857 = DIRECTION ( 'NONE',  ( 0.000000000000000000, 0.000000000000000000, 1.000000000000000000 ) ) ;
#28858 = ORIENTED_EDGE ( 'NONE', *, *, #30187, .F. ) ;
#28859 = DIRECTION ( 'NONE',  ( 1.000000000000000000, 0.000000000000000000, -0.000000000000000000 ) ) ;
#28860 = DIRECTION ( 'NONE',  ( 1.000000000000000000, 0.000000000000000000, 0.000000000000000000 ) ) ;
#28861 = VERTEX_POINT ( 'NONE', #41300 ) ;
#28862 = VECTOR ( 'NONE', #3565, 1000.000000000000000 ) ;
#28863 = ORIENTED_EDGE ( 'NONE', *, *, #39758, .F. ) ;
#28864 = CYLINDRICAL_SURFACE ( 'NONE', #32259, 82.00000000000000000 ) ;
#28865 = CARTESIAN_POINT ( 'NONE',  ( 1.250000000000000000, -12.36245420541525597, -1.199999999999999956 ) ) ;
#28866 = ORIENTED_EDGE ( 'NONE', *, *, #7186, .F. ) ;
#28867 = ORIENTED_EDGE ( 'NONE', *, *, #13861, .F. ) ;
#28868 = VECTOR ( 'NONE', #24153, 1000.000000000000000 ) ;
#28869 = DIRECTION ( 'NONE',  ( -1.000000000000000000, 0.000000000000000000, 0.000000000000000000 ) ) ;
#28870 = DIRECTION ( 'NONE',  ( -0.000000000000000000, -1.000000000000000000, -0.000000000000000000 ) ) ;
#28871 = DIRECTION ( 'NONE',  ( -1.000000000000000000, 0.000000000000000000, 0.000000000000000000 ) ) ;
#28872 = CARTESIAN_POINT ( 'NONE',  ( 0.000000000000000000, 74.74816331893430288, 33.71516098798768724 ) ) ;
#28873 = CARTESIAN_POINT ( 'NONE',  ( 11.99999999999999822, 0.000000000000000000, 0.000000000000000000 ) ) ;
#28874 = EDGE_CURVE ( 'NONE', #30819, #7858, #30760, .T. ) ;
#28875 = CARTESIAN_POINT ( 'NONE',  ( 0.000000000000000000, -31.52238457039619490, 27.75498641678731104 ) ) ;
#28876 = AXIS2_PLACEMENT_3D ( 'NONE', #41219, #7675, #44637 ) ;
#28877 = CYLINDRICAL_SURFACE ( 'NONE', #39503, 16.00000000000000000 ) ;
#28878 = EDGE_CURVE ( 'NONE', #10782, #23867, #40780, .T. ) ;
#28879 = CARTESIAN_POINT ( 'NONE',  ( 5.000000000000000000, -55.16347631942998220, -60.67117009219196433 ) ) ;
#28880 = DIRECTION ( 'NONE',  ( -1.000000000000000000, 0.000000000000000000, 0.000000000000000000 ) ) ;
#28881 = DIRECTION ( 'NONE',  ( -1.000000000000000000, 0.000000000000000000, -0.000000000000000000 ) ) ;
#28882 =( NAMED_UNIT ( * ) SI_UNIT ( $, .STERADIAN. ) SOLID_ANGLE_UNIT ( ) );
#28883 = EDGE_CURVE ( 'NONE', #30814, #9128, #46238, .T. ) ;
#28884 = CARTESIAN_POINT ( 'NONE',  ( 0.000000000000000000, -50.95692526931372157, 58.39081064771733054 ) ) ;
#28885 = ORIENTED_EDGE ( 'NONE', *, *, #28883, .T. ) ;
#28886 = VERTEX_POINT ( 'NONE', #414 ) ;
#28887 = LINE ( 'NONE', #39697, #45587 ) ;
#28888 = EDGE_CURVE ( 'NONE', #45584, #34499, #7525, .T. ) ;
#28889 = DIRECTION ( 'NONE',  ( 1.000000000000000000, 0.000000000000000000, -0.000000000000000000 ) ) ;
#28890 = ORIENTED_EDGE ( 'NONE', *, *, #47138, .F. ) ;
#28891 = ADVANCED_FACE ( 'NONE', ( #8239 ), #22456, .F. ) ;
#28892 = EDGE_CURVE ( 'NONE', #13449, #30895, #11451, .T. ) ;
#28893 = VERTEX_POINT ( 'NONE', #26603 ) ;
#28894 = CIRCLE ( 'NONE', #25777, 77.49899999999999523 ) ;
#28895 = AXIS2_PLACEMENT_3D ( 'NONE', #48294, #29934, #309 ) ;
#28896 = DIRECTION ( 'NONE',  ( -1.000000000000000000, 0.000000000000000000, -0.000000000000000000 ) ) ;
#28897 = DIRECTION ( 'NONE',  ( 1.000000000000000000, 0.000000000000000000, 0.000000000000000000 ) ) ;
#28898 = AXIS2_PLACEMENT_3D ( 'NONE', #119, #37573, #41492 ) ;
#28899 = VERTEX_POINT ( 'NONE', #41536 ) ;
#28900 = CYLINDRICAL_SURFACE ( 'NONE', #39127, 42.00000000000000000 ) ;
#28901 = CIRCLE ( 'NONE', #33700, 31.99999999999998579 ) ;
#28902 = ORIENTED_EDGE ( 'NONE', *, *, #1827, .F. ) ;
#28903 = CARTESIAN_POINT ( 'NONE',  ( 0.000000000000000000, 17.28742895386084655, 75.54627589209950145 ) ) ;
#28904 = CIRCLE ( 'NONE', #35160, 82.00000000000000000 ) ;
#28905 = CYLINDRICAL_SURFACE ( 'NONE', #37570, 42.00000000000000000 ) ;
#28906 = ORIENTED_EDGE ( 'NONE', *, *, #11233, .T. ) ;
#28907 = CARTESIAN_POINT ( 'NONE',  ( -9.937067298023317008, 7.583184918921300977, -44.99999999999998579 ) ) ;
#28908 = ORIENTED_EDGE ( 'NONE', *, *, #42116, .T. ) ;
#28909 = CARTESIAN_POINT ( 'NONE',  ( 11.99999999999999822, 39.78640506895604290, 66.50666863322015843 ) ) ;
#28910 = ORIENTED_EDGE ( 'NONE', *, *, #2631, .T. ) ;
#28911 = CARTESIAN_POINT ( 'NONE',  ( 10.00000000000000000, 0.000000000000000000, 0.000000000000000000 ) ) ;
#28912 = CARTESIAN_POINT ( 'NONE',  ( 15.00000000000000000, -22.67460108101782978, -6.353146135317906840 ) ) ;
#28913 = DIRECTION ( 'NONE',  ( 0.000000000000000000, 0.000000000000000000, 1.000000000000000000 ) ) ;
#28915 = ORIENTED_EDGE ( 'NONE', *, *, #17999, .F. ) ;
#28914 = CARTESIAN_POINT ( 'NONE',  ( 10.00000000000000000, -0.6853352020793173072, 37.58145647212453611 ) ) ;
#28916 = CARTESIAN_POINT ( 'NONE',  ( 5.000000000000002665, -80.55351364060599906, 15.33399622253456585 ) ) ;
#28917 = ORIENTED_EDGE ( 'NONE', *, *, #28846, .T. ) ;
#28918 = FACE_OUTER_BOUND ( 'NONE', #15269, .T. ) ;
#28919 = ORIENTED_EDGE ( 'NONE', *, *, #21370, .F. ) ;
#28920 = ORIENTED_EDGE ( 'NONE', *, *, #32325, .T. ) ;
#28921 = DIRECTION ( 'NONE',  ( 0.000000000000000000, 0.000000000000000000, 1.000000000000000000 ) ) ;
#28922 = CARTESIAN_POINT ( 'NONE',  ( 10.00000000000000000, 2.946379043147425492, -75.11764819372145041 ) ) ;
#28923 = ORIENTED_EDGE ( 'NONE', *, *, #32060, .F. ) ;
#28924 = DIRECTION ( 'NONE',  ( 0.000000000000000000, -0.3826834323650772363, -0.9238795325112919565 ) ) ;
#28925 = CARTESIAN_POINT ( 'NONE',  ( -3.000000000000000000, -13.04903810567675038, 19.60159698893425428 ) ) ;
#28926 = CYLINDRICAL_SURFACE ( 'NONE', #5541, 16.00000000000000000 ) ;
#28927 = EDGE_LOOP ( 'NONE', ( #632, #48234, #18504, #42940 ) ) ;
#28928 = CYLINDRICAL_SURFACE ( 'NONE', #44515, 12.49999999999999645 ) ;
#28929 = CARTESIAN_POINT ( 'NONE',  ( -11.99999999999999645, 1.574895783703496238E-15, -12.85999999999999943 ) ) ;
#28930 = CARTESIAN_POINT ( 'NONE',  ( 10.00000000000000000, -12.26510123303234501, -35.53030884539098366 ) ) ;
#28931 = ORIENTED_EDGE ( 'NONE', *, *, #47712, .F. ) ;
#28932 = EDGE_CURVE ( 'NONE', #12123, #40106, #158, .T. ) ;
#28933 = CARTESIAN_POINT ( 'NONE',  ( 15.00000000000000000, -1.278221433540507546, -26.51162292216071492 ) ) ;
#28934 = DIRECTION ( 'NONE',  ( 0.000000000000000000, 0.000000000000000000, -1.000000000000000000 ) ) ;
#28935 = CARTESIAN_POINT ( 'NONE',  ( 0.000000000000000000, -22.74946021919110706, -29.81001611431033282 ) ) ;
#28936 = LINE ( 'NONE', #32392, #38018 ) ;
#28937 = VECTOR ( 'NONE', #32437, 1000.000000000000000 ) ;
#28938 = CIRCLE ( 'NONE', #14096, 77.49899999999999523 ) ;
#28939 = ADVANCED_FACE ( 'NONE', ( #12176 ), #34179, .T. ) ;
#28940 = VERTEX_POINT ( 'NONE', #11916 ) ;
#28941 = EDGE_LOOP ( 'NONE', ( #429, #24951, #11822, #38086 ) ) ;
#28942 = DIRECTION ( 'NONE',  ( -1.000000000000000000, -0.000000000000000000, 0.000000000000000000 ) ) ;
#28943 = LINE ( 'NONE', #25747, #47222 ) ;
#28944 = LINE ( 'NONE', #21617, #12333 ) ;
#28945 = LINE ( 'NONE', #3489, #22535 ) ;
#28946 = EDGE_CURVE ( 'NONE', #39579, #28806, #36100, .T. ) ;
#28947 = CIRCLE ( 'NONE', #24270, 31.99999999999997868 ) ;
#28948 = CIRCLE ( 'NONE', #23566, 31.99999999999999289 ) ;
#28949 = ORIENTED_EDGE ( 'NONE', *, *, #25003, .F. ) ;
#28950 = DIRECTION ( 'NONE',  ( -1.000000000000000000, 0.000000000000000000, 0.000000000000000000 ) ) ;
#28951 = AXIS2_PLACEMENT_3D ( 'NONE', #38703, #27675, #17354 ) ;
#28952 = VERTEX_POINT ( 'NONE', #26839 ) ;
#28953 = CYLINDRICAL_SURFACE ( 'NONE', #22191, 77.49899999999999523 ) ;
#28954 = EDGE_CURVE ( 'NONE', #12529, #15618, #3845, .T. ) ;
#28955 = DIRECTION ( 'NONE',  ( 1.000000000000000000, 0.000000000000000000, 0.000000000000000000 ) ) ;
#28956 = DIRECTION ( 'NONE',  ( 0.000000000000000000, 0.000000000000000000, 1.000000000000000000 ) ) ;
#28957 = ORIENTED_EDGE ( 'NONE', *, *, #26877, .T. ) ;
#28958 = EDGE_CURVE ( 'NONE', #3684, #11421, #27094, .T. ) ;
#28959 = EDGE_CURVE ( 'NONE', #41768, #4382, #12631, .T. ) ;
#28960 = DIRECTION ( 'NONE',  ( -1.000000000000000000, -0.000000000000000000, -0.000000000000000000 ) ) ;
#28961 = ORIENTED_EDGE ( 'NONE', *, *, #12888, .F. ) ;
#28962 = EDGE_CURVE ( 'NONE', #46699, #7678, #22679, .T. ) ;
#28963 = AXIS2_PLACEMENT_3D ( 'NONE', #31718, #22387, #33156 ) ;
#28964 = DIRECTION ( 'NONE',  ( 1.000000000000000000, 0.000000000000000000, 0.000000000000000000 ) ) ;
#28965 = ORIENTED_EDGE ( 'NONE', *, *, #16082, .F. ) ;
#28966 = DIRECTION ( 'NONE',  ( 0.000000000000000000, 0.000000000000000000, -1.000000000000000000 ) ) ;
#28967 = DIRECTION ( 'NONE',  ( -0.000000000000000000, -0.4067366430757898277, -0.9135454576426055295 ) ) ;
#28968 = CIRCLE ( 'NONE', #18030, 30.50000000000000000 ) ;
#28969 = AXIS2_PLACEMENT_3D ( 'NONE', #31837, #20066, #27424 ) ;
#28970 = ORIENTED_EDGE ( 'NONE', *, *, #12897, .F. ) ;
#28971 = CARTESIAN_POINT ( 'NONE',  ( 11.99999999999999822, 74.65491531819118620, -8.830959090342659579 ) ) ;
#28972 = ORIENTED_EDGE ( 'NONE', *, *, #19715, .T. ) ;
#28973 = AXIS2_PLACEMENT_3D ( 'NONE', #38442, #12743, #9072 ) ;
#28974 = CYLINDRICAL_SURFACE ( 'NONE', #23321, 21.00000000000000000 ) ;
#28975 = DIRECTION ( 'NONE',  ( -0.000000000000000000, -0.000000000000000000, -1.000000000000000000 ) ) ;
#28976 = DIRECTION ( 'NONE',  ( -1.000000000000000000, 0.000000000000000000, 0.000000000000000000 ) ) ;
#28977 = ORIENTED_EDGE ( 'NONE', *, *, #33805, .T. ) ;
#28978 = CIRCLE ( 'NONE', #4777, 82.00000000000000000 ) ;
#28979 = DIRECTION ( 'NONE',  ( -0.5200609990133016058, -0.8541291221503261033, 0.000000000000000000 ) ) ;
#28980 = ORIENTED_EDGE ( 'NONE', *, *, #11617, .T. ) ;
#28981 = VERTEX_POINT ( 'NONE', #37131 ) ;
#28982 = FACE_BOUND ( 'NONE', #31699, .T. ) ;
#28983 = CARTESIAN_POINT ( 'NONE',  ( 0.000000000000000000, -2.946379043145784582, -75.11764819372150725 ) ) ;
#28984 = CYLINDRICAL_SURFACE ( 'NONE', #32075, 16.00000000000000000 ) ;
#28985 = CARTESIAN_POINT ( 'NONE',  ( 10.00000000000000000, -5.202137450156129717, -37.22597642581163768 ) ) ;
#28986 = EDGE_LOOP ( 'NONE', ( #30388, #16481, #23728, #29830 ) ) ;
#28987 = CARTESIAN_POINT ( 'NONE',  ( 0.000000000000000000, 1.530808498934191521E-15, -12.50000000000000000 ) ) ;
#28988 = DIRECTION ( 'NONE',  ( -1.000000000000000000, 0.000000000000000000, 0.000000000000000000 ) ) ;
#28989 = LINE ( 'NONE', #32440, #31314 ) ;
#28990 = CARTESIAN_POINT ( 'NONE',  ( 10.00000000000000000, 22.64427369931169309, 30.00120703465213623 ) ) ;
#28991 = DIRECTION ( 'NONE',  ( 0.000000000000000000, 0.000000000000000000, -1.000000000000000000 ) ) ;
#28992 = CARTESIAN_POINT ( 'NONE',  ( -3.000000000000000000, -13.04903810567675038, 19.60159698893425428 ) ) ;
#28993 = ORIENTED_EDGE ( 'NONE', *, *, #10719, .F. ) ;
#28994 = ORIENTED_EDGE ( 'NONE', *, *, #16008, .F. ) ;
#28995 = CARTESIAN_POINT ( 'NONE',  ( 10.00000000000000000, 39.04073710021344112, 15.48615015657596317 ) ) ;
#28996 = ADVANCED_FACE ( 'NONE', ( #45208 ), #39303, .T. ) ;
#28997 = DIRECTION ( 'NONE',  ( 0.000000000000000000, -0.8910065241883627918, -0.4539904997395568520 ) ) ;
#28998 = DIRECTION ( 'NONE',  ( 0.000000000000000000, 0.7071067811865437980, 0.7071067811865512365 ) ) ;
#28999 = ADVANCED_FACE ( 'NONE', ( #5779 ), #20700, .T. ) ;
#29000 = LINE ( 'NONE', #48329, #459 ) ;
#29001 = AXIS2_PLACEMENT_3D ( 'NONE', #9369, #24306, #9604 ) ;
#29002 = CARTESIAN_POINT ( 'NONE',  ( 10.00000000000000000, 24.73286445877808148, -73.44644590900034586 ) ) ;
#29003 = CARTESIAN_POINT ( 'NONE',  ( -10.43921258969510824, -98.89258801967538659, -5.500000000000000000 ) ) ;
#29004 = CIRCLE ( 'NONE', #41531, 16.00000000000000000 ) ;
#29006 = EDGE_CURVE ( 'NONE', #45331, #43377, #45935, .T. ) ;
#29005 = EDGE_LOOP ( 'NONE', ( #30375, #2537, #31763, #31265 ) ) ;
#29007 = DIRECTION ( 'NONE',  ( -1.000000000000000000, -0.000000000000000000, -0.000000000000000000 ) ) ;
#29008 = CIRCLE ( 'NONE', #12595, 77.49899999999999523 ) ;
#29009 = VECTOR ( 'NONE', #16343, 1000.000000000000000 ) ;
#29010 = CARTESIAN_POINT ( 'NONE',  ( 0.000000000000000000, -36.73666225445940370, 65.58780272294062286 ) ) ;
#29011 = AXIS2_PLACEMENT_3D ( 'NONE', #1981, #39893, #17605 ) ;
#29012 = EDGE_LOOP ( 'NONE', ( #37291, #9381, #44502, #47934 ) ) ;
#29013 = EDGE_LOOP ( 'NONE', ( #47029, #38943, #38130, #8390 ) ) ;
#29014 = ADVANCED_FACE ( 'NONE', ( #1868 ), #27331, .F. ) ;
#29015 = AXIS2_PLACEMENT_3D ( 'NONE', #27943, #46533, #27445 ) ;
#29016 = CIRCLE ( 'NONE', #27348, 12.49999999999999645 ) ;
#29017 = ORIENTED_EDGE ( 'NONE', *, *, #25155, .F. ) ;
#29018 = EDGE_CURVE ( 'NONE', #13986, #5941, #42982, .T. ) ;
#29019 = LINE ( 'NONE', #17522, #39860 ) ;
#29020 = ORIENTED_EDGE ( 'NONE', *, *, #14032, .T. ) ;
#29021 = ORIENTED_EDGE ( 'NONE', *, *, #23599, .T. ) ;
#29022 = EDGE_CURVE ( 'NONE', #17719, #13778, #14193, .T. ) ;
#29023 = CIRCLE ( 'NONE', #37632, 42.00000000000000000 ) ;
#29024 = DIRECTION ( 'NONE',  ( 0.9730327541852497042, -0.2306669878475622604, 0.000000000000000000 ) ) ;
#29025 = CARTESIAN_POINT ( 'NONE',  ( 10.00000000000000000, 50.95692526931328104, 58.39081064771769292 ) ) ;
#29027 = EDGE_LOOP ( 'NONE', ( #27006, #13102, #44796, #3954 ) ) ;
#29026 = DIRECTION ( 'NONE',  ( 0.000000000000000000, 0.000000000000000000, 1.000000000000000000 ) ) ;
#29028 = VERTEX_POINT ( 'NONE', #20450 ) ;
#29029 = DIRECTION ( 'NONE',  ( 0.2306669878475647861, 0.9730327541852491491, 0.000000000000000000 ) ) ;
#29030 = ORIENTED_EDGE ( 'NONE', *, *, #26060, .T. ) ;
#29031 = ORIENTED_EDGE ( 'NONE', *, *, #37952, .F. ) ;
#29032 = DIRECTION ( 'NONE',  ( 0.1850432970638667407, -0.9827303690289282967, 0.000000000000000000 ) ) ;
#29033 = CARTESIAN_POINT ( 'NONE',  ( 15.00000000000000000, -22.32062822937489344, -14.36278369418800160 ) ) ;
#29034 = VECTOR ( 'NONE', #18997, 1000.000000000000000 ) ;
#29035 = ADVANCED_FACE ( 'NONE', ( #23896 ), #16798, .T. ) ;
#29036 = CARTESIAN_POINT ( 'NONE',  ( 10.00000000000000000, -12.26510123303284594, 35.53030884539080603 ) ) ;
#29037 = ORIENTED_EDGE ( 'NONE', *, *, #41565, .T. ) ;
#29039 = ORIENTED_EDGE ( 'NONE', *, *, #21488, .F. ) ;
#29038 = VECTOR ( 'NONE', #37939, 1000.000000000000000 ) ;
#29040 = ORIENTED_EDGE ( 'NONE', *, *, #42371, .F. ) ;
#29041 = DIRECTION ( 'NONE',  ( -1.000000000000000000, -0.000000000000000000, -0.000000000000000000 ) ) ;
#29042 = ORIENTED_EDGE ( 'NONE', *, *, #17802, .T. ) ;
#29043 = AXIS2_PLACEMENT_3D ( 'NONE', #44089, #40908, #47994 ) ;
#29044 = DIRECTION ( 'NONE',  ( -1.000000000000000000, 0.000000000000000000, 0.000000000000000000 ) ) ;
#29045 = CARTESIAN_POINT ( 'NONE',  ( -10.00000000000000000, 0.000000000000000000, 0.000000000000000000 ) ) ;
#29046 = CARTESIAN_POINT ( 'NONE',  ( -3.000000000000000000, -19.89357724625003598, 12.59942793731059574 ) ) ;
#29047 = ORIENTED_EDGE ( 'NONE', *, *, #12906, .T. ) ;
#29048 = CARTESIAN_POINT ( 'NONE',  ( 0.000000000000000000, 0.000000000000000000, 0.000000000000000000 ) ) ;
#29049 = CARTESIAN_POINT ( 'NONE',  ( 0.000000000000000000, 0.000000000000000000, -54.99999999999998579 ) ) ;
#29050 = CARTESIAN_POINT ( 'NONE',  ( 0.000000000000000000, -77.49459641780886443, 0.8261519478428549501 ) ) ;
#29051 = DIRECTION ( 'NONE',  ( -1.000000000000000000, 0.000000000000000000, 0.000000000000000000 ) ) ;
#29052 = DIRECTION ( 'NONE',  ( -0.000000000000000000, -0.000000000000000000, -1.000000000000000000 ) ) ;
#29053 = ORIENTED_EDGE ( 'NONE', *, *, #3696, .T. ) ;
#29054 = ADVANCED_FACE ( 'NONE', ( #5057 ), #19973, .T. ) ;
#29055 = DIRECTION ( 'NONE',  ( -1.000000000000000000, 0.000000000000000000, 0.000000000000000000 ) ) ;
#29056 = ORIENTED_EDGE ( 'NONE', *, *, #24051, .F. ) ;
#29057 = AXIS2_PLACEMENT_3D ( 'NONE', #30138, #33777, #23266 ) ;
#29058 = EDGE_CURVE ( 'NONE', #2304, #5392, #2108, .T. ) ;
#29059 = CARTESIAN_POINT ( 'NONE',  ( -22.53294031248082163, -134.0273518838794757, -5.500000000000000000 ) ) ;
#29060 = ORIENTED_EDGE ( 'NONE', *, *, #28293, .F. ) ;
#29061 = PLANE ( 'NONE',  #44686 ) ;
#29062 = DIRECTION ( 'NONE',  ( 0.000000000000000000, 0.000000000000000000, 1.000000000000000000 ) ) ;
#29063 = ADVANCED_FACE ( 'NONE', ( #46661 ), #13124, .T. ) ;
#29064 = DIRECTION ( 'NONE',  ( 0.000000000000000000, -0.5224985647159380298, -0.8526401643540988395 ) ) ;
#29065 = LINE ( 'NONE', #14387, #44364 ) ;
#29066 = ADVANCED_FACE ( 'NONE', ( #8476 ), #35635, .F. ) ;
#29067 = VERTEX_POINT ( 'NONE', #31980 ) ;
#29068 = CARTESIAN_POINT ( 'NONE',  ( 11.99999999999999822, 46.21855187248630870, 62.20884554314035597 ) ) ;
#29069 = DIRECTION ( 'NONE',  ( 0.000000000000000000, -0.8090169943749422332, -0.5877852522924803536 ) ) ;
#29070 = DIRECTION ( 'NONE',  ( -0.000000000000000000, -0.000000000000000000, -1.000000000000000000 ) ) ;
#29071 = ADVANCED_FACE ( 'NONE', ( #9431 ), #38339, .T. ) ;
#29072 = ORIENTED_EDGE ( 'NONE', *, *, #25751, .T. ) ;
#29073 = DIRECTION ( 'NONE',  ( -0.6862798483830544471, -0.7273375899149802093, 0.000000000000000000 ) ) ;
#29074 = ORIENTED_EDGE ( 'NONE', *, *, #3294, .F. ) ;
#29075 = ORIENTED_EDGE ( 'NONE', *, *, #38235, .T. ) ;
#29076 = CIRCLE ( 'NONE', #26741, 77.49900000000000944 ) ;
#29077 = AXIS2_PLACEMENT_3D ( 'NONE', #9353, #34818, #47047 ) ;
#29078 = DIRECTION ( 'NONE',  ( -1.000000000000000000, 0.000000000000000000, -0.000000000000000000 ) ) ;
#29079 = DIRECTION ( 'NONE',  ( -0.2867529058022035837, 0.9580045777625452175, 0.000000000000000000 ) ) ;
#29080 = ORIENTED_EDGE ( 'NONE', *, *, #16214, .F. ) ;
#29081 = EDGE_CURVE ( 'NONE', #23433, #5548, #46170, .T. ) ;
#29082 = CARTESIAN_POINT ( 'NONE',  ( 10.00000000000000000, 18.89407956138362010, -75.16055320797013906 ) ) ;
#29083 = VECTOR ( 'NONE', #39883, 1000.000000000000000 ) ;
#29084 = ORIENTED_EDGE ( 'NONE', *, *, #45666, .F. ) ;
#29085 = EDGE_LOOP ( 'NONE', ( #23355, #30347, #31054, #41087 ) ) ;
#29086 = EDGE_CURVE ( 'NONE', #26821, #15059, #23618, .T. ) ;
#29087 = EDGE_CURVE ( 'NONE', #11520, #4178, #47824, .T. ) ;
#29088 = CARTESIAN_POINT ( 'NONE',  ( 0.000000000000000000, -26.08949754953044220, 27.05870788708222818 ) ) ;
#29089 = ORIENTED_EDGE ( 'NONE', *, *, #19067, .F. ) ;
#29090 = CARTESIAN_POINT ( 'NONE',  ( 10.00000000000000000, 30.00120703465205452, 22.64427369931179967 ) ) ;
#29091 = ORIENTED_EDGE ( 'NONE', *, *, #37932, .T. ) ;
#29092 = DIRECTION ( 'NONE',  ( -1.000000000000000000, -0.000000000000000000, -0.000000000000000000 ) ) ;
#29093 = CARTESIAN_POINT ( 'NONE',  ( 0.000000000000000000, -81.90746397400386059, -3.894527615418773347 ) ) ;
#29094 = DIRECTION ( 'NONE',  ( 0.7533909544171998318, 0.6575728627325954090, 0.000000000000000000 ) ) ;
#29095 = EDGE_LOOP ( 'NONE', ( #7426, #47732, #13059, #36653 ) ) ;
#29096 = ORIENTED_EDGE ( 'NONE', *, *, #31085, .F. ) ;
#29097 = VECTOR ( 'NONE', #27275, 1000.000000000000000 ) ;
#29098 = CARTESIAN_POINT ( 'NONE',  ( 11.99999999999999822, -34.94270380257585629, -74.18225833017926618 ) ) ;
#29099 = CARTESIAN_POINT ( 'NONE',  ( 11.99999999999999822, -74.65491531819111515, -8.830959090343204920 ) ) ;
#29100 = VERTEX_POINT ( 'NONE', #1621 ) ;
#29101 = ORIENTED_EDGE ( 'NONE', *, *, #44320, .T. ) ;
#29102 = EDGE_CURVE ( 'NONE', #27731, #20060, #18927, .T. ) ;
#29103 = CARTESIAN_POINT ( 'NONE',  ( 0.000000000000000000, 12.42422080174688404, -35.38097989696498047 ) ) ;
#29104 = CARTESIAN_POINT ( 'NONE',  ( 0.000000000000000000, 0.000000000000000000, 0.000000000000000000 ) ) ;
#29105 = EDGE_LOOP ( 'NONE', ( #29299, #35052, #29131, #28915 ) ) ;
#29106 = CIRCLE ( 'NONE', #1761, 37.49900000000000233 ) ;
#29107 = ORIENTED_EDGE ( 'NONE', *, *, #35159, .F. ) ;
#29108 = CARTESIAN_POINT ( 'NONE',  ( 0.000000000000000000, -81.96053171279901051, -2.543863470249259962 ) ) ;
#29109 = CARTESIAN_POINT ( 'NONE',  ( 11.99999999999999822, 55.20638768913831029, -51.02545421589267960 ) ) ;
#29110 = FACE_OUTER_BOUND ( 'NONE', #45708, .T. ) ;
#29111 = EDGE_CURVE ( 'NONE', #39094, #28609, #42395, .T. ) ;
#29112 = CARTESIAN_POINT ( 'NONE',  ( 0.000000000000000000, -65.58780272294048075, -36.73666225445966660 ) ) ;
#29113 = CYLINDRICAL_SURFACE ( 'NONE', #18541, 32.00000000000000000 ) ;
#29114 = CARTESIAN_POINT ( 'NONE',  ( 11.99999999999999822, 0.000000000000000000, 0.000000000000000000 ) ) ;
#29115 = DIRECTION ( 'NONE',  ( 0.000000000000000000, 0.000000000000000000, 1.000000000000000000 ) ) ;
#29116 = ADVANCED_FACE ( 'NONE', ( #28281, #17749 ), #32210, .T. ) ;
#29117 = CIRCLE ( 'NONE', #37725, 37.49900000000000944 ) ;
#29118 = ADVANCED_FACE ( 'NONE', ( #47597 ), #40512, .T. ) ;
#29119 = CARTESIAN_POINT ( 'NONE',  ( 11.99999999999999822, 0.000000000000000000, 0.000000000000000000 ) ) ;
#29120 = LINE ( 'NONE', #33032, #46470 ) ;
#29121 = CARTESIAN_POINT ( 'NONE',  ( 10.00000000000000000, 35.38097989696528600, -12.42422080174602605 ) ) ;
#29122 = ORIENTED_EDGE ( 'NONE', *, *, #32639, .T. ) ;
#29123 = ORIENTED_EDGE ( 'NONE', *, *, #26943, .T. ) ;
#29124 = VERTEX_POINT ( 'NONE', #32450 ) ;
#29125 = UNCERTAINTY_MEASURE_WITH_UNIT (LENGTH_MEASURE( 1.000000000000000082E-05 ), #48040, 'distance_accuracy_value', 'NONE');
#29126 = FACE_OUTER_BOUND ( 'NONE', #36681, .T. ) ;
#29127 = AXIS2_PLACEMENT_3D ( 'NONE', #7572, #40385, #2922 ) ;
#29128 = CIRCLE ( 'NONE', #17426, 82.00000000000000000 ) ;
#29129 = CYLINDRICAL_SURFACE ( 'NONE', #4235, 77.49899999999999523 ) ;
#29130 = ORIENTED_EDGE ( 'NONE', *, *, #46467, .T. ) ;
#29131 = ORIENTED_EDGE ( 'NONE', *, *, #46816, .F. ) ;
#29132 = AXIS2_PLACEMENT_3D ( 'NONE', #39171, #35740, #27681 ) ;
#29133 = APPLICATION_CONTEXT ( 'automotive_design' ) ;
#29134 = DIRECTION ( 'NONE',  ( 0.000000000000000000, -6.982962677686267499E-15, 1.000000000000000000 ) ) ;
#29135 = AXIS2_PLACEMENT_3D ( 'NONE', #26409, #30325, #689 ) ;
#29136 = ORIENTED_EDGE ( 'NONE', *, *, #25885, .T. ) ;
#29137 = CARTESIAN_POINT ( 'NONE',  ( -10.00000000000000000, 0.000000000000000000, 0.000000000000000000 ) ) ;
#29138 = AXIS2_PLACEMENT_3D ( 'NONE', #16354, #31791, #13163 ) ;
#29139 = EDGE_LOOP ( 'NONE', ( #25812, #26032, #40802, #11864 ) ) ;
#29140 = CARTESIAN_POINT ( 'NONE',  ( -43.60332556124591719, -107.0000000000000000, -2.500000000000002220 ) ) ;
#29141 = VECTOR ( 'NONE', #41301, 1000.000000000000114 ) ;
#29142 = DIRECTION ( 'NONE',  ( -1.000000000000000000, 0.000000000000000000, 0.000000000000000000 ) ) ;
#29143 = AXIS2_PLACEMENT_3D ( 'NONE', #38776, #4507, #18925 ) ;
#29144 = LINE ( 'NONE', #17402, #10210 ) ;
#29145 = CARTESIAN_POINT ( 'NONE',  ( 0.000000000000000000, 16.61724383029361718, 20.69703378468926402 ) ) ;
#29146 = CIRCLE ( 'NONE', #24445, 82.00000000000000000 ) ;
#29147 = EDGE_CURVE ( 'NONE', #40538, #20444, #29076, .T. ) ;
#29148 = ORIENTED_EDGE ( 'NONE', *, *, #19891, .T. ) ;
#29149 = DIRECTION ( 'NONE',  ( 0.000000000000000000, -0.8090169943749531134, 0.5877852522924653655 ) ) ;
#29150 = VERTEX_POINT ( 'NONE', #9928 ) ;
#29151 = DIRECTION ( 'NONE',  ( 1.000000000000000000, 0.000000000000000000, 0.000000000000000000 ) ) ;
#29152 = VERTEX_POINT ( 'NONE', #13851 ) ;
#29153 = DIRECTION ( 'NONE',  ( 0.000000000000000000, 0.000000000000000000, -1.000000000000000000 ) ) ;
#29154 = DIRECTION ( 'NONE',  ( -1.000000000000000000, 0.000000000000000000, -0.000000000000000000 ) ) ;
#29155 = DIRECTION ( 'NONE',  ( -1.000000000000000000, 0.000000000000000000, 0.000000000000000000 ) ) ;
#29156 = CARTESIAN_POINT ( 'NONE',  ( 10.00000000000000000, 0.000000000000000000, 0.000000000000000000 ) ) ;
#29157 = VERTEX_POINT ( 'NONE', #47832 ) ;
#29158 = DIRECTION ( 'NONE',  ( 0.000000000000000000, 0.000000000000000000, 1.000000000000000000 ) ) ;
#29159 = ORIENTED_EDGE ( 'NONE', *, *, #2164, .F. ) ;
#29160 = VERTEX_POINT ( 'NONE', #24619 ) ;
#29161 = CARTESIAN_POINT ( 'NONE',  ( 10.00000000000000000, 0.000000000000000000, 0.000000000000000000 ) ) ;
#29162 = CARTESIAN_POINT ( 'NONE',  ( 11.99999999999999822, -73.72996012237449293, 14.67089635893687571 ) ) ;
#29163 = ORIENTED_EDGE ( 'NONE', *, *, #33819, .F. ) ;
#29164 = CARTESIAN_POINT ( 'NONE',  ( 10.00000000000000000, -20.40083707022829174, -72.35432306680507963 ) ) ;
#29165 = DIRECTION ( 'NONE',  ( 0.000000000000000000, 0.5224985647159500202, -0.8526401643540915121 ) ) ;
#29166 = DIRECTION ( 'NONE',  ( -0.9966891607226786576, -0.08130631524009861166, 0.000000000000000000 ) ) ;
#29167 = EDGE_LOOP ( 'NONE', ( #43711, #34157, #30279, #25207 ) ) ;
#29168 = CIRCLE ( 'NONE', #6502, 82.00000000000000000 ) ;
#29169 = EDGE_CURVE ( 'NONE', #16520, #40761, #11125, .T. ) ;
#29170 = DIRECTION ( 'NONE',  ( 0.000000000000000000, 0.000000000000000000, 1.000000000000000000 ) ) ;
#29171 = ADVANCED_FACE ( 'NONE', ( #24851 ), #6261, .F. ) ;
#29172 = EDGE_CURVE ( 'NONE', #31993, #2457, #7959, .T. ) ;
#29173 = DIRECTION ( 'NONE',  ( 0.000000000000000000, 0.000000000000000000, -1.000000000000000000 ) ) ;
#29174 = AXIS2_PLACEMENT_3D ( 'NONE', #24688, #2629, #17571 ) ;
#29175 = DIRECTION ( 'NONE',  ( 0.000000000000000000, -0.000000000000000000, 1.000000000000000000 ) ) ;
#29176 = CARTESIAN_POINT ( 'NONE',  ( 0.000000000000000000, -0.8261519478425841667, -77.49459641780886443 ) ) ;
#29177 = CYLINDRICAL_SURFACE ( 'NONE', #6681, 82.00000000000000000 ) ;
#29178 = CARTESIAN_POINT ( 'NONE',  ( -10.00000000000000000, 0.000000000000000000, 0.000000000000000000 ) ) ;
#29179 = DIRECTION ( 'NONE',  ( -0.000000000000000000, -0.000000000000000000, -1.000000000000000000 ) ) ;
#29180 = ADVANCED_FACE ( 'NONE', ( #43932 ), #21170, .T. ) ;
#29181 = CIRCLE ( 'NONE', #36955, 37.49900000000000233 ) ;
#29182 = CIRCLE ( 'NONE', #234, 77.49899999999999523 ) ;
#29183 = CIRCLE ( 'NONE', #45601, 31.99999999999999289 ) ;
#29184 = AXIS2_PLACEMENT_3D ( 'NONE', #30746, #22666, #23154 ) ;
#29185 = EDGE_CURVE ( 'NONE', #21061, #10970, #12702, .T. ) ;
#29186 = CARTESIAN_POINT ( 'NONE',  ( -119.3426274441927433, -132.5434155921188619, -5.500000000000000000 ) ) ;
#29187 = DIRECTION ( 'NONE',  ( 0.000000000000000000, 0.5224985647159500202, -0.8526401643540915121 ) ) ;
#29188 = DIRECTION ( 'NONE',  ( 0.000000000000000000, -0.3090169943749349057, -0.9510565162951577500 ) ) ;
#29189 = CARTESIAN_POINT ( 'NONE',  ( 0.000000000000000000, 0.000000000000000000, -54.99999999999998579 ) ) ;
#29190 = AXIS2_PLACEMENT_3D ( 'NONE', #10715, #3601, #25625 ) ;
#29191 = VERTEX_POINT ( 'NONE', #36587 ) ;
#29192 = EDGE_LOOP ( 'NONE', ( #18048, #40545, #41149, #24146 ) ) ;
#29194 = PLANE ( 'NONE',  #15983 ) ;
#29193 = VECTOR ( 'NONE', #41677, 1000.000000000000000 ) ;
#29195 = AXIS2_PLACEMENT_3D ( 'NONE', #28282, #24368, #17023 ) ;
#29196 = ORIENTED_EDGE ( 'NONE', *, *, #1224, .T. ) ;
#29197 = CIRCLE ( 'NONE', #46392, 42.00000000000000000 ) ;
#29198 = LINE ( 'NONE', #40231, #13528 ) ;
#29199 = CIRCLE ( 'NONE', #36217, 42.00000000000000000 ) ;
#29201 = EDGE_CURVE ( 'NONE', #31219, #38104, #33163, .T. ) ;
#29200 = PRODUCT_CONTEXT ( 'NONE', #39159, 'mechanical' ) ;
#29202 = DIRECTION ( 'NONE',  ( -1.000000000000000000, 0.000000000000000000, 0.000000000000000000 ) ) ;
#29203 = CIRCLE ( 'NONE', #3402, 31.99999999999999289 ) ;
#29204 = EDGE_LOOP ( 'NONE', ( #38667, #13806, #12947, #3761 ) ) ;
#29205 = DIRECTION ( 'NONE',  ( -1.000000000000000000, 0.000000000000000000, -0.000000000000000000 ) ) ;
#29207 = ORIENTED_EDGE ( 'NONE', *, *, #23886, .T. ) ;
#29206 = ADVANCED_BREP_SHAPE_REPRESENTATION ( '', ( #3572, #11636 ), #48316 ) ;
#29208 = VERTEX_POINT ( 'NONE', #39797 ) ;
#29209 = VECTOR ( 'NONE', #21123, 1000.000000000000000 ) ;
#29210 = ADVANCED_FACE ( 'NONE', ( #2566 ), #14318, .T. ) ;
#29211 = PLANE ( 'NONE',  #43328 ) ;
#29212 = ORIENTED_EDGE ( 'NONE', *, *, #25453, .F. ) ;
#29213 = CARTESIAN_POINT ( 'NONE',  ( 10.00000000000000000, 0.000000000000000000, 0.000000000000000000 ) ) ;
#29214 = VECTOR ( 'NONE', #24842, 1000.000000000000000 ) ;
#29215 = AXIS2_PLACEMENT_3D ( 'NONE', #44462, #25371, #33447 ) ;
#29216 = DIRECTION ( 'NONE',  ( 1.000000000000000000, 0.000000000000000000, 0.000000000000000000 ) ) ;
#29217 = CIRCLE ( 'NONE', #7343, 82.00000000000000000 ) ;
#29218 = EDGE_CURVE ( 'NONE', #15461, #28709, #18895, .T. ) ;
#29219 = ORIENTED_EDGE ( 'NONE', *, *, #40833, .T. ) ;
#29220 = DIRECTION ( 'NONE',  ( 1.000000000000000000, 0.000000000000000000, 0.000000000000000000 ) ) ;
#29221 = EDGE_CURVE ( 'NONE', #19386, #15851, #9675, .T. ) ;
#29222 = ORIENTED_EDGE ( 'NONE', *, *, #7186, .T. ) ;
#29223 = DIRECTION ( 'NONE',  ( 0.000000000000000000, 0.000000000000000000, 1.000000000000000000 ) ) ;
#29224 = FACE_OUTER_BOUND ( 'NONE', #40265, .T. ) ;
#29225 = DIRECTION ( 'NONE',  ( 0.000000000000000000, 0.000000000000000000, -1.000000000000000000 ) ) ;
#29226 = ORIENTED_EDGE ( 'NONE', *, *, #17169, .F. ) ;
#29227 = AXIS2_PLACEMENT_3D ( 'NONE', #46191, #12667, #37217 ) ;
#29228 = AXIS2_PLACEMENT_3D ( 'NONE', #21359, #42692, #24805 ) ;
#29229 = ORIENTED_EDGE ( 'NONE', *, *, #40556, .F. ) ;
#29230 = FACE_OUTER_BOUND ( 'NONE', #10762, .T. ) ;
#29231 = ORIENTED_EDGE ( 'NONE', *, *, #7328, .F. ) ;
#29232 = ORIENTED_EDGE ( 'NONE', *, *, #26258, .F. ) ;
#29233 = VECTOR ( 'NONE', #473, 1000.000000000000000 ) ;
#29234 = DIRECTION ( 'NONE',  ( -1.000000000000000000, -0.000000000000000000, -0.000000000000000000 ) ) ;
#29235 = CIRCLE ( 'NONE', #32279, 82.00000000000000000 ) ;
#29236 = CYLINDRICAL_SURFACE ( 'NONE', #32449, 42.00000000000000000 ) ;
#29237 = CARTESIAN_POINT ( 'NONE',  ( 10.00000000000000000, 0.000000000000000000, 0.000000000000000000 ) ) ;
#29238 = FACE_OUTER_BOUND ( 'NONE', #27673, .T. ) ;
#29239 = ORIENTED_EDGE ( 'NONE', *, *, #30351, .T. ) ;
#29240 = DIRECTION ( 'NONE',  ( 1.000000000000000000, -0.000000000000000000, -0.000000000000000000 ) ) ;
#29241 = CIRCLE ( 'NONE', #11255, 77.49899999999999523 ) ;
#29242 = CARTESIAN_POINT ( 'NONE',  ( 0.000000000000000000, 17.67226234102826510, 33.17418723428314564 ) ) ;
#29243 = EDGE_CURVE ( 'NONE', #44060, #27986, #6495, .T. ) ;
#29244 = EDGE_CURVE ( 'NONE', #17337, #41232, #20945, .T. ) ;
#29245 = DIRECTION ( 'NONE',  ( -1.000000000000000000, 0.000000000000000000, 0.000000000000000000 ) ) ;
#29246 = DIRECTION ( 'NONE',  ( 0.000000000000000000, 0.7071067811865487940, -0.7071067811865462405 ) ) ;
#29247 = DIRECTION ( 'NONE',  ( -1.000000000000000000, 0.000000000000000000, -0.000000000000000000 ) ) ;
#29248 = ORIENTED_EDGE ( 'NONE', *, *, #38670, .T. ) ;
#29249 = CARTESIAN_POINT ( 'NONE',  ( 10.00000000000000000, 74.65491531819105830, 8.830959090343693418 ) ) ;
#29250 = DIRECTION ( 'NONE',  ( -1.000000000000000000, 0.000000000000000000, -0.000000000000000000 ) ) ;
#29251 = CYLINDRICAL_SURFACE ( 'NONE', #20590, 32.00000000000000000 ) ;
#29252 = DIRECTION ( 'NONE',  ( -1.000000000000000000, 0.000000000000000000, -0.000000000000000000 ) ) ;
#29253 = EDGE_CURVE ( 'NONE', #5920, #25033, #44659, .T. ) ;
#29254 = CIRCLE ( 'NONE', #47252, 16.00000000000000355 ) ;
#29255 = DIRECTION ( 'NONE',  ( 0.000000000000000000, 0.9135454576426002005, 0.4067366430758017071 ) ) ;
#29256 = CARTESIAN_POINT ( 'NONE',  ( 11.99999999999999822, 0.000000000000000000, 0.000000000000000000 ) ) ;
#29257 = ORIENTED_EDGE ( 'NONE', *, *, #19320, .T. ) ;
#29258 = CIRCLE ( 'NONE', #5828, 42.00000000000000000 ) ;
#29259 = LINE ( 'NONE', #22146, #37123 ) ;
#29260 = VECTOR ( 'NONE', #6413, 1000.000000000000000 ) ;
#29261 = PRODUCT_DEFINITION_SHAPE ( 'NONE', 'NONE',  #48461 ) ;
#29262 = LINE ( 'NONE', #47606, #11943 ) ;
#29263 = ORIENTED_EDGE ( 'NONE', *, *, #19765, .F. ) ;
#29264 = ORIENTED_EDGE ( 'NONE', *, *, #9933, .F. ) ;
#29265 = AXIS2_PLACEMENT_3D ( 'NONE', #32001, #27854, #46689 ) ;
#29266 = CIRCLE ( 'NONE', #40217, 82.00000000000000000 ) ;
#29267 = VERTEX_POINT ( 'NONE', #44902 ) ;
#29268 = VECTOR ( 'NONE', #26118, 1000.000000000000000 ) ;
#29269 = ORIENTED_EDGE ( 'NONE', *, *, #2405, .T. ) ;
#29270 = AXIS2_PLACEMENT_3D ( 'NONE', #43055, #12715, #12476 ) ;
#29271 = DIRECTION ( 'NONE',  ( 0.000000000000000000, 0.000000000000000000, 1.000000000000000000 ) ) ;
#29272 = ORIENTED_EDGE ( 'NONE', *, *, #8356, .T. ) ;
#29273 = AXIS2_PLACEMENT_3D ( 'NONE', #1458, #34480, #15653 ) ;
#29274 = VERTEX_POINT ( 'NONE', #19194 ) ;
#29275 = EDGE_CURVE ( 'NONE', #38428, #2295, #19689, .T. ) ;
#29276 = LINE ( 'NONE', #14102, #7384 ) ;
#29277 = CARTESIAN_POINT ( 'NONE',  ( -0.8815729230226008184, -93.47222532549339746, 5.500000000000000000 ) ) ;
#29279 = VERTEX_POINT ( 'NONE', #99 ) ;
#29278 = DIRECTION ( 'NONE',  ( 0.000000000000000000, 0.000000000000000000, 1.000000000000000000 ) ) ;
#29280 = ADVANCED_FACE ( 'NONE', ( #11388 ), #26308, .T. ) ;
#29281 = ORIENTED_EDGE ( 'NONE', *, *, #41969, .T. ) ;
#29282 = CARTESIAN_POINT ( 'NONE',  ( 10.00000000000000000, 26.79245525562714647, 32.34446384429980981 ) ) ;
#29283 = VERTEX_POINT ( 'NONE', #41000 ) ;
#29284 = EDGE_CURVE ( 'NONE', #17996, #14039, #46271, .T. ) ;
#29285 = ORIENTED_EDGE ( 'NONE', *, *, #11947, .F. ) ;
#29286 = DIRECTION ( 'NONE',  ( 0.000000000000000000, 0.000000000000000000, 1.000000000000000000 ) ) ;
#29287 = CARTESIAN_POINT ( 'NONE',  ( 5.000000000000002665, 78.73519480814985627, -22.90783923731548199 ) ) ;
#29289 = CARTESIAN_POINT ( 'NONE',  ( 10.00000000000000000, 39.47590169984943742, -71.87247863392373404 ) ) ;
#29288 = CIRCLE ( 'NONE', #18345, 77.49900000000000944 ) ;
#29290 = ORIENTED_EDGE ( 'NONE', *, *, #41607, .T. ) ;
#29291 = EDGE_LOOP ( 'NONE', ( #11723, #4425, #25104, #43946 ) ) ;
#29292 = ORIENTED_EDGE ( 'NONE', *, *, #15605, .T. ) ;
#29293 = LINE ( 'NONE', #43973, #5242 ) ;
#29294 = ORIENTED_EDGE ( 'NONE', *, *, #16163, .F. ) ;
#29295 = AXIS2_PLACEMENT_3D ( 'NONE', #9661, #32194, #28266 ) ;
#29296 = CARTESIAN_POINT ( 'NONE',  ( 10.00000000000000000, -74.65491531819124305, 8.830959090342128448 ) ) ;
#29297 = CARTESIAN_POINT ( 'NONE',  ( 10.00000000000000000, 16.45098606841173705, -33.79645857604496229 ) ) ;
#29298 = DIRECTION ( 'NONE',  ( 0.000000000000000000, 0.3090169943749410120, 0.9510565162951557516 ) ) ;
#29299 = ORIENTED_EDGE ( 'NONE', *, *, #12999, .F. ) ;
#29300 = DIRECTION ( 'NONE',  ( 0.000000000000000000, 0.000000000000000000, -1.000000000000000000 ) ) ;
#29301 = CARTESIAN_POINT ( 'NONE',  ( 0.000000000000000000, 0.000000000000000000, 0.000000000000000000 ) ) ;
#29302 = DIRECTION ( 'NONE',  ( -1.000000000000000000, 0.000000000000000000, -0.000000000000000000 ) ) ;
#29303 = EDGE_CURVE ( 'NONE', #3648, #17321, #41594, .T. ) ;
#29304 = ADVANCED_FACE ( 'NONE', ( #23114 ), #30227, .T. ) ;
#29305 = CARTESIAN_POINT ( 'NONE',  ( 0.000000000000000000, -26.23277895567245821, -4.042438405570103477 ) ) ;
#29306 = DIRECTION ( 'NONE',  ( -0.000000000000000000, -0.000000000000000000, -1.000000000000000000 ) ) ;
#29307 = AXIS2_PLACEMENT_3D ( 'NONE', #25827, #37341, #37097 ) ;
#29308 = VECTOR ( 'NONE', #1879, 1000.000000000000114 ) ;
#29309 = EDGE_LOOP ( 'NONE', ( #8361, #30469, #48342, #4307 ) ) ;
#29310 = ADVANCED_FACE ( 'NONE', ( #15527 ), #11133, .T. ) ;
#29311 = CARTESIAN_POINT ( 'NONE',  ( 11.99999999999999822, 0.000000000000000000, 0.000000000000000000 ) ) ;
#29312 = CIRCLE ( 'NONE', #369, 31.99999999999998934 ) ;
#29313 = DIRECTION ( 'NONE',  ( 0.000000000000000000, 0.000000000000000000, 1.000000000000000000 ) ) ;
#29314 = DIRECTION ( 'NONE',  ( -1.000000000000000000, 0.000000000000000000, 0.000000000000000000 ) ) ;
#29315 = DIRECTION ( 'NONE',  ( -1.000000000000000000, -0.000000000000000000, -0.000000000000000000 ) ) ;
#29316 = AXIS2_PLACEMENT_3D ( 'NONE', #6887, #18383, #48245 ) ;
#29317 = CARTESIAN_POINT ( 'NONE',  ( -10.00000000000000000, 0.000000000000000000, 0.000000000000000000 ) ) ;
#29318 = FACE_OUTER_BOUND ( 'NONE', #43930, .T. ) ;
#29319 = EDGE_CURVE ( 'NONE', #42347, #46621, #7210, .T. ) ;
#29320 = ORIENTED_EDGE ( 'NONE', *, *, #42243, .T. ) ;
#29321 = CARTESIAN_POINT ( 'NONE',  ( 0.000000000000000000, 0.000000000000000000, 0.000000000000000000 ) ) ;
#29322 = CARTESIAN_POINT ( 'NONE',  ( 10.00000000000000000, 22.64427369931212297, -30.00120703465181293 ) ) ;
#29323 = CIRCLE ( 'NONE', #14469, 77.49899999999999523 ) ;
#29324 = CYLINDRICAL_SURFACE ( 'NONE', #27690, 31.99999999999998579 ) ;
#29325 = CARTESIAN_POINT ( 'NONE',  ( 10.00000000000000000, 39.04073710021344112, 15.48615015657596317 ) ) ;
#29326 = ORIENTED_EDGE ( 'NONE', *, *, #18419, .F. ) ;
#29327 = ORIENTED_EDGE ( 'NONE', *, *, #28838, .F. ) ;
#29328 = CIRCLE ( 'NONE', #48085, 16.00000000000000000 ) ;
#29329 = VECTOR ( 'NONE', #12099, 1000.000000000000000 ) ;
#29330 = DIRECTION ( 'NONE',  ( -1.000000000000000000, -0.000000000000000000, 0.000000000000000000 ) ) ;
#29331 = CARTESIAN_POINT ( 'NONE',  ( -10.00000000000000000, 0.000000000000000000, 0.000000000000000000 ) ) ;
#29332 = VERTEX_POINT ( 'NONE', #4031 ) ;
#29333 = CIRCLE ( 'NONE', #28539, 31.99999999999998934 ) ;
#29334 = AXIS2_PLACEMENT_3D ( 'NONE', #32645, #17945, #36079 ) ;
#29335 = DIRECTION ( 'NONE',  ( -1.000000000000000000, 0.000000000000000000, -0.000000000000000000 ) ) ;
#29336 = EDGE_CURVE ( 'NONE', #28487, #12494, #16566, .T. ) ;
#29337 = ORIENTED_EDGE ( 'NONE', *, *, #15897, .F. ) ;
#29338 = AXIS2_PLACEMENT_3D ( 'NONE', #34644, #16070, #23890 ) ;
#29339 = EDGE_CURVE ( 'NONE', #7437, #1027, #29870, .T. ) ;
#29340 = CIRCLE ( 'NONE', #3553, 42.00000000000000000 ) ;
#29341 = ADVANCED_FACE ( 'NONE', ( #19419 ), #41477, .T. ) ;
#29342 = CIRCLE ( 'NONE', #15273, 31.99999999999998934 ) ;
#29343 = DIRECTION ( 'NONE',  ( -1.000000000000000000, -0.000000000000000000, -0.000000000000000000 ) ) ;
#29344 = ORIENTED_EDGE ( 'NONE', *, *, #8610, .F. ) ;
#29345 = EDGE_LOOP ( 'NONE', ( #43893, #15, #6755, #2296 ) ) ;
#29346 = DIRECTION ( 'NONE',  ( 0.000000000000000000, 0.000000000000000000, 1.000000000000000000 ) ) ;
#29347 = EDGE_CURVE ( 'NONE', #10009, #9517, #47075, .T. ) ;
#29348 = ORIENTED_EDGE ( 'NONE', *, *, #5363, .T. ) ;
#29349 = CARTESIAN_POINT ( 'NONE',  ( 0.000000000000000000, -120.0000000000000000, -5.500000000000000000 ) ) ;
#29350 = VECTOR ( 'NONE', #39134, 1000.000000000000227 ) ;
#29351 = CARTESIAN_POINT ( 'NONE',  ( 10.00000000000000000, 0.000000000000000000, 0.000000000000000000 ) ) ;
#29352 = CARTESIAN_POINT ( 'NONE',  ( 0.000000000000000000, 0.000000000000000000, 0.000000000000000000 ) ) ;
#29353 = ORIENTED_EDGE ( 'NONE', *, *, #33535, .F. ) ;
#29354 = VERTEX_POINT ( 'NONE', #25803 ) ;
#29355 = DIRECTION ( 'NONE',  ( -0.000000000000000000, -0.6691306063588671194, 0.7431448254773862505 ) ) ;
#29356 = VECTOR ( 'NONE', #32152, 1000.000000000000000 ) ;
#29357 = CARTESIAN_POINT ( 'NONE',  ( 11.99999999999999822, -80.28980883073769803, 16.65972982744905551 ) ) ;
#29358 = VERTEX_POINT ( 'NONE', #7695 ) ;
#29359 = ADVANCED_FACE ( 'NONE', ( #26056 ), #18935, .F. ) ;
#29360 = CARTESIAN_POINT ( 'NONE',  ( 10.00000000000000000, 0.000000000000000000, 0.000000000000000000 ) ) ;
#29361 = DIRECTION ( 'NONE',  ( -1.000000000000000000, -0.000000000000000000, -0.000000000000000000 ) ) ;
#29362 = ORIENTED_EDGE ( 'NONE', *, *, #15015, .F. ) ;
#29363 = ORIENTED_EDGE ( 'NONE', *, *, #9402, .T. ) ;
#29364 = CARTESIAN_POINT ( 'NONE',  ( 12.00000000000000000, -22.67460108101774452, 6.353146135318220367 ) ) ;
#29365 = CARTESIAN_POINT ( 'NONE',  ( 10.00000000000000000, -75.54627589209955829, 17.28742895386058009 ) ) ;
#29366 = CARTESIAN_POINT ( 'NONE',  ( 19.29194287201271862, -133.5026271600380880, 5.500000000000000000 ) ) ;
#29367 = LINE ( 'NONE', #212, #33783 ) ;
#29368 = LINE ( 'NONE', #47481, #24982 ) ;
#29369 = FACE_OUTER_BOUND ( 'NONE', #19286, .T. ) ;
#29370 = ADVANCED_FACE ( 'NONE', ( #22395 ), #11618, .T. ) ;
#29371 = CARTESIAN_POINT ( 'NONE',  ( 10.00000000000000000, -10.41901085202107247, 40.68715046381925049 ) ) ;
#29372 = DIRECTION ( 'NONE',  ( -1.000000000000000000, 0.000000000000000000, 0.000000000000000000 ) ) ;
#29373 = EDGE_LOOP ( 'NONE', ( #12474, #12007, #8800, #37746 ) ) ;
#29374 = CIRCLE ( 'NONE', #19205, 31.99999999999998934 ) ;
#29375 = DIRECTION ( 'NONE',  ( -1.000000000000000000, 0.000000000000000000, -0.000000000000000000 ) ) ;
#29376 = FACE_OUTER_BOUND ( 'NONE', #29446, .T. ) ;
#29377 = DIRECTION ( 'NONE',  ( 0.000000000000000000, 0.000000000000000000, 1.000000000000000000 ) ) ;
#29378 = AXIS2_PLACEMENT_3D ( 'NONE', #30441, #4729, #19641 ) ;
#29379 = FACE_OUTER_BOUND ( 'NONE', #27671, .T. ) ;
#29380 = VERTEX_POINT ( 'NONE', #15049 ) ;
#29381 = VERTEX_POINT ( 'NONE', #22863 ) ;
#29382 = ORIENTED_EDGE ( 'NONE', *, *, #8449, .F. ) ;
#29383 = ADVANCED_FACE ( 'NONE', ( #42927 ), #20391, .T. ) ;
#29384 = DIRECTION ( 'NONE',  ( 1.000000000000000000, -0.000000000000000000, -0.000000000000000000 ) ) ;
#29385 = SHAPE_REPRESENTATION ( 'Sliding Dog Clutch Collar', ( #11636 ), #10062 ) ;
#29386 = CIRCLE ( 'NONE', #10630, 82.00000000000000000 ) ;
#29387 = VECTOR ( 'NONE', #4518, 1000.000000000000000 ) ;
#29388 = CARTESIAN_POINT ( 'NONE',  ( 5.000000000000002665, -81.50828551894220197, -8.966570791701590437 ) ) ;
#29389 = ORIENTED_EDGE ( 'NONE', *, *, #18523, .T. ) ;
#29390 = EDGE_CURVE ( 'NONE', #26518, #13379, #25951, .T. ) ;
#29391 = AXIS2_PLACEMENT_3D ( 'NONE', #30892, #15701, #34529 ) ;
#29392 = ORIENTED_EDGE ( 'NONE', *, *, #44818, .T. ) ;
#29393 = EDGE_CURVE ( 'NONE', #3571, #44934, #9150, .T. ) ;
#29394 = CYLINDRICAL_SURFACE ( 'NONE', #46138, 77.49899999999999523 ) ;
#29395 = ORIENTED_EDGE ( 'NONE', *, *, #39871, .F. ) ;
#29396 = DIRECTION ( 'NONE',  ( 0.000000000000000000, 0.000000000000000000, 1.000000000000000000 ) ) ;
#29397 = EDGE_LOOP ( 'NONE', ( #9715, #22257, #48122, #48000 ) ) ;
#29398 = ORIENTED_EDGE ( 'NONE', *, *, #20967, .T. ) ;
#29399 = CARTESIAN_POINT ( 'NONE',  ( 35.50000000000000711, -120.0000000000000000, 2.500000000000000000 ) ) ;
#29400 = CIRCLE ( 'NONE', #24720, 77.49899999999999523 ) ;
#29401 = ORIENTED_EDGE ( 'NONE', *, *, #24875, .F. ) ;
#29402 = ADVANCED_FACE ( 'NONE', ( #13073 ), #34846, .F. ) ;
#29403 = VECTOR ( 'NONE', #14415, 1000.000000000000000 ) ;
#29404 = DIRECTION ( 'NONE',  ( -1.000000000000000000, 0.000000000000000000, 0.000000000000000000 ) ) ;
#29405 = EDGE_CURVE ( 'NONE', #10399, #47783, #10348, .T. ) ;
#29406 = VERTEX_POINT ( 'NONE', #38784 ) ;
#29407 = DIRECTION ( 'NONE',  ( -1.000000000000000000, -0.000000000000000000, -0.000000000000000000 ) ) ;
#29408 = ORIENTED_EDGE ( 'NONE', *, *, #47320, .F. ) ;
#29409 = CIRCLE ( 'NONE', #25479, 12.50000000000000000 ) ;
#29410 = DIRECTION ( 'NONE',  ( -1.000000000000000000, 0.000000000000000000, 0.000000000000000000 ) ) ;
#29411 = CARTESIAN_POINT ( 'NONE',  ( 0.000000000000000000, -20.55727247249748046, 16.78983467731285018 ) ) ;
#29412 = ORIENTED_EDGE ( 'NONE', *, *, #12912, .T. ) ;
#29413 = CARTESIAN_POINT ( 'NONE',  ( -3.961125083139900749, -143.2122702051246677, -5.500000000000000000 ) ) ;
#29414 = LINE ( 'NONE', #34035, #18485 ) ;
#29416 = ORIENTED_EDGE ( 'NONE', *, *, #18290, .F. ) ;
#29415 = CARTESIAN_POINT ( 'NONE',  ( 0.000000000000000000, 68.26794271651307611, -31.47745569255064169 ) ) ;
#29417 = CARTESIAN_POINT ( 'NONE',  ( -8.637688417678548447, 13.69818742750669749, -55.00000000000000000 ) ) ;
#29418 = ORIENTED_EDGE ( 'NONE', *, *, #26376, .T. ) ;
#29419 = CARTESIAN_POINT ( 'NONE',  ( 10.00000000000000000, 0.000000000000000000, 0.000000000000000000 ) ) ;
#29420 = ORIENTED_EDGE ( 'NONE', *, *, #38855, .F. ) ;
#29421 = VERTEX_POINT ( 'NONE', #35327 ) ;
#29422 = CARTESIAN_POINT ( 'NONE',  ( 5.000000000000002665, 81.90746397400387480, 3.894527615418187150 ) ) ;
#29423 = CARTESIAN_POINT ( 'NONE',  ( 10.00000000000000000, 5.256550761633969060, -77.32052557432835727 ) ) ;
#29424 = ORIENTED_EDGE ( 'NONE', *, *, #11070, .F. ) ;
#29425 = CARTESIAN_POINT ( 'NONE',  ( 10.00000000000000000, 0.000000000000000000, 0.000000000000000000 ) ) ;
#29426 = CIRCLE ( 'NONE', #13017, 31.99999999999998934 ) ;
#29427 = CARTESIAN_POINT ( 'NONE',  ( -43.60332556124591719, -107.0000000000000000, 102.9091629284897493 ) ) ;
#29428 = DIRECTION ( 'NONE',  ( -1.000000000000000000, -0.000000000000000000, 0.000000000000000000 ) ) ;
#29429 = ORIENTED_EDGE ( 'NONE', *, *, #16227, .T. ) ;
#29430 = AXIS2_PLACEMENT_3D ( 'NONE', #25716, #33555, #22048 ) ;
#29431 = LINE ( 'NONE', #33086, #30453 ) ;
#29432 = PLANE ( 'NONE',  #27480 ) ;
#29433 = CYLINDRICAL_SURFACE ( 'NONE', #10657, 31.99999999999998579 ) ;
#29434 = VERTEX_POINT ( 'NONE', #27515 ) ;
#29435 = CYLINDRICAL_SURFACE ( 'NONE', #17604, 31.99999999999998579 ) ;
#29436 = DIRECTION ( 'NONE',  ( -1.000000000000000000, 0.000000000000000000, 0.000000000000000000 ) ) ;
#29437 = DIRECTION ( 'NONE',  ( -1.000000000000000000, -0.000000000000000000, -0.000000000000000000 ) ) ;
#29438 = DIRECTION ( 'NONE',  ( 0.000000000000000000, 0.4539904997395477482, -0.8910065241883673437 ) ) ;
#29439 = FACE_BOUND ( 'NONE', #46417, .T. ) ;
#29440 = FACE_OUTER_BOUND ( 'NONE', #9836, .T. ) ;
#29441 = CARTESIAN_POINT ( 'NONE',  ( 10.00000000000000000, -6.903761155838323837, 77.19088730480521576 ) ) ;
#29442 = LINE ( 'NONE', #22078, #17842 ) ;
#29443 = ORIENTED_EDGE ( 'NONE', *, *, #46913, .T. ) ;
#29444 = VECTOR ( 'NONE', #6013, 1000.000000000000000 ) ;
#29445 = CARTESIAN_POINT ( 'NONE',  ( 10.00000000000000000, 0.000000000000000000, 0.000000000000000000 ) ) ;
#29446 = EDGE_LOOP ( 'NONE', ( #15538, #6901, #19888, #9499 ) ) ;
#29447 = DIRECTION ( 'NONE',  ( -1.000000000000000000, -0.000000000000000000, 0.000000000000000000 ) ) ;
#29448 = DIRECTION ( 'NONE',  ( 0.000000000000000000, 0.000000000000000000, 1.000000000000000000 ) ) ;
#29449 = CARTESIAN_POINT ( 'NONE',  ( 15.00000000000000000, -22.67460108101774452, 6.353146135318220367 ) ) ;
#29450 = ORIENTED_EDGE ( 'NONE', *, *, #34201, .T. ) ;
#29451 = AXIS2_PLACEMENT_3D ( 'NONE', #29597, #18586, #210 ) ;
#29452 = ADVANCED_FACE ( 'NONE', ( #8901 ), #46349, .T. ) ;
#29453 = DIRECTION ( 'NONE',  ( -1.000000000000000000, 0.000000000000000000, 0.000000000000000000 ) ) ;
#29454 = EDGE_LOOP ( 'NONE', ( #7659, #6344, #46748, #5069 ) ) ;
#29455 = EDGE_CURVE ( 'NONE', #17495, #44907, #16495, .T. ) ;
#29456 = AXIS2_PLACEMENT_3D ( 'NONE', #18284, #14141, #6803 ) ;
#29457 = VECTOR ( 'NONE', #44483, 999.9999999999998863 ) ;
#29458 = LINE ( 'NONE', #13816, #32355 ) ;
#29459 = EDGE_CURVE ( 'NONE', #5623, #23602, #14269, .T. ) ;
#29460 = DIRECTION ( 'NONE',  ( 0.000000000000000000, 0.7604059656000322631, -0.6494480483301821039 ) ) ;
#29461 = DIRECTION ( 'NONE',  ( -0.000000000000000000, -0.000000000000000000, 1.000000000000000000 ) ) ;
#29462 = VERTEX_POINT ( 'NONE', #27766 ) ;
#29463 = CARTESIAN_POINT ( 'NONE',  ( 10.00000000000000000, -73.73191006444582740, 14.66109333815435889 ) ) ;
#29464 = EDGE_CURVE ( 'NONE', #36144, #28409, #5672, .T. ) ;
#29465 = ORIENTED_EDGE ( 'NONE', *, *, #37252, .F. ) ;
#29466 = CARTESIAN_POINT ( 'NONE',  ( -10.00000000000000000, 0.000000000000000000, 0.000000000000000000 ) ) ;
#29467 = DIRECTION ( 'NONE',  ( 0.000000000000000000, 0.000000000000000000, -1.000000000000000000 ) ) ;
#29468 = DIRECTION ( 'NONE',  ( 0.000000000000000000, 0.4539904997395414754, 0.8910065241883706744 ) ) ;
#29470 = CARTESIAN_POINT ( 'NONE',  ( 10.00000000000000000, -60.67117009219176538, 55.16347631943019536 ) ) ;
#29469 = CIRCLE ( 'NONE', #8375, 77.49899999999998101 ) ;
#29471 = EDGE_LOOP ( 'NONE', ( #42837, #24646, #4139, #47827 ) ) ;
#29472 = FACE_OUTER_BOUND ( 'NONE', #39578, .T. ) ;
#29473 = ORIENTED_EDGE ( 'NONE', *, *, #6759, .F. ) ;
#29474 = ORIENTED_EDGE ( 'NONE', *, *, #28235, .F. ) ;
#29475 = DIRECTION ( 'NONE',  ( 0.000000000000000000, -0.2334453638558921240, -0.9723699203976797767 ) ) ;
#29476 = CIRCLE ( 'NONE', #12307, 77.49899999999999523 ) ;
#29477 = DIRECTION ( 'NONE',  ( 0.000000000000000000, 0.000000000000000000, 1.000000000000000000 ) ) ;
#29478 = CARTESIAN_POINT ( 'NONE',  ( 11.99999999999999822, 0.000000000000000000, 0.000000000000000000 ) ) ;
#29479 = FACE_OUTER_BOUND ( 'NONE', #41826, .T. ) ;
#29480 = VERTEX_POINT ( 'NONE', #42439 ) ;
#29481 = CARTESIAN_POINT ( 'NONE',  ( 23.49916127795269460, -121.5130826919798039, 5.500000000000000000 ) ) ;
#29482 = CARTESIAN_POINT ( 'NONE',  ( 10.00000000000000000, 0.000000000000000000, 0.000000000000000000 ) ) ;
#29483 = DIRECTION ( 'NONE',  ( 0.000000000000000000, 0.000000000000000000, 1.000000000000000000 ) ) ;
#29484 = DIRECTION ( 'NONE',  ( 1.000000000000000000, -0.000000000000000000, -0.000000000000000000 ) ) ;
#29485 = DIRECTION ( 'NONE',  ( 0.2306669878475647861, 0.9730327541852491491, 0.000000000000000000 ) ) ;
#29486 = ORIENTED_EDGE ( 'NONE', *, *, #15379, .T. ) ;
#29487 = AXIS2_PLACEMENT_3D ( 'NONE', #43640, #2508, #28475 ) ;
#29488 = DIRECTION ( 'NONE',  ( -1.000000000000000000, -0.000000000000000000, -0.000000000000000000 ) ) ;
#29489 = CARTESIAN_POINT ( 'NONE',  ( 10.00000000000000000, 0.000000000000000000, 0.000000000000000000 ) ) ;
#29490 = CARTESIAN_POINT ( 'NONE',  ( -10.00000000000000000, 0.000000000000000000, 0.000000000000000000 ) ) ;
#29491 = DIRECTION ( 'NONE',  ( 0.000000000000000000, 0.000000000000000000, 1.000000000000000000 ) ) ;
#29492 = LINE ( 'NONE', #43933, #23735 ) ;
#29493 = CARTESIAN_POINT ( 'NONE',  ( -10.00000000000000000, 0.000000000000000000, 0.000000000000000000 ) ) ;
#29494 = CIRCLE ( 'NONE', #24019, 77.49899999999999523 ) ;
#29495 = ADVANCED_FACE ( 'NONE', ( #39248 ), #38529, .T. ) ;
#29496 = LINE ( 'NONE', #22400, #2895 ) ;
#29497 = LINE ( 'NONE', #47603, #18277 ) ;
#29498 = FACE_OUTER_BOUND ( 'NONE', #33217, .T. ) ;
#29499 = DIRECTION ( 'NONE',  ( -1.000000000000000000, 0.000000000000000000, 0.000000000000000000 ) ) ;
#29500 = EDGE_CURVE ( 'NONE', #29885, #13511, #35357, .T. ) ;
#29501 = EDGE_CURVE ( 'NONE', #20927, #33784, #45620, .T. ) ;
#29502 = DIRECTION ( 'NONE',  ( 0.000000000000000000, 0.3090169943749483394, -0.9510565162951534202 ) ) ;
#29503 = ORIENTED_EDGE ( 'NONE', *, *, #25962, .F. ) ;
#29504 = ORIENTED_EDGE ( 'NONE', *, *, #35411, .T. ) ;
#29505 = VECTOR ( 'NONE', #6664, 1000.000000000000000 ) ;
#29506 = VERTEX_POINT ( 'NONE', #4994 ) ;
#29507 = EDGE_LOOP ( 'NONE', ( #38363, #9956, #45956, #4577 ) ) ;
#29508 = AXIS2_PLACEMENT_3D ( 'NONE', #11454, #41784, #8480 ) ;
#29509 = CARTESIAN_POINT ( 'NONE',  ( 10.00000000000000000, -3.925862922256464493, 41.81611651403861174 ) ) ;
#29510 = ADVANCED_FACE ( 'NONE', ( #41972 ), #8421, .T. ) ;
#29511 = VERTEX_POINT ( 'NONE', #16015 ) ;
#29512 = EDGE_CURVE ( 'NONE', #1317, #17390, #30957, .T. ) ;
#29513 = EDGE_CURVE ( 'NONE', #17937, #27340, #42191, .T. ) ;
#29514 = ORIENTED_EDGE ( 'NONE', *, *, #42095, .T. ) ;
#29515 = AXIS2_PLACEMENT_3D ( 'NONE', #14018, #10337, #34292 ) ;
#29516 = FACE_OUTER_BOUND ( 'NONE', #26346, .T. ) ;
#29517 = DIRECTION ( 'NONE',  ( -1.000000000000000000, -0.000000000000000000, 0.000000000000000000 ) ) ;
#29518 = CARTESIAN_POINT ( 'NONE',  ( -7.469491406282094736, 4.756046723998911929, 42.00000000000001421 ) ) ;
#29519 = ORIENTED_EDGE ( 'NONE', *, *, #23063, .T. ) ;
#29520 = FACE_OUTER_BOUND ( 'NONE', #28796, .T. ) ;
#29521 = EDGE_LOOP ( 'NONE', ( #10536, #44334, #39216, #40040 ) ) ;
#29522 = ORIENTED_EDGE ( 'NONE', *, *, #34927, .F. ) ;
#29523 = VERTEX_POINT ( 'NONE', #19910 ) ;
#29524 = DIRECTION ( 'NONE',  ( -1.000000000000000000, 0.000000000000000000, -0.000000000000000000 ) ) ;
#29525 = PRODUCT_DEFINITION ( 'UNKNOWN', '', #17044, #40877 ) ;
#29526 = FACE_OUTER_BOUND ( 'NONE', #41091, .T. ) ;
#29527 = AXIS2_PLACEMENT_3D ( 'NONE', #13482, #24749, #47261 ) ;
#29528 = CARTESIAN_POINT ( 'NONE',  ( -23.54415474984308787, -120.4156646670583086, -5.500000000000000000 ) ) ;
#29529 = ORIENTED_EDGE ( 'NONE', *, *, #38976, .T. ) ;
#29530 = VERTEX_POINT ( 'NONE', #16263 ) ;
#29531 = DIRECTION ( 'NONE',  ( -1.000000000000000000, 0.000000000000000000, 0.000000000000000000 ) ) ;
#29532 = ORIENTED_EDGE ( 'NONE', *, *, #21868, .F. ) ;
#29533 = CARTESIAN_POINT ( 'NONE',  ( 4.999999999999999112, -21.40280677340345505, -36.13751322684441192 ) ) ;
#29534 = DIRECTION ( 'NONE',  ( 1.000000000000000000, 0.000000000000000000, 0.000000000000000000 ) ) ;
#29535 = CARTESIAN_POINT ( 'NONE',  ( 15.00000000000000000, -3.948201729842355068, -23.21447184625292692 ) ) ;
#29536 = DIRECTION ( 'NONE',  ( -1.000000000000000000, -0.000000000000000000, -0.000000000000000000 ) ) ;
#29537 = DIRECTION ( 'NONE',  ( 0.000000000000000000, 0.000000000000000000, -1.000000000000000000 ) ) ;
#29538 = DIRECTION ( 'NONE',  ( -1.000000000000000000, 0.000000000000000000, -0.000000000000000000 ) ) ;
#29539 = DIRECTION ( 'NONE',  ( 0.000000000000000000, -1.000000000000000000, -1.040834085586084257E-14 ) ) ;
#29540 = CARTESIAN_POINT ( 'NONE',  ( 12.50000000000000000, -107.5000000000000000, 40.00000000000000000 ) ) ;
#29541 = LINE ( 'NONE', #48380, #44670 ) ;
#29542 = VECTOR ( 'NONE', #402, 1000.000000000000000 ) ;
#29543 = ORIENTED_EDGE ( 'NONE', *, *, #22102, .F. ) ;
#29544 = CARTESIAN_POINT ( 'NONE',  ( 10.00000000000000000, -30.41916302227164337, 71.27951684758015460 ) ) ;
#29545 = ORIENTED_EDGE ( 'NONE', *, *, #28296, .F. ) ;
#29546 = CIRCLE ( 'NONE', #8435, 31.99999999999999289 ) ;
#29547 = LINE ( 'NONE', #45207, #2702 ) ;
#29548 = DIRECTION ( 'NONE',  ( 1.000000000000000000, 0.000000000000000000, 0.000000000000000000 ) ) ;
#29549 = CARTESIAN_POINT ( 'NONE',  ( 0.000000000000000000, 0.000000000000000000, 0.000000000000000000 ) ) ;
#29550 = VECTOR ( 'NONE', #32941, 1000.000000000000114 ) ;
#29551 = CARTESIAN_POINT ( 'NONE',  ( 0.000000000000000000, -35.91791733033525702, 68.67312586194982771 ) ) ;
#29552 = DIRECTION ( 'NONE',  ( -1.000000000000000000, -0.000000000000000000, 0.000000000000000000 ) ) ;
#29553 = ADVANCED_FACE ( 'NONE', ( #25512 ), #13541, .F. ) ;
#29554 = DIRECTION ( 'NONE',  ( -1.000000000000000000, 0.000000000000000000, 0.000000000000000000 ) ) ;
#29555 = DIRECTION ( 'NONE',  ( 0.000000000000000000, 0.000000000000000000, 1.000000000000000000 ) ) ;
#29556 = EDGE_CURVE ( 'NONE', #34442, #45584, #12726, .T. ) ;
#29557 = DIRECTION ( 'NONE',  ( -1.000000000000000000, 0.000000000000000000, 0.000000000000000000 ) ) ;
#29558 =( LENGTH_UNIT ( ) NAMED_UNIT ( * ) SI_UNIT ( .MILLI., .METRE. ) );
#29559 = EDGE_CURVE ( 'NONE', #8522, #48048, #40091, .T. ) ;
#29560 = FACE_OUTER_BOUND ( 'NONE', #34045, .T. ) ;
#29561 = VERTEX_POINT ( 'NONE', #6207 ) ;
#29562 = EDGE_LOOP ( 'NONE', ( #17057, #23679, #13756, #9591 ) ) ;
#29563 = AXIS2_PLACEMENT_3D ( 'NONE', #19314, #4635, #19538 ) ;
#29564 = ORIENTED_EDGE ( 'NONE', *, *, #25861, .T. ) ;
#29565 = CARTESIAN_POINT ( 'NONE',  ( -3.000000000000000000, -23.29833615347104825, -3.418703333116803744 ) ) ;
#29566 = DIRECTION ( 'NONE',  ( 0.000000000000000000, 0.000000000000000000, 1.000000000000000000 ) ) ;
#29567 = VERTEX_POINT ( 'NONE', #9615 ) ;
#29568 = VERTEX_POINT ( 'NONE', #24566 ) ;
#29569 = ADVANCED_FACE ( 'NONE', ( #10603 ), #6686, .T. ) ;
#29570 = EDGE_CURVE ( 'NONE', #24574, #29827, #39276, .T. ) ;
#29571 = FACE_OUTER_BOUND ( 'NONE', #44322, .T. ) ;
#29572 = CIRCLE ( 'NONE', #30358, 77.49900000000000944 ) ;
#29573 = ORIENTED_EDGE ( 'NONE', *, *, #41782, .T. ) ;
#29574 = VERTEX_POINT ( 'NONE', #36298 ) ;
#29575 = CIRCLE ( 'NONE', #41327, 82.00000000000000000 ) ;
#29576 = EDGE_CURVE ( 'NONE', #21501, #24420, #29917, .T. ) ;
#29577 = DIRECTION ( 'NONE',  ( -0.5200609990133016058, -0.8541291221503261033, 0.000000000000000000 ) ) ;
#29578 = EDGE_LOOP ( 'NONE', ( #17904, #28484, #23185, #6474 ) ) ;
#29579 = LINE ( 'NONE', #32999, #27043 ) ;
#29580 = EDGE_LOOP ( 'NONE', ( #10366, #42361, #7799, #41501 ) ) ;
#29581 = ORIENTED_EDGE ( 'NONE', *, *, #10493, .F. ) ;
#29582 = CARTESIAN_POINT ( 'NONE',  ( 0.000000000000000000, -1.278221433540501550, 26.51162292216071847 ) ) ;
#29583 = CARTESIAN_POINT ( 'NONE',  ( 10.00000000000000000, 26.08949754953062694, -27.05870788708203989 ) ) ;
#29584 = DIRECTION ( 'NONE',  ( 0.000000000000000000, -0.7071067811865389130, -0.7071067811865563435 ) ) ;
#29585 = EDGE_LOOP ( 'NONE', ( #7319, #46969, #28121, #43626 ) ) ;
#29586 = VERTEX_POINT ( 'NONE', #36534 ) ;
#29587 = VECTOR ( 'NONE', #45097, 1000.000000000000000 ) ;
#29588 = CARTESIAN_POINT ( 'NONE',  ( 0.000000000000000000, 0.000000000000000000, 0.000000000000000000 ) ) ;
#29589 = CYLINDRICAL_SURFACE ( 'NONE', #24332, 42.00000000000000000 ) ;
#29590 = ORIENTED_EDGE ( 'NONE', *, *, #21056, .F. ) ;
#29591 = ORIENTED_EDGE ( 'NONE', *, *, #31232, .F. ) ;
#29592 = CARTESIAN_POINT ( 'NONE',  ( 0.000000000000000000, 0.000000000000000000, 0.000000000000000000 ) ) ;
#29593 = CARTESIAN_POINT ( 'NONE',  ( 0.000000000000000000, 0.000000000000000000, 0.000000000000000000 ) ) ;
#29594 = VERTEX_POINT ( 'NONE', #2510 ) ;
#29595 = CARTESIAN_POINT ( 'NONE',  ( 10.00000000000000000, 34.94270380257639630, 74.18225833017902460 ) ) ;
#29596 = PLANE ( 'NONE',  #41004 ) ;
#29597 = CARTESIAN_POINT ( 'NONE',  ( 10.00000000000000000, 0.000000000000000000, 0.000000000000000000 ) ) ;
#29598 = DIRECTION ( 'NONE',  ( 1.000000000000000000, 0.000000000000000000, 0.000000000000000000 ) ) ;
#29599 = CARTESIAN_POINT ( 'NONE',  ( 0.000000000000000000, 17.80606268964540106, 33.00180498840052934 ) ) ;
#29600 = DIRECTION ( 'NONE',  ( 0.7533909544171998318, 0.6575728627325954090, 0.000000000000000000 ) ) ;
#29601 = DIRECTION ( 'NONE',  ( -1.000000000000000000, -0.000000000000000000, -0.000000000000000000 ) ) ;
#29602 = CARTESIAN_POINT ( 'NONE',  ( -12.40464318976454905, 10.41032311384371845, -64.01812422950393966 ) ) ;
#29603 = AXIS2_PLACEMENT_3D ( 'NONE', #726, #15660, #958 ) ;
#29604 = DIRECTION ( 'NONE',  ( -1.000000000000000000, -0.000000000000000000, -0.000000000000000000 ) ) ;
#29606 = EDGE_CURVE ( 'NONE', #44547, #25900, #35816, .T. ) ;
#29605 = CIRCLE ( 'NONE', #12426, 14.09999999999999964 ) ;
#29607 = CARTESIAN_POINT ( 'NONE',  ( 0.000000000000000000, 0.000000000000000000, 0.000000000000000000 ) ) ;
#29608 = CARTESIAN_POINT ( 'NONE',  ( 10.00000000000000000, 0.000000000000000000, 0.000000000000000000 ) ) ;
#29610 = AXIS2_PLACEMENT_3D ( 'NONE', #19167, #48304, #26025 ) ;
#29609 = PRESENTATION_STYLE_ASSIGNMENT (( #48215 ) ) ;
#29611 = DIRECTION ( 'NONE',  ( 0.000000000000000000, 0.000000000000000000, 1.000000000000000000 ) ) ;
#29612 = EDGE_CURVE ( 'NONE', #23424, #5424, #21615, .T. ) ;
#29613 = VERTEX_POINT ( 'NONE', #21358 ) ;
#29615 = EDGE_CURVE ( 'NONE', #2609, #24762, #16973, .T. ) ;
#29614 = UNCERTAINTY_MEASURE_WITH_UNIT (LENGTH_MEASURE( 1.000000000000000082E-05 ), #14152, 'distance_accuracy_value', 'NONE');
#29616 = CYLINDRICAL_SURFACE ( 'NONE', #40116, 31.99999999999999289 ) ;
#29617 = DIRECTION ( 'NONE',  ( 1.000000000000000000, 0.000000000000000000, 0.000000000000000000 ) ) ;
#29618 = VERTEX_POINT ( 'NONE', #31930 ) ;
#29619 = EDGE_CURVE ( 'NONE', #33614, #3193, #25996, .T. ) ;
#29620 = AXIS2_PLACEMENT_3D ( 'NONE', #13733, #28661, #2225 ) ;
#29621 = ADVANCED_FACE ( 'NONE', ( #2995 ), #9870, .T. ) ;
#29622 = CARTESIAN_POINT ( 'NONE',  ( 50.00005079999999680, 0.000000000000000000, 21.00000000000000000 ) ) ;
#29623 = CARTESIAN_POINT ( 'NONE',  ( 5.000000000000000000, 27.75498641678742473, 31.52238457039609187 ) ) ;
#29624 = ORIENTED_EDGE ( 'NONE', *, *, #18937, .F. ) ;
#29625 = ORIENTED_EDGE ( 'NONE', *, *, #41282, .T. ) ;
#29626 = ORIENTED_EDGE ( 'NONE', *, *, #42394, .F. ) ;
#29627 = ORIENTED_EDGE ( 'NONE', *, *, #23342, .F. ) ;
#29628 = CARTESIAN_POINT ( 'NONE',  ( 25.81725066941077529, -113.8380548628854854, 5.500000000000000000 ) ) ;
#29629 = EDGE_CURVE ( 'NONE', #7892, #46255, #24804, .T. ) ;
#29630 = AXIS2_PLACEMENT_3D ( 'NONE', #11062, #18407, #48264 ) ;
#29631 = DIRECTION ( 'NONE',  ( -1.000000000000000000, 0.000000000000000000, 0.000000000000000000 ) ) ;
#29633 = ORIENTED_EDGE ( 'NONE', *, *, #7397, .T. ) ;
#29632 = AXIS2_PLACEMENT_3D ( 'NONE', #1410, #38618, #8986 ) ;
#29634 = ORIENTED_EDGE ( 'NONE', *, *, #14032, .F. ) ;
#29635 = CARTESIAN_POINT ( 'NONE',  ( -12.49999999999999645, 0.000000000000000000, 42.00000000000001421 ) ) ;
#29636 = VERTEX_POINT ( 'NONE', #39746 ) ;
#29637 = CIRCLE ( 'NONE', #25710, 37.49900000000000233 ) ;
#29638 = LINE ( 'NONE', #28909, #5108 ) ;
#29639 = CYLINDRICAL_SURFACE ( 'NONE', #25930, 37.49900000000000233 ) ;
#29640 = ORIENTED_EDGE ( 'NONE', *, *, #9005, .T. ) ;
#29641 = DIRECTION ( 'NONE',  ( -1.000000000000000000, 0.000000000000000000, 0.000000000000000000 ) ) ;
#29642 = DIRECTION ( 'NONE',  ( -1.000000000000000000, 0.000000000000000000, 0.000000000000000000 ) ) ;
#29643 = EDGE_LOOP ( 'NONE', ( #41615, #31491, #22053, #9058 ) ) ;
#29644 = ADVANCED_FACE ( 'NONE', ( #6920 ), #35579, .F. ) ;
#29645 = DIRECTION ( 'NONE',  ( 1.000000000000000000, 0.000000000000000000, 0.000000000000000000 ) ) ;
#29646 = CARTESIAN_POINT ( 'NONE',  ( 0.000000000000000000, -89.50000000000000000, -5.500000000000000000 ) ) ;
#29647 = ORIENTED_EDGE ( 'NONE', *, *, #22877, .F. ) ;
#29648 = DIRECTION ( 'NONE',  ( -0.000000000000000000, -0.000000000000000000, -1.000000000000000000 ) ) ;
#29649 = ORIENTED_EDGE ( 'NONE', *, *, #14519, .T. ) ;
#29650 = VECTOR ( 'NONE', #23326, 1000.000000000000000 ) ;
#29651 = ORIENTED_EDGE ( 'NONE', *, *, #42267, .T. ) ;
#29652 = CARTESIAN_POINT ( 'NONE',  ( 10.00000000000000000, -65.59268652807183742, -36.72794159290312166 ) ) ;
#29653 = DIRECTION ( 'NONE',  ( -1.000000000000000000, -0.000000000000000000, 0.000000000000000000 ) ) ;
#29654 = ORIENTED_EDGE ( 'NONE', *, *, #12711, .T. ) ;
#29655 = LINE ( 'NONE', #17907, #43305 ) ;
#29656 = CARTESIAN_POINT ( 'NONE',  ( 0.000000000000000000, 0.000000000000000000, -44.99999999999998579 ) ) ;
#29657 = DIRECTION ( 'NONE',  ( 0.000000000000000000, 0.000000000000000000, 1.000000000000000000 ) ) ;
#29658 = PRODUCT_DEFINITION_SHAPE ( 'NONE', 'NONE',  #48454 ) ;
#29659 = DIRECTION ( 'NONE',  ( -1.000000000000000000, 0.000000000000000000, 0.000000000000000000 ) ) ;
#29660 = DIRECTION ( 'NONE',  ( 0.9038112904824853189, -0.4279312458752977388, 0.000000000000000000 ) ) ;
#29661 = CARTESIAN_POINT ( 'NONE',  ( 12.00000000000000355, 0.000000000000000000, 0.000000000000000000 ) ) ;
#29662 = CYLINDRICAL_SURFACE ( 'NONE', #10637, 37.49900000000000233 ) ;
#29663 = DIRECTION ( 'NONE',  ( 0.02332147558787671729, 0.9997280174009349762, -0.000000000000000000 ) ) ;
#29664 = DIRECTION ( 'NONE',  ( 0.000000000000000000, 0.000000000000000000, 1.000000000000000000 ) ) ;
#29665 = CYLINDRICAL_SURFACE ( 'NONE', #46620, 82.00000000000000000 ) ;
#29666 = EDGE_CURVE ( 'NONE', #12928, #12661, #17695, .T. ) ;
#29667 = ADVANCED_FACE ( 'NONE', ( #14020 ), #17920, .T. ) ;
#29668 = DIRECTION ( 'NONE',  ( 1.000000000000000000, 0.000000000000000000, 0.000000000000000000 ) ) ;
#29669 = DIRECTION ( 'NONE',  ( -1.000000000000000000, 0.000000000000000000, -0.000000000000000000 ) ) ;
#29670 = CARTESIAN_POINT ( 'NONE',  ( 2.874421927457452952, -143.3717286177755739, 2.500000000000000000 ) ) ;
#29671 = DIRECTION ( 'NONE',  ( -0.000000000000000000, -0.000000000000000000, -1.000000000000000000 ) ) ;
#29672 = EDGE_CURVE ( 'NONE', #21021, #21809, #3727, .T. ) ;
#29673 = ORIENTED_EDGE ( 'NONE', *, *, #2168, .T. ) ;
#29674 = ORIENTED_EDGE ( 'NONE', *, *, #3465, .T. ) ;
#29675 = EDGE_LOOP ( 'NONE', ( #26112, #44209 ) ) ;
#29676 = AXIS2_PLACEMENT_3D ( 'NONE', #26970, #4682, #19836 ) ;
#29677 = CARTESIAN_POINT ( 'NONE',  ( 0.000000000000000000, -73.95703589263958122, -23.16143007188505010 ) ) ;
#29678 = AXIS2_PLACEMENT_3D ( 'NONE', #21445, #14105, #43957 ) ;
#29679 = ORIENTED_EDGE ( 'NONE', *, *, #45523, .T. ) ;
#29680 = EDGE_CURVE ( 'NONE', #25106, #12844, #22572, .T. ) ;
#29681 = CARTESIAN_POINT ( 'NONE',  ( 11.99999999999999822, -62.20884554313985149, -46.21855187248698371 ) ) ;
#29682 = CIRCLE ( 'NONE', #35933, 37.49900000000000233 ) ;
#29683 = DIRECTION ( 'NONE',  ( 0.000000000000000000, 0.000000000000000000, 0.9999999999999998890 ) ) ;
#29684 = LINE ( 'NONE', #47553, #38540 ) ;
#29685 = VERTEX_POINT ( 'NONE', #48273 ) ;
#29686 = CIRCLE ( 'NONE', #25798, 16.00000000000000000 ) ;
#29687 = DIRECTION ( 'NONE',  ( -1.000000000000000000, -0.000000000000000000, 0.000000000000000000 ) ) ;
#29688 = VERTEX_POINT ( 'NONE', #15475 ) ;
#29689 = EDGE_CURVE ( 'NONE', #28447, #1914, #21304, .T. ) ;
#29690 = CARTESIAN_POINT ( 'NONE',  ( 10.00000000000000000, 0.000000000000000000, 0.000000000000000000 ) ) ;
#29691 = DIRECTION ( 'NONE',  ( -1.000000000000000000, 0.000000000000000000, -0.000000000000000000 ) ) ;
#29692 = DIRECTION ( 'NONE',  ( -1.000000000000000000, 0.000000000000000000, 0.000000000000000000 ) ) ;
#29693 = ORIENTED_EDGE ( 'NONE', *, *, #42213, .T. ) ;
#29694 = CARTESIAN_POINT ( 'NONE',  ( 11.99999999999999822, -72.35432306680498016, 20.40083707022857951 ) ) ;
#29695 = ORIENTED_EDGE ( 'NONE', *, *, #2575, .T. ) ;
#29696 = DIRECTION ( 'NONE',  ( 0.000000000000000000, 0.2334453638559060296, -0.9723699203976764460 ) ) ;
#29697 = CARTESIAN_POINT ( 'NONE',  ( 0.000000000000000000, -41.76106447765533147, 62.50884508063410294 ) ) ;
#29698 = LINE ( 'NONE', #44636, #9507 ) ;
#29699 = VECTOR ( 'NONE', #18088, 1000.000000000000000 ) ;
#29700 = EDGE_CURVE ( 'NONE', #36027, #24462, #44757, .T. ) ;
#29701 = DIRECTION ( 'NONE',  ( -1.000000000000000000, 0.000000000000000000, -0.000000000000000000 ) ) ;
#29702 = ORIENTED_EDGE ( 'NONE', *, *, #25751, .F. ) ;
#29703 = VECTOR ( 'NONE', #36555, 1000.000000000000114 ) ;
#29704 = DIRECTION ( 'NONE',  ( 0.000000000000000000, 0.000000000000000000, 1.000000000000000000 ) ) ;
#29705 = VERTEX_POINT ( 'NONE', #11799 ) ;
#29706 = ORIENTED_EDGE ( 'NONE', *, *, #27561, .F. ) ;
#29707 = DIRECTION ( 'NONE',  ( 0.000000000000000000, 0.000000000000000000, 1.000000000000000000 ) ) ;
#29708 = AXIS2_PLACEMENT_3D ( 'NONE', #27413, #21017, #9764 ) ;
#29709 = FACE_OUTER_BOUND ( 'NONE', #17988, .T. ) ;
#29710 = CARTESIAN_POINT ( 'NONE',  ( 0.000000000000000000, 26.02418014898310261, 70.52718814184268581 ) ) ;
#29711 = CARTESIAN_POINT ( 'NONE',  ( 11.99999999999999822, -63.18004540532995605, -44.88180994100445531 ) ) ;
#29712 = ORIENTED_EDGE ( 'NONE', *, *, #37162, .T. ) ;
#29713 = CARTESIAN_POINT ( 'NONE',  ( 11.99999999999999822, -28.89263327155796190, 71.91182617369179297 ) ) ;
#29714 = CYLINDRICAL_SURFACE ( 'NONE', #9577, 16.00000000000000000 ) ;
#29715 = CIRCLE ( 'NONE', #10183, 31.99999999999998579 ) ;
#29716 = VERTEX_POINT ( 'NONE', #33347 ) ;
#29717 = CYLINDRICAL_SURFACE ( 'NONE', #19588, 82.00000000000000000 ) ;
#29718 = PLANE ( 'NONE',  #36896 ) ;
#29719 = LINE ( 'NONE', #44416, #17624 ) ;
#29720 = AXIS2_PLACEMENT_3D ( 'NONE', #5395, #1726, #31602 ) ;
#29721 = DIRECTION ( 'NONE',  ( -1.000000000000000000, 0.000000000000000000, -0.000000000000000000 ) ) ;
#29722 = FACE_OUTER_BOUND ( 'NONE', #13494, .T. ) ;
#29723 = DIRECTION ( 'NONE',  ( -1.000000000000000000, -0.000000000000000000, -0.000000000000000000 ) ) ;
#29724 = EDGE_CURVE ( 'NONE', #35358, #10091, #34062, .T. ) ;
#29725 = CARTESIAN_POINT ( 'NONE',  ( 0.000000000000000000, 0.000000000000000000, 0.000000000000000000 ) ) ;
#29726 = DIRECTION ( 'NONE',  ( -1.000000000000000000, -0.000000000000000000, -0.000000000000000000 ) ) ;
#29727 = EDGE_CURVE ( 'NONE', #30166, #38428, #15244, .T. ) ;
#29728 = DIRECTION ( 'NONE',  ( 0.000000000000000000, 0.000000000000000000, 1.000000000000000000 ) ) ;
#29729 = ORIENTED_EDGE ( 'NONE', *, *, #4919, .T. ) ;
#29730 = LINE ( 'NONE', #44663, #33409 ) ;
#29731 = DIRECTION ( 'NONE',  ( -0.000000000000000000, -0.000000000000000000, -1.000000000000000000 ) ) ;
#29732 = CARTESIAN_POINT ( 'NONE',  ( 11.99999999999999822, 0.000000000000000000, 0.000000000000000000 ) ) ;
#29733 = EDGE_CURVE ( 'NONE', #13936, #42659, #22811, .T. ) ;
#29734 = CARTESIAN_POINT ( 'NONE',  ( 11.99999999999999822, -36.72794159290288718, 65.59268652807197952 ) ) ;
#29735 = EDGE_CURVE ( 'NONE', #6127, #13396, #36164, .T. ) ;
#29736 = CARTESIAN_POINT ( 'NONE',  ( 0.000000000000000000, 0.000000000000000000, 0.000000000000000000 ) ) ;
#29737 = ORIENTED_EDGE ( 'NONE', *, *, #20476, .T. ) ;
#29738 = ORIENTED_EDGE ( 'NONE', *, *, #35532, .F. ) ;
#29739 = CIRCLE ( 'NONE', #32840, 42.00000000000000000 ) ;
#29740 = ORIENTED_EDGE ( 'NONE', *, *, #21864, .F. ) ;
#29741 = CIRCLE ( 'NONE', #17986, 31.99999999999998224 ) ;
#29742 = EDGE_LOOP ( 'NONE', ( #30859, #14896, #28564, #40430 ) ) ;
#29743 = CIRCLE ( 'NONE', #30524, 31.99999999999998579 ) ;
#29744 = CONICAL_SURFACE ( 'NONE', #33649, 12.85999999999999943, 0.7853981633974482790 ) ;
#29745 = CARTESIAN_POINT ( 'NONE',  ( 5.000000000000002665, -79.10210256391383155, 21.60688246758557796 ) ) ;
#29746 = VERTEX_POINT ( 'NONE', #26729 ) ;
#29747 = AXIS2_PLACEMENT_3D ( 'NONE', #4906, #4670, #34274 ) ;
#29748 = CIRCLE ( 'NONE', #42266, 31.99999999999999289 ) ;
#29749 = DIRECTION ( 'NONE',  ( 1.000000000000000000, -0.000000000000000000, 0.000000000000000000 ) ) ;
#29750 = AXIS2_PLACEMENT_3D ( 'NONE', #16849, #6076, #34703 ) ;
#29751 = FACE_OUTER_BOUND ( 'NONE', #44799, .T. ) ;
#29752 = CARTESIAN_POINT ( 'NONE',  ( 10.00000000000000000, -24.73286445877653961, -73.44644590900085745 ) ) ;
#29753 = ORIENTED_EDGE ( 'NONE', *, *, #34973, .T. ) ;
#29754 = CYLINDRICAL_SURFACE ( 'NONE', #39113, 12.50000000000000000 ) ;
#29755 = EDGE_LOOP ( 'NONE', ( #10677, #20551, #36960, #45804 ) ) ;
#29756 = ORIENTED_EDGE ( 'NONE', *, *, #42827, .T. ) ;
#29757 = LINE ( 'NONE', #11166, #31166 ) ;
#29758 = DIRECTION ( 'NONE',  ( -1.000000000000000000, 0.000000000000000000, 0.000000000000000000 ) ) ;
#29759 = DIRECTION ( 'NONE',  ( 0.000000000000000000, 0.000000000000000000, 1.000000000000000000 ) ) ;
#29760 = ORIENTED_EDGE ( 'NONE', *, *, #555, .F. ) ;
#29761 = EDGE_LOOP ( 'NONE', ( #3168, #14349, #1032, #45512 ) ) ;
#29762 = DIRECTION ( 'NONE',  ( 0.000000000000000000, 0.000000000000000000, 1.000000000000000000 ) ) ;
#29763 = ORIENTED_EDGE ( 'NONE', *, *, #10436, .F. ) ;
#29764 = CYLINDRICAL_SURFACE ( 'NONE', #47312, 37.49900000000000233 ) ;
#29765 = EDGE_CURVE ( 'NONE', #1817, #4301, #30688, .T. ) ;
#29766 = CYLINDRICAL_SURFACE ( 'NONE', #27231, 37.49900000000000233 ) ;
#29767 = CARTESIAN_POINT ( 'NONE',  ( 12.00000000000000000, -13.04903810567646971, 19.60159698893442481 ) ) ;
#29768 = CARTESIAN_POINT ( 'NONE',  ( -6.719258119307965238, -15.35072898742050107, -1.199999999999999956 ) ) ;
#29769 = CYLINDRICAL_SURFACE ( 'NONE', #22751, 15.77977592589476608 ) ;
#29770 = DIRECTION ( 'NONE',  ( 0.000000000000000000, 0.000000000000000000, 1.000000000000000000 ) ) ;
#29771 = ADVANCED_FACE ( 'NONE', ( #36764 ), #48031, .T. ) ;
#29772 = DIRECTION ( 'NONE',  ( -0.000000000000000000, -0.000000000000000000, 1.000000000000000000 ) ) ;
#29773 = CARTESIAN_POINT ( 'NONE',  ( 10.00000000000000000, 0.000000000000000000, 0.000000000000000000 ) ) ;
#29774 = ORIENTED_EDGE ( 'NONE', *, *, #26393, .T. ) ;
#29775 = AXIS2_PLACEMENT_3D ( 'NONE', #41705, #27760, #12816 ) ;
#29776 = DIRECTION ( 'NONE',  ( -1.000000000000000000, 0.000000000000000000, -0.000000000000000000 ) ) ;
#29777 = ORIENTED_EDGE ( 'NONE', *, *, #33435, .F. ) ;
#29778 = AXIS2_PLACEMENT_3D ( 'NONE', #35896, #35169, #32241 ) ;
#29779 = LINE ( 'NONE', #36405, #10855 ) ;
#29780 = VECTOR ( 'NONE', #25245, 1000.000000000000114 ) ;
#29781 = VECTOR ( 'NONE', #20797, 1000.000000000000000 ) ;
#29782 = DIRECTION ( 'NONE',  ( 0.000000000000000000, 0.000000000000000000, 1.000000000000000000 ) ) ;
#29783 = CARTESIAN_POINT ( 'NONE',  ( 0.000000000000000000, 0.000000000000000000, -105.0000000000000000 ) ) ;
#29784 = DIRECTION ( 'NONE',  ( 0.000000000000000000, 0.8910065241883657894, 0.4539904997395509678 ) ) ;
#29785 = ADVANCED_FACE ( 'NONE', ( #29439, #25991 ), #30172, .F. ) ;
#29786 = VECTOR ( 'NONE', #8760, 1000.000000000000000 ) ;
#29787 = EDGE_CURVE ( 'NONE', #35244, #29480, #37739, .T. ) ;
#29788 = EDGE_CURVE ( 'NONE', #37954, #6365, #22081, .T. ) ;
#29789 = PLANE ( 'NONE',  #7994 ) ;
#29790 = AXIS2_PLACEMENT_3D ( 'NONE', #38453, #24486, #25434 ) ;
#29791 = CARTESIAN_POINT ( 'NONE',  ( 5.000000000000000000, -46.11716303203136391, -67.80270845531939017 ) ) ;
#29792 = CARTESIAN_POINT ( 'NONE',  ( 0.000000000000000000, 33.79645857604513992, -16.45098606841138178 ) ) ;
#29793 = CIRCLE ( 'NONE', #37581, 82.00000000000000000 ) ;
#29794 = CARTESIAN_POINT ( 'NONE',  ( -10.43921258969510824, -98.89258801967538659, 5.500000000000000000 ) ) ;
#29795 = DIRECTION ( 'NONE',  ( -1.000000000000000000, -0.000000000000000000, 0.000000000000000000 ) ) ;
#29796 = EDGE_CURVE ( 'NONE', #9950, #9128, #22340, .T. ) ;
#29797 = LINE ( 'NONE', #48395, #17467 ) ;
#29798 = ORIENTED_EDGE ( 'NONE', *, *, #7746, .F. ) ;
#29799 = ORIENTED_EDGE ( 'NONE', *, *, #41027, .F. ) ;
#29800 = DIRECTION ( 'NONE',  ( -1.000000000000000000, 0.000000000000000000, -0.000000000000000000 ) ) ;
#29801 = DIRECTION ( 'NONE',  ( 1.000000000000000000, -0.000000000000000000, -0.000000000000000000 ) ) ;
#29802 = ORIENTED_EDGE ( 'NONE', *, *, #12643, .F. ) ;
#29803 = VECTOR ( 'NONE', #47537, 1000.000000000000114 ) ;
#29804 = AXIS2_PLACEMENT_3D ( 'NONE', #18970, #3818, #41509 ) ;
#29805 = DIRECTION ( 'NONE',  ( -1.000000000000000000, -0.000000000000000000, 0.000000000000000000 ) ) ;
#29806 = AXIS2_PLACEMENT_3D ( 'NONE', #39667, #25176, #39889 ) ;
#29807 = CIRCLE ( 'NONE', #8705, 37.49900000000000944 ) ;
#29808 = ORIENTED_EDGE ( 'NONE', *, *, #32337, .F. ) ;
#29809 = VERTEX_POINT ( 'NONE', #29911 ) ;
#29810 = AXIS2_PLACEMENT_3D ( 'NONE', #28100, #10208, #5587 ) ;
#29811 = CARTESIAN_POINT ( 'NONE',  ( 19.29194287201271862, -133.5026271600380880, 5.500000000000000000 ) ) ;
#29812 = ORIENTED_EDGE ( 'NONE', *, *, #40514, .F. ) ;
#29813 = DIRECTION ( 'NONE',  ( 0.000000000000000000, 0.000000000000000000, 1.000000000000000000 ) ) ;
#29814 = ADVANCED_FACE ( 'NONE', ( #7645 ), #37261, .F. ) ;
#29815 = ORIENTED_EDGE ( 'NONE', *, *, #33746, .F. ) ;
#29816 = CARTESIAN_POINT ( 'NONE',  ( 10.00000000000000000, 35.47612816024556537, -22.48208911017461631 ) ) ;
#29817 = CIRCLE ( 'NONE', #3933, 16.00000000000000000 ) ;
#29818 = ORIENTED_EDGE ( 'NONE', *, *, #21320, .F. ) ;
#29819 = ORIENTED_EDGE ( 'NONE', *, *, #5142, .T. ) ;
#29820 = CARTESIAN_POINT ( 'NONE',  ( 11.99999999999999822, -27.74655509720725277, 77.16300072079650363 ) ) ;
#29821 = AXIS2_PLACEMENT_3D ( 'NONE', #27185, #8560, #11767 ) ;
#29822 = ADVANCED_FACE ( 'NONE', ( #37499 ), #41418, .T. ) ;
#29823 = CARTESIAN_POINT ( 'NONE',  ( 10.00000000000000000, 26.79245525562761188, -32.34446384429941901 ) ) ;
#29824 = CARTESIAN_POINT ( 'NONE',  ( 0.000000000000000000, -3.925862922256468046, 41.81611651403860463 ) ) ;
#29825 = ADVANCED_FACE ( 'NONE', ( #7875 ), #30641, .T. ) ;
#29826 = ORIENTED_EDGE ( 'NONE', *, *, #12479, .T. ) ;
#29827 = VERTEX_POINT ( 'NONE', #30897 ) ;
#29828 = CARTESIAN_POINT ( 'NONE',  ( 11.99999999999999822, 0.000000000000000000, 0.000000000000000000 ) ) ;
#29829 = EDGE_LOOP ( 'NONE', ( #26095, #3040, #41751, #37724 ) ) ;
#29830 = ORIENTED_EDGE ( 'NONE', *, *, #29390, .T. ) ;
#29831 = DIRECTION ( 'NONE',  ( -1.000000000000000000, 0.000000000000000000, -0.000000000000000000 ) ) ;
#29832 = EDGE_CURVE ( 'NONE', #4650, #30765, #42457, .T. ) ;
#29833 = ORIENTED_EDGE ( 'NONE', *, *, #41314, .F. ) ;
#29834 = CARTESIAN_POINT ( 'NONE',  ( 0.000000000000000000, -33.17418723428319538, 17.67226234102814431 ) ) ;
#29835 = DIRECTION ( 'NONE',  ( -1.000000000000000000, 0.000000000000000000, 0.000000000000000000 ) ) ;
#29836 = CYLINDRICAL_SURFACE ( 'NONE', #524, 31.99999999999998579 ) ;
#29837 = LINE ( 'NONE', #22264, #31593 ) ;
#29838 = DIRECTION ( 'NONE',  ( -0.000000000000000000, -0.000000000000000000, -1.000000000000000000 ) ) ;
#29839 = DIRECTION ( 'NONE',  ( 0.000000000000000000, 0.2334453638558991184, 0.9723699203976781114 ) ) ;
#29840 = ADVANCED_FACE ( 'NONE', ( #12762 ), #35270, .F. ) ;
#29841 = ADVANCED_FACE ( 'NONE', ( #12526 ), #38228, .T. ) ;
#29843 = AXIS2_PLACEMENT_3D ( 'NONE', #29783, #30286, #37377 ) ;
#29842 = CARTESIAN_POINT ( 'NONE',  ( 22.08297821871651934, -111.8242998470044540, 5.500000000000000000 ) ) ;
#29844 = VECTOR ( 'NONE', #1780, 1000.000000000000000 ) ;
#29845 = CARTESIAN_POINT ( 'NONE',  ( 5.000000000000002665, -10.30890764327323872, -81.34940948281348483 ) ) ;
#29846 = FACE_OUTER_BOUND ( 'NONE', #2432, .T. ) ;
#29847 = VERTEX_POINT ( 'NONE', #34296 ) ;
#29848 = AXIS2_PLACEMENT_3D ( 'NONE', #44452, #22180, #29759 ) ;
#29849 = DIRECTION ( 'NONE',  ( -1.000000000000000000, -0.000000000000000000, 0.000000000000000000 ) ) ;
#29850 = CARTESIAN_POINT ( 'NONE',  ( 10.00000000000000000, -39.78640506895653317, 66.50666863321987421 ) ) ;
#29851 = VECTOR ( 'NONE', #27034, 1000.000000000000000 ) ;
#29852 = CYLINDRICAL_SURFACE ( 'NONE', #12314, 31.99999999999999289 ) ;
#29853 = CIRCLE ( 'NONE', #47048, 31.99999999999999289 ) ;
#29854 = ORIENTED_EDGE ( 'NONE', *, *, #33498, .T. ) ;
#29855 = EDGE_CURVE ( 'NONE', #47761, #21860, #13019, .T. ) ;
#29856 = ORIENTED_EDGE ( 'NONE', *, *, #24973, .F. ) ;
#29857 = CARTESIAN_POINT ( 'NONE',  ( 10.00000000000000000, 0.000000000000000000, 0.000000000000000000 ) ) ;
#29858 = AXIS2_PLACEMENT_3D ( 'NONE', #21029, #10504, #36674 ) ;
#29859 = DIRECTION ( 'NONE',  ( -1.000000000000000000, 0.000000000000000000, -0.000000000000000000 ) ) ;
#29860 = CARTESIAN_POINT ( 'NONE',  ( 11.99999999999999822, 0.000000000000000000, 0.000000000000000000 ) ) ;
#29861 = ORIENTED_EDGE ( 'NONE', *, *, #46054, .F. ) ;
#29862 = ORIENTED_EDGE ( 'NONE', *, *, #32110, .F. ) ;
#29863 = FACE_OUTER_BOUND ( 'NONE', #16526, .T. ) ;
#29864 = CIRCLE ( 'NONE', #16599, 37.49900000000000233 ) ;
#29865 = ORIENTED_EDGE ( 'NONE', *, *, #15737, .F. ) ;
#29866 = VERTEX_POINT ( 'NONE', #31383 ) ;
#29867 = ORIENTED_EDGE ( 'NONE', *, *, #5321, .T. ) ;
#29868 = ORIENTED_EDGE ( 'NONE', *, *, #30359, .T. ) ;
#29869 = DIRECTION ( 'NONE',  ( 0.000000000000000000, 0.000000000000000000, 1.000000000000000000 ) ) ;
#29870 = CIRCLE ( 'NONE', #43927, 42.00000000000000000 ) ;
#29871 = CYLINDRICAL_SURFACE ( 'NONE', #37572, 31.99999999999999289 ) ;
#29872 = VERTEX_POINT ( 'NONE', #16431 ) ;
#29873 = ORIENTED_EDGE ( 'NONE', *, *, #8569, .T. ) ;
#29874 = CARTESIAN_POINT ( 'NONE',  ( 10.00000000000000000, 0.000000000000000000, 0.000000000000000000 ) ) ;
#29875 = ORIENTED_EDGE ( 'NONE', *, *, #41931, .F. ) ;
#29876 = ADVANCED_FACE ( 'NONE', ( #31137 ), #27699, .F. ) ;
#29877 = DIRECTION ( 'NONE',  ( -1.000000000000000000, 0.000000000000000000, 0.000000000000000000 ) ) ;
#29878 = DIRECTION ( 'NONE',  ( -1.000000000000000000, -0.000000000000000000, 0.000000000000000000 ) ) ;
#29879 = ORIENTED_EDGE ( 'NONE', *, *, #32647, .F. ) ;
#29880 = ADVANCED_FACE ( 'NONE', ( #4465 ), #1748, .T. ) ;
#29881 = CIRCLE ( 'NONE', #7241, 31.99999999999998934 ) ;
#29882 = VERTEX_POINT ( 'NONE', #26983 ) ;
#29883 = DIRECTION ( 'NONE',  ( -1.000000000000000000, 0.000000000000000000, 0.000000000000000000 ) ) ;
#29884 = CYLINDRICAL_SURFACE ( 'NONE', #23175, 77.49899999999999523 ) ;
#29885 = VERTEX_POINT ( 'NONE', #27219 ) ;
#29887 = VERTEX_POINT ( 'NONE', #38465 ) ;
#29886 = CARTESIAN_POINT ( 'NONE',  ( 11.99999999999999822, 27.74655509720670210, 77.16300072079670258 ) ) ;
#29888 = CARTESIAN_POINT ( 'NONE',  ( 0.000000000000000000, 5.202137450156907761, -37.22597642581151689 ) ) ;
#29889 = ORIENTED_EDGE ( 'NONE', *, *, #4240, .F. ) ;
#29890 = DIRECTION ( 'NONE',  ( -1.000000000000000000, -0.000000000000000000, 0.000000000000000000 ) ) ;
#29891 = EDGE_LOOP ( 'NONE', ( #7198, #5030, #46792, #34851 ) ) ;
#29892 = ORIENTED_EDGE ( 'NONE', *, *, #35603, .T. ) ;
#29893 = DIRECTION ( 'NONE',  ( -1.000000000000000000, 0.000000000000000000, -0.000000000000000000 ) ) ;
#29894 = PLANE ( 'NONE',  #21479 ) ;
#29895 = VECTOR ( 'NONE', #11927, 1000.000000000000000 ) ;
#29896 = CARTESIAN_POINT ( 'NONE',  ( 0.000000000000000000, -27.05870788708213226, -26.08949754953053102 ) ) ;
#29897 = LINE ( 'NONE', #19359, #20383 ) ;
#29898 = CARTESIAN_POINT ( 'NONE',  ( 10.00000000000000000, -21.32104025579135964, 30.84782396557210760 ) ) ;
#29899 = DIRECTION ( 'NONE',  ( 0.000000000000000000, 0.000000000000000000, -1.000000000000000000 ) ) ;
#29900 = EDGE_CURVE ( 'NONE', #31057, #2616, #11195, .T. ) ;
#29901 = DIRECTION ( 'NONE',  ( -1.000000000000000000, 0.000000000000000000, 0.000000000000000000 ) ) ;
#29902 = EDGE_CURVE ( 'NONE', #32940, #18691, #30720, .T. ) ;
#29903 = DIRECTION ( 'NONE',  ( -1.000000000000000000, 0.000000000000000000, 0.000000000000000000 ) ) ;
#29904 = VERTEX_POINT ( 'NONE', #19597 ) ;
#29905 = CARTESIAN_POINT ( 'NONE',  ( 0.000000000000000000, -37.01155633439053361, -6.555932627142825986 ) ) ;
#29906 = ADVANCED_FACE ( 'NONE', ( #37990 ), #1006, .T. ) ;
#29907 = CARTESIAN_POINT ( 'NONE',  ( -3.000000000000000000, -20.55727247249748046, 16.78983467731285018 ) ) ;
#29908 = DIRECTION ( 'NONE',  ( -1.000000000000000000, -0.000000000000000000, -0.000000000000000000 ) ) ;
#29909 = CARTESIAN_POINT ( 'NONE',  ( -14.09999999999999964, 1.726751986797767995E-15, -1.199999999999999956 ) ) ;
#29910 = AXIS2_PLACEMENT_3D ( 'NONE', #13232, #43088, #9537 ) ;
#29911 = CARTESIAN_POINT ( 'NONE',  ( 24.95699195200417364, -110.9640411295978595, -2.500000000000000000 ) ) ;
#29912 = CARTESIAN_POINT ( 'NONE',  ( 0.000000000000000000, 56.15606465355041621, -59.75363087400017292 ) ) ;
#29914 = AXIS2_PLACEMENT_3D ( 'NONE', #8378, #20583, #1518 ) ;
#29913 = FACE_OUTER_BOUND ( 'NONE', #4780, .T. ) ;
#29915 = DIRECTION ( 'NONE',  ( -1.000000000000000000, -0.000000000000000000, -0.000000000000000000 ) ) ;
#29916 = EDGE_LOOP ( 'NONE', ( #7003, #40931, #34615, #43915 ) ) ;
#29917 = CIRCLE ( 'NONE', #25208, 82.00000000000000000 ) ;
#29918 = EDGE_CURVE ( 'NONE', #2128, #25169, #12769, .T. ) ;
#29919 = VERTEX_POINT ( 'NONE', #19847 ) ;
#29920 = AXIS2_PLACEMENT_3D ( 'NONE', #29652, #6667, #25240 ) ;
#29921 = DIRECTION ( 'NONE',  ( -1.000000000000000000, 0.000000000000000000, 0.000000000000000000 ) ) ;
#29922 = ORIENTED_EDGE ( 'NONE', *, *, #34134, .T. ) ;
#29923 = CARTESIAN_POINT ( 'NONE',  ( 10.00000000000000000, -8.830959090341869100, -74.65491531819127147 ) ) ;
#29924 = VECTOR ( 'NONE', #21213, 1000.000000000000000 ) ;
#29925 = DIRECTION ( 'NONE',  ( -3.065994397161057213E-18, 1.942648362116681808E-16, 1.000000000000000000 ) ) ;
#29926 = DIRECTION ( 'NONE',  ( -1.000000000000000000, 0.000000000000000000, 0.000000000000000000 ) ) ;
#29927 = ORIENTED_EDGE ( 'NONE', *, *, #3190, .F. ) ;
#29928 = VECTOR ( 'NONE', #11868, 1000.000000000000000 ) ;
#29929 = FACE_OUTER_BOUND ( 'NONE', #24177, .T. ) ;
#29930 = EDGE_LOOP ( 'NONE', ( #13928, #31284, #8366, #4175 ) ) ;
#29931 = ORIENTED_EDGE ( 'NONE', *, *, #46418, .T. ) ;
#29932 = CARTESIAN_POINT ( 'NONE',  ( 11.99999999999999822, 0.000000000000000000, 0.000000000000000000 ) ) ;
#29933 = EDGE_CURVE ( 'NONE', #42774, #21856, #26802, .T. ) ;
#29934 = DIRECTION ( 'NONE',  ( 0.4796670183876304283, -0.8774505977381978905, 0.000000000000000000 ) ) ;
#29936 = VERTEX_POINT ( 'NONE', #8120 ) ;
#29935 = FACE_OUTER_BOUND ( 'NONE', #14544, .T. ) ;
#29937 = VERTEX_POINT ( 'NONE', #23055 ) ;
#29938 = EDGE_CURVE ( 'NONE', #11028, #43074, #7270, .T. ) ;
#29939 = AXIS2_PLACEMENT_3D ( 'NONE', #8062, #22999, #25691 ) ;
#29940 = EDGE_CURVE ( 'NONE', #21411, #17540, #23297, .T. ) ;
#29941 = EDGE_CURVE ( 'NONE', #7495, #8522, #21349, .T. ) ;
#29942 = CYLINDRICAL_SURFACE ( 'NONE', #43236, 82.00000000000000000 ) ;
#29943 = DIRECTION ( 'NONE',  ( 0.000000000000000000, 0.000000000000000000, 1.000000000000000000 ) ) ;
#29944 = CYLINDRICAL_SURFACE ( 'NONE', #11862, 31.99999999999998579 ) ;
#29945 = FACE_OUTER_BOUND ( 'NONE', #24988, .T. ) ;
#29946 = ORIENTED_EDGE ( 'NONE', *, *, #4982, .F. ) ;
#29947 = CARTESIAN_POINT ( 'NONE',  ( 10.00000000000000000, 26.01480285779933510, -70.53064760720289428 ) ) ;
#29948 = VERTEX_POINT ( 'NONE', #24744 ) ;
#29949 = VERTEX_POINT ( 'NONE', #39191 ) ;
#29950 = EDGE_CURVE ( 'NONE', #23745, #15994, #17625, .T. ) ;
#29951 = AXIS2_PLACEMENT_3D ( 'NONE', #31481, #19958, #12626 ) ;
#29952 = DIRECTION ( 'NONE',  ( -1.000000000000000000, -0.000000000000000000, -0.000000000000000000 ) ) ;
#29953 = CARTESIAN_POINT ( 'NONE',  ( 14.09999999999999964, 0.000000000000000000, -1.199999999999999956 ) ) ;
#29954 = CYLINDRICAL_SURFACE ( 'NONE', #10963, 77.49899999999999523 ) ;
#29955 = DIRECTION ( 'NONE',  ( 1.000000000000000000, -0.000000000000000000, -0.000000000000000000 ) ) ;
#29956 = ORIENTED_EDGE ( 'NONE', *, *, #29172, .F. ) ;
#29957 = CARTESIAN_POINT ( 'NONE',  ( 10.00000000000000000, 0.000000000000000000, 0.000000000000000000 ) ) ;
#29958 = CIRCLE ( 'NONE', #12010, 16.00000000000000711 ) ;
#29959 = LINE ( 'NONE', #26297, #23670 ) ;
#29960 = LINE ( 'NONE', #14798, #37569 ) ;
#29961 = LINE ( 'NONE', #18211, #40827 ) ;
#29962 = DIRECTION ( 'NONE',  ( -1.000000000000000000, 0.000000000000000000, 0.000000000000000000 ) ) ;
#29963 = AXIS2_PLACEMENT_3D ( 'NONE', #31939, #39994, #43430 ) ;
#29964 = CIRCLE ( 'NONE', #21319, 42.00000000000000000 ) ;
#29965 = DIRECTION ( 'NONE',  ( 0.000000000000000000, 0.000000000000000000, -1.000000000000000000 ) ) ;
#29966 = EDGE_CURVE ( 'NONE', #40106, #39158, #46367, .T. ) ;
#29967 = PLANE ( 'NONE',  #21640 ) ;
#29968 = DIRECTION ( 'NONE',  ( -1.000000000000000000, 0.000000000000000000, 0.000000000000000000 ) ) ;
#29969 = AXIS2_PLACEMENT_3D ( 'NONE', #16688, #27716, #5431 ) ;
#29970 = CARTESIAN_POINT ( 'NONE',  ( 11.99999999999999822, 0.000000000000000000, 0.000000000000000000 ) ) ;
#29971 = DIRECTION ( 'NONE',  ( 1.000000000000000000, -0.000000000000000000, -0.000000000000000000 ) ) ;
#29972 = CIRCLE ( 'NONE', #42485, 31.99999999999998934 ) ;
#29973 = FACE_BOUND ( 'NONE', #33792, .T. ) ;
#29974 = ADVANCED_FACE ( 'NONE', ( #25198 ), #5911, .T. ) ;
#29975 = ORIENTED_EDGE ( 'NONE', *, *, #43121, .F. ) ;
#29976 = CARTESIAN_POINT ( 'NONE',  ( 11.99999999999999822, 0.000000000000000000, 0.000000000000000000 ) ) ;
#29977 = FACE_OUTER_BOUND ( 'NONE', #28739, .T. ) ;
#29978 = DIRECTION ( 'NONE',  ( -1.000000000000000000, 0.000000000000000000, 0.000000000000000000 ) ) ;
#29979 = LINE ( 'NONE', #32915, #5907 ) ;
#29980 = ADVANCED_FACE ( 'NONE', ( #6140 ), #43102, .F. ) ;
#29981 = CARTESIAN_POINT ( 'NONE',  ( 10.00000000000000000, -36.88895765772637247, 6.736453364083436313 ) ) ;
#29982 = ORIENTED_EDGE ( 'NONE', *, *, #38, .T. ) ;
#29983 = VERTEX_POINT ( 'NONE', #5660 ) ;
#29984 = CIRCLE ( 'NONE', #8068, 31.99999999999998934 ) ;
#29985 = EDGE_CURVE ( 'NONE', #28552, #15863, #32326, .T. ) ;
#29986 = ORIENTED_EDGE ( 'NONE', *, *, #39007, .F. ) ;
#29987 = AXIS2_PLACEMENT_3D ( 'NONE', #38514, #19411, #4979 ) ;
#29988 = AXIS2_PLACEMENT_3D ( 'NONE', #47415, #32956, #29300 ) ;
#29989 = AXIS2_PLACEMENT_3D ( 'NONE', #5071, #38353, #8721 ) ;
#29990 = ORIENTED_EDGE ( 'NONE', *, *, #14591, .T. ) ;
#29991 = CYLINDRICAL_SURFACE ( 'NONE', #22646, 16.00000000000000000 ) ;
#29992 = VERTEX_POINT ( 'NONE', #47487 ) ;
#29993 = EDGE_CURVE ( 'NONE', #13636, #19576, #231, .T. ) ;
#29994 = VECTOR ( 'NONE', #32579, 1000.000000000000000 ) ;
#29995 = AXIS2_PLACEMENT_3D ( 'NONE', #4032, #22624, #11389 ) ;
#29996 = CARTESIAN_POINT ( 'NONE',  ( 11.99999999999999822, 0.000000000000000000, 0.000000000000000000 ) ) ;
#29997 = CIRCLE ( 'NONE', #34667, 16.00000000000000355 ) ;
#29998 = ADVANCED_FACE ( 'NONE', ( #13730 ), #20573, .T. ) ;
#29999 = DIRECTION ( 'NONE',  ( 1.000000000000000000, -0.000000000000000000, -0.000000000000000000 ) ) ;
#30000 = DIRECTION ( 'NONE',  ( 0.000000000000000000, 0.000000000000000000, 1.000000000000000000 ) ) ;
#30001 = ORIENTED_EDGE ( 'NONE', *, *, #24413, .F. ) ;
#30002 = CARTESIAN_POINT ( 'NONE',  ( 10.00000000000000000, 35.47612816024523141, 22.48208911017513145 ) ) ;
#30003 = ORIENTED_EDGE ( 'NONE', *, *, #28474, .T. ) ;
#30004 = ADVANCED_FACE ( 'NONE', ( #47709 ), #2937, .T. ) ;
#30005 = ORIENTED_EDGE ( 'NONE', *, *, #17880, .F. ) ;
#30006 = EDGE_LOOP ( 'NONE', ( #44115, #25016, #42538, #25544 ) ) ;
#30007 = VECTOR ( 'NONE', #46077, 1000.000000000000000 ) ;
#30008 = EDGE_CURVE ( 'NONE', #36384, #42951, #8841, .T. ) ;
#30009 = CARTESIAN_POINT ( 'NONE',  ( 0.000000000000000000, 73.44644590900094272, -24.73286445877628026 ) ) ;
#30010 = DIRECTION ( 'NONE',  ( 0.000000000000000000, 0.3090169943749410120, 0.9510565162951557516 ) ) ;
#30011 = CARTESIAN_POINT ( 'NONE',  ( -10.00000000000000000, 0.000000000000000000, 0.000000000000000000 ) ) ;
#30012 = ORIENTED_EDGE ( 'NONE', *, *, #17131, .T. ) ;
#30013 = ORIENTED_EDGE ( 'NONE', *, *, #21770, .F. ) ;
#30014 = DIRECTION ( 'NONE',  ( 0.000000000000000000, 0.000000000000000000, 1.000000000000000000 ) ) ;
#30015 = ORIENTED_EDGE ( 'NONE', *, *, #23986, .T. ) ;
#30016 = EDGE_CURVE ( 'NONE', #410, #2592, #14200, .T. ) ;
#30017 = LINE ( 'NONE', #29533, #10548 ) ;
#30018 = CARTESIAN_POINT ( 'NONE',  ( 10.00000000000000000, -40.98264845739743834, -9.188173127307738497 ) ) ;
#30019 = DIRECTION ( 'NONE',  ( -1.000000000000000000, -0.000000000000000000, -0.000000000000000000 ) ) ;
#30020 = DIRECTION ( 'NONE',  ( 0.000000000000000000, 0.3090169943749479509, -0.9510565162951534202 ) ) ;
#30021 = CARTESIAN_POINT ( 'NONE',  ( 0.000000000000000000, 35.38097989696512968, 12.42422080174651100 ) ) ;
#30022 = CARTESIAN_POINT ( 'NONE',  ( 0.000000000000000000, 73.95703589263973754, 23.16143007188452430 ) ) ;
#30023 = CYLINDRICAL_SURFACE ( 'NONE', #2968, 42.00000000000000000 ) ;
#30024 = AXIS2_PLACEMENT_3D ( 'NONE', #35706, #2175, #46961 ) ;
#30025 = DIRECTION ( 'NONE',  ( -1.000000000000000000, 0.000000000000000000, 0.000000000000000000 ) ) ;
#30026 = DIRECTION ( 'NONE',  ( 1.000000000000000000, -0.000000000000000000, 0.000000000000000000 ) ) ;
#30027 = ORIENTED_EDGE ( 'NONE', *, *, #12483, .F. ) ;
#30028 = LINE ( 'NONE', #3839, #3251 ) ;
#30029 = AXIS2_PLACEMENT_3D ( 'NONE', #36747, #10092, #25242 ) ;
#30030 = ORIENTED_EDGE ( 'NONE', *, *, #30667, .T. ) ;
#30031 = PLANE ( 'NONE',  #36657 ) ;
#30032 = CIRCLE ( 'NONE', #2646, 15.77977592589476608 ) ;
#30033 = VECTOR ( 'NONE', #40286, 1000.000000000000114 ) ;
#30034 = CARTESIAN_POINT ( 'NONE',  ( 11.99999999999999822, 70.53064760720278059, 26.01480285779964774 ) ) ;
#30035 = DIRECTION ( 'NONE',  ( 1.000000000000000000, 0.000000000000000000, -0.000000000000000000 ) ) ;
#30036 = DIRECTION ( 'NONE',  ( -1.000000000000000000, 0.000000000000000000, 0.000000000000000000 ) ) ;
#30037 = CARTESIAN_POINT ( 'NONE',  ( 10.00000000000000000, 0.000000000000000000, 0.000000000000000000 ) ) ;
#30038 = CARTESIAN_POINT ( 'NONE',  ( 10.00000000000000000, 76.66974797899852945, -11.30684508768257679 ) ) ;
#30039 = VERTEX_POINT ( 'NONE', #42870 ) ;
#30040 = VECTOR ( 'NONE', #43047, 1000.000000000000000 ) ;
#30041 = CIRCLE ( 'NONE', #6557, 37.49900000000000233 ) ;
#30042 = DIRECTION ( 'NONE',  ( -1.000000000000000000, -0.000000000000000000, 0.000000000000000000 ) ) ;
#30043 = CARTESIAN_POINT ( 'NONE',  ( 10.00000000000000000, -75.11725578898470701, 2.956366410620372864 ) ) ;
#30044 = CIRCLE ( 'NONE', #20639, 31.99999999999999645 ) ;
#30045 = CIRCLE ( 'NONE', #36297, 1.000000000000000000 ) ;
#30046 = DIRECTION ( 'NONE',  ( -1.000000000000000000, -0.000000000000000000, -0.000000000000000000 ) ) ;
#30047 = DIRECTION ( 'NONE',  ( -1.000000000000000000, -0.000000000000000000, -0.000000000000000000 ) ) ;
#30048 = VECTOR ( 'NONE', #23162, 1000.000000000000000 ) ;
#30049 = VERTEX_POINT ( 'NONE', #39438 ) ;
#30050 = EDGE_LOOP ( 'NONE', ( #20670, #11872, #43313, #42909 ) ) ;
#30051 = EDGE_CURVE ( 'NONE', #21369, #410, #10043, .T. ) ;
#30052 = ORIENTED_EDGE ( 'NONE', *, *, #14203, .T. ) ;
#30053 = ORIENTED_EDGE ( 'NONE', *, *, #43676, .T. ) ;
#30054 = AXIS2_PLACEMENT_3D ( 'NONE', #22337, #29663, #31078 ) ;
#30055 = CARTESIAN_POINT ( 'NONE',  ( 0.000000000000000000, 30.84782396557248418, -21.32104025579081252 ) ) ;
#30056 = CARTESIAN_POINT ( 'NONE',  ( 11.99999999999999822, 62.50884508063487033, -41.76106447765422303 ) ) ;
#30057 = ORIENTED_EDGE ( 'NONE', *, *, #2570, .F. ) ;
#30058 = ORIENTED_EDGE ( 'NONE', *, *, #2016, .F. ) ;
#30059 = AXIS2_PLACEMENT_3D ( 'NONE', #14188, #17364, #18084 ) ;
#30060 = LINE ( 'NONE', #23427, #39792 ) ;
#30061 = AXIS2_PLACEMENT_3D ( 'NONE', #26331, #374, #18958 ) ;
#30062 = AXIS2_PLACEMENT_3D ( 'NONE', #13310, #16977, #28233 ) ;
#30063 = VERTEX_POINT ( 'NONE', #24494 ) ;
#30064 = VERTEX_POINT ( 'NONE', #2689 ) ;
#30065 = EDGE_CURVE ( 'NONE', #40628, #24345, #3349, .T. ) ;
#30066 = PLANE ( 'NONE',  #25682 ) ;
#30067 = EDGE_CURVE ( 'NONE', #15931, #30390, #19763, .T. ) ;
#30069 = ORIENTED_EDGE ( 'NONE', *, *, #21723, .F. ) ;
#30068 = CARTESIAN_POINT ( 'NONE',  ( 20.85212586905262100, -130.9402397935870965, -5.500000000000000000 ) ) ;
#30070 = FACE_OUTER_BOUND ( 'NONE', #40094, .T. ) ;
#30071 = AXIS2_PLACEMENT_3D ( 'NONE', #18001, #26083, #3566 ) ;
#30072 = AXIS2_PLACEMENT_3D ( 'NONE', #9806, #39439, #1749 ) ;
#30073 = ORIENTED_EDGE ( 'NONE', *, *, #36381, .T. ) ;
#30074 = CARTESIAN_POINT ( 'NONE',  ( 5.000000000000002665, -8.966570791701281351, 81.50828551894224461 ) ) ;
#30075 = ORIENTED_EDGE ( 'NONE', *, *, #24250, .T. ) ;
#30076 = VECTOR ( 'NONE', #13899, 1000.000000000000000 ) ;
#30077 = EDGE_CURVE ( 'NONE', #7503, #44271, #21057, .T. ) ;
#30078 = LINE ( 'NONE', #34214, #25938 ) ;
#30079 = AXIS2_PLACEMENT_3D ( 'NONE', #2435, #35976, #13715 ) ;
#30080 = EDGE_CURVE ( 'NONE', #46139, #25303, #6383, .T. ) ;
#30081 = DIRECTION ( 'NONE',  ( 0.000000000000000000, 0.8660254037844368202, 0.5000000000000029976 ) ) ;
#30082 = LINE ( 'NONE', #44752, #3312 ) ;
#30084 = ORIENTED_EDGE ( 'NONE', *, *, #43604, .T. ) ;
#30083 = VECTOR ( 'NONE', #44173, 1000.000000000000000 ) ;
#30085 = VERTEX_POINT ( 'NONE', #47961 ) ;
#30086 = DIRECTION ( 'NONE',  ( -1.000000000000000000, 0.000000000000000000, -0.000000000000000000 ) ) ;
#30087 = PLANE ( 'NONE',  #35274 ) ;
#30088 = ORIENTED_EDGE ( 'NONE', *, *, #12065, .T. ) ;
#30089 = ORIENTED_EDGE ( 'NONE', *, *, #30711, .T. ) ;
#30090 =( REPRESENTATION_RELATIONSHIP ('NONE','NONE', #5957, #21223 ) REPRESENTATION_RELATIONSHIP_WITH_TRANSFORMATION ( #13255 )SHAPE_REPRESENTATION_RELATIONSHIP( ) );
#30091 = DIRECTION ( 'NONE',  ( 0.000000000000000000, 0.000000000000000000, 1.000000000000000000 ) ) ;
#30092 = ORIENTED_EDGE ( 'NONE', *, *, #11228, .T. ) ;
#30093 = DIRECTION ( 'NONE',  ( 0.000000000000000000, 0.000000000000000000, 1.000000000000000000 ) ) ;
#30094 = CARTESIAN_POINT ( 'NONE',  ( -3.360000000000002096, 0.000000000000000000, 0.000000000000000000 ) ) ;
#30095 = CARTESIAN_POINT ( 'NONE',  ( 10.00000000000000000, 32.34446384429971744, 26.79245525562727082 ) ) ;
#30096 = DIRECTION ( 'NONE',  ( -1.000000000000000000, -0.000000000000000000, 0.000000000000000000 ) ) ;
#30097 = CARTESIAN_POINT ( 'NONE',  ( -30.50000000000000000, -120.0000000000000000, 5.500000000000000888 ) ) ;
#30098 = LINE ( 'NONE', #45026, #37504 ) ;
#30099 = DIRECTION ( 'NONE',  ( 1.000000000000000000, 0.000000000000000000, 0.000000000000000000 ) ) ;
#30100 = AXIS2_PLACEMENT_3D ( 'NONE', #9976, #37316, #20993 ) ;
#30101 = CARTESIAN_POINT ( 'NONE',  ( -7.543218489614351263, -11.91259227951415056, -1.199999999999999956 ) ) ;
#30102 = CARTESIAN_POINT ( 'NONE',  ( 0.000000000000000000, -39.47590169984793818, -71.87247863392457248 ) ) ;
#30103 = ORIENTED_EDGE ( 'NONE', *, *, #98, .T. ) ;
#30104 = AXIS2_PLACEMENT_3D ( 'NONE', #1314, #11603, #22849 ) ;
#30105 = CARTESIAN_POINT ( 'NONE',  ( 0.000000000000000000, 0.000000000000000000, 0.000000000000000000 ) ) ;
#30106 = DIRECTION ( 'NONE',  ( -1.000000000000000000, 0.000000000000000000, -0.000000000000000000 ) ) ;
#30107 =( NAMED_UNIT ( * ) PLANE_ANGLE_UNIT ( ) SI_UNIT ( $, .RADIAN. ) );
#30108 = DIRECTION ( 'NONE',  ( -0.000000000000000000, -0.000000000000000000, -1.000000000000000000 ) ) ;
#30109 = EDGE_CURVE ( 'NONE', #127, #20106, #31545, .T. ) ;
#30110 = EDGE_LOOP ( 'NONE', ( #47752, #30980 ) ) ;
#30111 = ADVANCED_FACE ( 'NONE', ( #33283 ), #18351, .T. ) ;
#30112 = CIRCLE ( 'NONE', #37122, 42.00000000000000000 ) ;
#30113 = AXIS2_PLACEMENT_3D ( 'NONE', #15056, #18225, #26064 ) ;
#30114 = UNCERTAINTY_MEASURE_WITH_UNIT (LENGTH_MEASURE( 1.000000000000000082E-05 ), #4857, 'distance_accuracy_value', 'NONE');
#30115 = DIRECTION ( 'NONE',  ( -1.000000000000000000, -0.000000000000000000, -0.000000000000000000 ) ) ;
#30116 = EDGE_CURVE ( 'NONE', #188, #18133, #22514, .T. ) ;
#30117 = CIRCLE ( 'NONE', #14499, 77.49900000000002365 ) ;
#30118 = CYLINDRICAL_SURFACE ( 'NONE', #26058, 32.00000000000000000 ) ;
#30119 = DIRECTION ( 'NONE',  ( 0.000000000000000000, 0.4539904997395413089, 0.8910065241883705633 ) ) ;
#30120 = EDGE_CURVE ( 'NONE', #19539, #47351, #25446, .T. ) ;
#30121 = CIRCLE ( 'NONE', #26199, 77.49900000000002365 ) ;
#30122 = ORIENTED_EDGE ( 'NONE', *, *, #16262, .T. ) ;
#30123 = CIRCLE ( 'NONE', #30163, 77.49899999999999523 ) ;
#30124 = DIRECTION ( 'NONE',  ( -1.000000000000000000, 0.000000000000000000, 0.000000000000000000 ) ) ;
#30125 = ORIENTED_EDGE ( 'NONE', *, *, #36381, .F. ) ;
#30126 = VERTEX_POINT ( 'NONE', #6860 ) ;
#30127 = ORIENTED_EDGE ( 'NONE', *, *, #17166, .F. ) ;
#30128 = ORIENTED_EDGE ( 'NONE', *, *, #44008, .F. ) ;
#30129 = VECTOR ( 'NONE', #19070, 1000.000000000000114 ) ;
#30130 = CYLINDRICAL_SURFACE ( 'NONE', #43316, 16.00000000000000000 ) ;
#30131 = ADVANCED_FACE ( 'NONE', ( #7088 ), #44300, .T. ) ;
#30132 = EDGE_CURVE ( 'NONE', #17599, #21447, #8031, .T. ) ;
#30133 = EDGE_CURVE ( 'NONE', #4884, #30895, #11998, .T. ) ;
#30134 = VECTOR ( 'NONE', #19190, 1000.000000000000114 ) ;
#30135 = CARTESIAN_POINT ( 'NONE',  ( 10.00000000000000000, 10.96151621346487914, 35.95386929396260456 ) ) ;
#30136 = VERTEX_POINT ( 'NONE', #11011 ) ;
#30137 = VERTEX_POINT ( 'NONE', #25931 ) ;
#30138 = CARTESIAN_POINT ( 'NONE',  ( 0.000000000000000000, 0.000000000000000000, 0.000000000000000000 ) ) ;
#30139 = VERTEX_POINT ( 'NONE', #3907 ) ;
#30140 = DIRECTION ( 'NONE',  ( 0.000000000000000000, -0.5877852522924787992, -0.8090169943749434545 ) ) ;
#30141 = LINE ( 'NONE', #19343, #22862 ) ;
#30142 = ORIENTED_EDGE ( 'NONE', *, *, #42558, .F. ) ;
#30143 = ORIENTED_EDGE ( 'NONE', *, *, #36362, .F. ) ;
#30144 = DIRECTION ( 'NONE',  ( 0.000000000000000000, -0.9510565162951565288, 0.3090169943749382919 ) ) ;
#30145 = CARTESIAN_POINT ( 'NONE',  ( 11.99999999999999822, 8.840884882376133902, -74.65374052328640175 ) ) ;
#30146 = VERTEX_POINT ( 'NONE', #40399 ) ;
#30147 = ADVANCED_FACE ( 'NONE', ( #7817 ), #220, .T. ) ;
#30148 = DIRECTION ( 'NONE',  ( 1.000000000000000000, -0.000000000000000000, -0.000000000000000000 ) ) ;
#30149 = DIRECTION ( 'NONE',  ( 0.000000000000000000, 0.2079116908177664480, -0.9781476007338041345 ) ) ;
#30150 = AXIS2_PLACEMENT_3D ( 'NONE', #4000, #41212, #45583 ) ;
#30151 = VECTOR ( 'NONE', #11102, 1000.000000000000000 ) ;
#30152 = ORIENTED_EDGE ( 'NONE', *, *, #8392, .T. ) ;
#30153 = DIRECTION ( 'NONE',  ( 0.000000000000000000, -0.9781476007338070211, 0.2079116908177525425 ) ) ;
#30154 = ORIENTED_EDGE ( 'NONE', *, *, #40078, .F. ) ;
#30155 = CARTESIAN_POINT ( 'NONE',  ( -32.50000000000000000, -120.0000000000000000, 102.9091629284897493 ) ) ;
#30156 = DIRECTION ( 'NONE',  ( -1.000000000000000000, 0.000000000000000000, 0.000000000000000000 ) ) ;
#30157 = DIRECTION ( 'NONE',  ( 0.000000000000000000, -0.9510565162951500895, -0.3090169943749583314 ) ) ;
#30158 = AXIS2_PLACEMENT_3D ( 'NONE', #12108, #1062, #818 ) ;
#30159 = DIRECTION ( 'NONE',  ( 0.5200609990133008287, 0.8541291221503266584, -0.000000000000000000 ) ) ;
#30160 = CARTESIAN_POINT ( 'NONE',  ( -10.00000000000000000, 0.000000000000000000, 0.000000000000000000 ) ) ;
#30161 = AXIS2_PLACEMENT_3D ( 'NONE', #20372, #13777, #9361 ) ;
#30162 = DIRECTION ( 'NONE',  ( -1.000000000000000000, 0.000000000000000000, 0.000000000000000000 ) ) ;
#30163 = AXIS2_PLACEMENT_3D ( 'NONE', #10254, #17833, #14667 ) ;
#30164 = CARTESIAN_POINT ( 'NONE',  ( 10.00000000000000000, 51.02545421589324803, 55.20638768913779870 ) ) ;
#30165 = DIRECTION ( 'NONE',  ( -0.000000000000000000, -1.000000000000000000, -0.000000000000000000 ) ) ;
#30166 = VERTEX_POINT ( 'NONE', #14691 ) ;
#30167 = CARTESIAN_POINT ( 'NONE',  ( 10.00000000000000000, 0.000000000000000000, 0.000000000000000000 ) ) ;
#30168 = CARTESIAN_POINT ( 'NONE',  ( -11.59517495878806947, -96.12423995607481686, -5.500000000000000000 ) ) ;
#30169 = CARTESIAN_POINT ( 'NONE',  ( 10.00000000000000000, -12.42422080174663712, 35.38097989696507994 ) ) ;
#30170 = LINE ( 'NONE', #34060, #39574 ) ;
#30171 = AXIS2_PLACEMENT_3D ( 'NONE', #17569, #13424, #2395 ) ;
#30172 = PLANE ( 'NONE',  #6473 ) ;
#30173 = CARTESIAN_POINT ( 'NONE',  ( 6.000000000000000000, -71.21200624218825226, 40.65526001592589722 ) ) ;
#30174 = DIRECTION ( 'NONE',  ( -0.1276937514489705217, -0.9918136447140101231, 0.000000000000000000 ) ) ;
#30175 = AXIS2_PLACEMENT_3D ( 'NONE', #25321, #17976, #17751 ) ;
#30176 = CYLINDRICAL_SURFACE ( 'NONE', #44440, 77.49899999999999523 ) ;
#30177 = VECTOR ( 'NONE', #5908, 1000.000000000000227 ) ;
#30178 = EDGE_CURVE ( 'NONE', #48063, #39870, #13560, .T. ) ;
#30179 = DIRECTION ( 'NONE',  ( 1.000000000000000000, -0.000000000000000000, -0.000000000000000000 ) ) ;
#30180 = ORIENTED_EDGE ( 'NONE', *, *, #34184, .T. ) ;
#30181 = CARTESIAN_POINT ( 'NONE',  ( 12.49999999999999645, 1.530808498934191127E-15, 42.00000000000001421 ) ) ;
#30182 = EDGE_CURVE ( 'NONE', #44237, #28297, #25281, .T. ) ;
#30183 = CARTESIAN_POINT ( 'NONE',  ( -5.574404190523511974E-14, 1.019753860068740540E-13, -55.00000000000000711 ) ) ;
#30184 = ORIENTED_EDGE ( 'NONE', *, *, #5182, .T. ) ;
#30185 = CARTESIAN_POINT ( 'NONE',  ( 10.00000000000000000, -62.50329211542465657, 41.76937507738766442 ) ) ;
#30186 = AXIS2_PLACEMENT_3D ( 'NONE', #12638, #2331, #31977 ) ;
#30187 = EDGE_CURVE ( 'NONE', #24216, #39388, #4158, .T. ) ;
#30188 = ORIENTED_EDGE ( 'NONE', *, *, #32695, .F. ) ;
#30189 = AXIS2_PLACEMENT_3D ( 'NONE', #10014, #39881, #2421 ) ;
#30190 = DIRECTION ( 'NONE',  ( 0.000000000000000000, 0.000000000000000000, 1.000000000000000000 ) ) ;
#30191 = AXIS2_PLACEMENT_3D ( 'NONE', #16011, #19653, #34583 ) ;
#30192 = ORIENTED_EDGE ( 'NONE', *, *, #2270, .F. ) ;
#30193 = CIRCLE ( 'NONE', #32424, 82.00000000000000000 ) ;
#30194 = EDGE_CURVE ( 'NONE', #7173, #30536, #7333, .T. ) ;
#30195 = EDGE_CURVE ( 'NONE', #5128, #21831, #18229, .T. ) ;
#30196 = CARTESIAN_POINT ( 'NONE',  ( 0.000000000000000000, -5.202137450156655518, 37.22597642581156663 ) ) ;
#30197 = CLOSED_SHELL ( 'NONE', ( #23773, #19382, #31211, #18844, #48344, #41660, #1087, #18705, #38348, #17613, #40770, #6634, #4563, #30593, #28834, #8414, #3838, #3090, #34024, #25034, #1887, #38652, #43912, #48017, #37405, #16948, #37397, #30235, #43539, #385, #46806, #27210, #16816, #28515, #16463, #7281, #24707, #19877, #3323, #34522, #41732, #34360, #40401, #20400, #20548, #11709, #4243, #36635, #8058, #31756, #25239, #33421, #21232, #22589, #36288, #10957, #4085, #41669, #44739, #3544, #48405, #23464, #25175, #32917, #13092, #22315, #4765, #33650, #16436, #29066, #5666, #27244, #30676, #38360, #5314, #1517, #29553, #47727, #2834, #35089, #38089, #34181, #15526, #33854, #46650, #47264, #41798, #17602, #10215, #29171, #38316, #41486, #36350, #19103, #29980, #43327, #17897, #5814, #43104, #1949, #3616, #36898, #46155, #44982, #25465, #1712, #17213, #43722, #14296, #7405, #3524, #35425, #43168, #20446, #3981, #16458, #41196, #12633, #10631, #6077, #12954, #37259, #21980, #45212, #46022, #23648, #30523, #20769, #47991, #21376, #7061, #46463, #2372, #28015, #22268, #1103, #40037, #9862, #44834, #32869, #40125, #1339, #33472, #41336, #5878, #39982, #5473, #21064, #20320, #45206, #46671, #14879, #14818, #16619, #11415, #29118, #14377, #16037, #30561, #47768, #36266, #6849, #31344, #20051, #3354, #29785, #17840, #25143, #33680, #27246 ) ) ;
#30198 = CARTESIAN_POINT ( 'NONE',  ( -3.000000000000000000, -26.23277895567251505, 4.042438405569750870 ) ) ;
#30199 = CARTESIAN_POINT ( 'NONE',  ( 11.99999999999999822, 65.64334221924909230, 41.19522573413756561 ) ) ;
#30200 = EDGE_LOOP ( 'NONE', ( #40577, #23019, #26015, #33600 ) ) ;
#30201 = VECTOR ( 'NONE', #4688, 1000.000000000000000 ) ;
#30202 = VECTOR ( 'NONE', #39949, 1000.000000000000000 ) ;
#30203 = CYLINDRICAL_SURFACE ( 'NONE', #43352, 31.99999999999999289 ) ;
#30204 = CYLINDRICAL_SURFACE ( 'NONE', #13238, 32.00000000000000000 ) ;
#30205 = DIRECTION ( 'NONE',  ( -1.000000000000000000, -0.000000000000000000, 0.000000000000000000 ) ) ;
#30206 = EDGE_CURVE ( 'NONE', #3893, #18061, #41688, .T. ) ;
#30207 = VECTOR ( 'NONE', #33280, 1000.000000000000000 ) ;
#30208 = CARTESIAN_POINT ( 'NONE',  ( 10.00000000000000000, -21.53537804866058991, -30.80686688397033635 ) ) ;
#30209 = VERTEX_POINT ( 'NONE', #18596 ) ;
#30210 = CARTESIAN_POINT ( 'NONE',  ( 10.00000000000000000, 46.21855187248719687, -62.20884554313968806 ) ) ;
#30211 = ORIENTED_EDGE ( 'NONE', *, *, #13421, .F. ) ;
#30212 = VERTEX_POINT ( 'NONE', #11260 ) ;
#30213 = CARTESIAN_POINT ( 'NONE',  ( 10.00000000000000000, -16.65560815589439159, 38.55633173627004595 ) ) ;
#30214 = CARTESIAN_POINT ( 'NONE',  ( 10.00000000000000000, 6.736453364084091788, -36.88895765772625879 ) ) ;
#30215 = LINE ( 'NONE', #3768, #11072 ) ;
#30216 = CARTESIAN_POINT ( 'NONE',  ( 6.000000000000000000, -80.28980883073769803, 16.65972982744905551 ) ) ;
#30217 = ORIENTED_EDGE ( 'NONE', *, *, #39969, .F. ) ;
#30218 = DIRECTION ( 'NONE',  ( 1.000000000000000000, 0.000000000000000000, -0.000000000000000000 ) ) ;
#30219 = DIRECTION ( 'NONE',  ( -1.000000000000000000, -0.000000000000000000, -0.000000000000000000 ) ) ;
#30220 = DIRECTION ( 'NONE',  ( -1.000000000000000000, -0.000000000000000000, 0.000000000000000000 ) ) ;
#30221 = CARTESIAN_POINT ( 'NONE',  ( 0.000000000000000000, -120.0000000000000000, -5.500000000000000000 ) ) ;
#30222 = CARTESIAN_POINT ( 'NONE',  ( 10.00000000000000000, 63.18004540533092239, -44.88180994100307686 ) ) ;
#30223 = CARTESIAN_POINT ( 'NONE',  ( 5.999999999999999112, 27.74655509720779989, -77.16300072079631889 ) ) ;
#30224 = ORIENTED_EDGE ( 'NONE', *, *, #44382, .F. ) ;
#30225 = DIRECTION ( 'NONE',  ( 1.000000000000000000, 0.000000000000000000, 0.000000000000000000 ) ) ;
#30226 = CARTESIAN_POINT ( 'NONE',  ( 10.00000000000000000, 0.000000000000000000, 0.000000000000000000 ) ) ;
#30227 = CYLINDRICAL_SURFACE ( 'NONE', #30653, 77.49899999999999523 ) ;
#30228 = CARTESIAN_POINT ( 'NONE',  ( 0.000000000000000000, -23.29833615347104825, -3.418703333116803744 ) ) ;
#30229 = DIRECTION ( 'NONE',  ( -1.000000000000000000, 0.000000000000000000, 0.000000000000000000 ) ) ;
#30230 = CARTESIAN_POINT ( 'NONE',  ( -16.06301359042743115, -102.7814171781257357, -5.500000000000000000 ) ) ;
#30231 = LINE ( 'NONE', #38055, #34695 ) ;
#30232 = CIRCLE ( 'NONE', #16153, 82.00000000000000000 ) ;
#30233 = DIRECTION ( 'NONE',  ( -1.000000000000000000, 0.000000000000000000, 0.000000000000000000 ) ) ;
#30234 = ORIENTED_EDGE ( 'NONE', *, *, #9541, .F. ) ;
#30235 = ADVANCED_FACE ( 'NONE', ( #11507 ), #26186, .F. ) ;
#30236 = CIRCLE ( 'NONE', #27908, 16.00000000000000000 ) ;
#30237 = ADVANCED_FACE ( 'NONE', ( #44056 ), #10532, .T. ) ;
#30238 = FACE_OUTER_BOUND ( 'NONE', #32975, .T. ) ;
#30239 = EDGE_CURVE ( 'NONE', #38423, #29150, #11739, .T. ) ;
#30240 = VERTEX_POINT ( 'NONE', #1207 ) ;
#30241 = ORIENTED_EDGE ( 'NONE', *, *, #11341, .F. ) ;
#30242 = CIRCLE ( 'NONE', #10709, 77.49899999999999523 ) ;
#30243 = ADVANCED_FACE ( 'NONE', ( #38668 ), #23971, .T. ) ;
#30244 = ORIENTED_EDGE ( 'NONE', *, *, #38976, .F. ) ;
#30245 = CARTESIAN_POINT ( 'NONE',  ( 4.999999999999999112, -3.925862922255855647, -41.81611651403866858 ) ) ;
#30246 = ORIENTED_EDGE ( 'NONE', *, *, #22179, .F. ) ;
#30247 = EDGE_CURVE ( 'NONE', #20016, #7287, #47173, .T. ) ;
#30248 = VECTOR ( 'NONE', #37109, 1000.000000000000114 ) ;
#30249 = DIRECTION ( 'NONE',  ( -1.000000000000000000, 0.000000000000000000, 0.000000000000000000 ) ) ;
#30250 = EDGE_CURVE ( 'NONE', #4970, #17460, #29984, .T. ) ;
#30251 = CARTESIAN_POINT ( 'NONE',  ( 10.00000000000000000, 0.000000000000000000, 0.000000000000000000 ) ) ;
#30252 = CARTESIAN_POINT ( 'NONE',  ( -21.67772167707813935, -110.8034581014852762, 5.500000000000000000 ) ) ;
#30253 = ORIENTED_EDGE ( 'NONE', *, *, #17332, .T. ) ;
#30254 = CIRCLE ( 'NONE', #16176, 77.49900000000000944 ) ;
#30255 = DIRECTION ( 'NONE',  ( -1.000000000000000000, 0.000000000000000000, 0.000000000000000000 ) ) ;
#30256 = VERTEX_POINT ( 'NONE', #46235 ) ;
#30257 = ORIENTED_EDGE ( 'NONE', *, *, #45335, .F. ) ;
#30258 = ORIENTED_EDGE ( 'NONE', *, *, #12143, .F. ) ;
#30259 = DIRECTION ( 'NONE',  ( 0.000000000000000000, -0.4999999999999913403, -0.8660254037844435926 ) ) ;
#30260 = DIRECTION ( 'NONE',  ( -0.000000000000000000, -0.000000000000000000, 1.000000000000000000 ) ) ;
#30261 = EDGE_CURVE ( 'NONE', #17177, #2793, #38406, .T. ) ;
#30262 = DIRECTION ( 'NONE',  ( -1.000000000000000000, 0.000000000000000000, 0.000000000000000000 ) ) ;
#30263 = ORIENTED_EDGE ( 'NONE', *, *, #9279, .T. ) ;
#30264 = ORIENTED_EDGE ( 'NONE', *, *, #47119, .F. ) ;
#30265 = ORIENTED_EDGE ( 'NONE', *, *, #44801, .T. ) ;
#30266 = CIRCLE ( 'NONE', #9925, 31.99999999999998224 ) ;
#30267 = ORIENTED_EDGE ( 'NONE', *, *, #12479, .F. ) ;
#30268 = CARTESIAN_POINT ( 'NONE',  ( 15.00000000000000000, 20.85821328998756385, 10.92862929874494249 ) ) ;
#30269 = ORIENTED_EDGE ( 'NONE', *, *, #16103, .F. ) ;
#30270 = DIRECTION ( 'NONE',  ( -1.000000000000000000, 0.000000000000000000, -0.000000000000000000 ) ) ;
#30271 = DIRECTION ( 'NONE',  ( -1.000000000000000000, 0.000000000000000000, 0.000000000000000000 ) ) ;
#30272 = FACE_OUTER_BOUND ( 'NONE', #21817, .T. ) ;
#30273 = DIRECTION ( 'NONE',  ( -1.000000000000000000, -0.000000000000000000, -0.000000000000000000 ) ) ;
#30274 = DIRECTION ( 'NONE',  ( 0.000000000000000000, 0.000000000000000000, 1.000000000000000000 ) ) ;
#30275 = LINE ( 'NONE', #18265, #11199 ) ;
#30276 = CIRCLE ( 'NONE', #20093, 82.00000000000000000 ) ;
#30277 = CARTESIAN_POINT ( 'NONE',  ( 0.000000000000000000, 0.000000000000000000, 0.000000000000000000 ) ) ;
#30278 = CARTESIAN_POINT ( 'NONE',  ( 11.99999999999999822, 12.93880638057315657, 76.41127070299278046 ) ) ;
#30279 = ORIENTED_EDGE ( 'NONE', *, *, #47591, .T. ) ;
#30280 = ADVANCED_FACE ( 'NONE', ( #35212, #9035 ), #5129, .T. ) ;
#30281 = DIRECTION ( 'NONE',  ( -1.000000000000000000, 0.000000000000000000, 0.000000000000000000 ) ) ;
#30282 = EDGE_LOOP ( 'NONE', ( #20067, #36593, #8745, #38720 ) ) ;
#30283 = ORIENTED_EDGE ( 'NONE', *, *, #9252, .F. ) ;
#30284 = DIRECTION ( 'NONE',  ( -1.000000000000000000, 0.000000000000000000, 0.000000000000000000 ) ) ;
#30285 = DIRECTION ( 'NONE',  ( 0.000000000000000000, 0.000000000000000000, 1.000000000000000000 ) ) ;
#30286 = DIRECTION ( 'NONE',  ( 0.000000000000000000, -0.000000000000000000, 1.000000000000000000 ) ) ;
#30287 = CARTESIAN_POINT ( 'NONE',  ( 11.99999999999999822, 0.000000000000000000, 0.000000000000000000 ) ) ;
#30288 = FACE_OUTER_BOUND ( 'NONE', #46902, .T. ) ;
#30289 = DIRECTION ( 'NONE',  ( 0.000000000000000000, 0.9876883405951371042, 0.1564344650402347547 ) ) ;
#30290 = AXIS2_PLACEMENT_3D ( 'NONE', #34826, #22844, #23563 ) ;
#30291 = ORIENTED_EDGE ( 'NONE', *, *, #1505, .F. ) ;
#30292 = CARTESIAN_POINT ( 'NONE',  ( 5.000000000000002665, -78.73519480814938731, -22.90783923731713756 ) ) ;
#30293 = DIRECTION ( 'NONE',  ( -1.000000000000000000, -0.000000000000000000, -0.000000000000000000 ) ) ;
#30294 = EDGE_CURVE ( 'NONE', #39398, #15461, #27399, .T. ) ;
#30296 = EDGE_CURVE ( 'NONE', #17963, #26344, #35432, .T. ) ;
#30295 = AXIS2_PLACEMENT_3D ( 'NONE', #41072, #47434, #7531 ) ;
#30297 = PRESENTATION_STYLE_ASSIGNMENT (( #4355 ) ) ;
#30298 = DIRECTION ( 'NONE',  ( -0.4279312458752990711, -0.9038112904824846527, 0.000000000000000000 ) ) ;
#30299 = VERTEX_POINT ( 'NONE', #16149 ) ;
#30300 = EDGE_CURVE ( 'NONE', #27337, #9557, #42501, .T. ) ;
#30301 = EDGE_LOOP ( 'NONE', ( #15975, #2063, #1913, #39197 ) ) ;
#30302 = ORIENTED_EDGE ( 'NONE', *, *, #1384, .T. ) ;
#30303 = AXIS2_PLACEMENT_3D ( 'NONE', #11327, #26249, #26487 ) ;
#30304 = EDGE_CURVE ( 'NONE', #10011, #30136, #1453, .T. ) ;
#30305 = VERTEX_POINT ( 'NONE', #26914 ) ;
#30306 = ORIENTED_EDGE ( 'NONE', *, *, #17618, .F. ) ;
#30307 = CARTESIAN_POINT ( 'NONE',  ( 6.000000000000000000, 76.69515212746057387, -29.01471420065479379 ) ) ;
#30308 = DIRECTION ( 'NONE',  ( -1.000000000000000000, 0.000000000000000000, -0.000000000000000000 ) ) ;
#30309 = ORIENTED_EDGE ( 'NONE', *, *, #6875, .T. ) ;
#30310 = AXIS2_PLACEMENT_3D ( 'NONE', #39917, #6387, #34354 ) ;
#30311 = CARTESIAN_POINT ( 'NONE',  ( -23.30023580412278505, -123.4057321492263384, 2.500000000000000000 ) ) ;
#30312 = ORIENTED_EDGE ( 'NONE', *, *, #3010, .T. ) ;
#30313 = ORIENTED_EDGE ( 'NONE', *, *, #24823, .F. ) ;
#30314 = CARTESIAN_POINT ( 'NONE',  ( 10.00000000000000000, 2.663952781846733675, -41.91543099594814947 ) ) ;
#30315 = CARTESIAN_POINT ( 'NONE',  ( 0.000000000000000000, -72.35432306680498016, 20.40083707022857951 ) ) ;
#30316 = AXIS2_PLACEMENT_3D ( 'NONE', #47298, #25491, #36741 ) ;
#30317 = CARTESIAN_POINT ( 'NONE',  ( 0.000000000000000000, -14.67089635893764665, 73.72996012237435082 ) ) ;
#30318 = VERTEX_POINT ( 'NONE', #34723 ) ;
#30319 = DIRECTION ( 'NONE',  ( -0.000000000000000000, -0.9135454576426006446, 0.4067366430758008744 ) ) ;
#30320 = ORIENTED_EDGE ( 'NONE', *, *, #1225, .T. ) ;
#30321 = VERTEX_POINT ( 'NONE', #31083 ) ;
#30322 = DIRECTION ( 'NONE',  ( -0.02332147558787823344, -0.9997280174009349762, 0.000000000000000000 ) ) ;
#30323 = AXIS2_PLACEMENT_3D ( 'NONE', #45234, #26629, #39335 ) ;
#30324 = LINE ( 'NONE', #8026, #18166 ) ;
#30325 = DIRECTION ( 'NONE',  ( -1.000000000000000000, 0.000000000000000000, 0.000000000000000000 ) ) ;
#30326 = ORIENTED_EDGE ( 'NONE', *, *, #46531, .F. ) ;
#30327 = ORIENTED_EDGE ( 'NONE', *, *, #26628, .F. ) ;
#30328 = CARTESIAN_POINT ( 'NONE',  ( 0.000000000000000000, -11.95096189432345390, 23.69967320028757385 ) ) ;
#30329 = ADVANCED_FACE ( 'NONE', ( #8054 ), #46004, .T. ) ;
#30330 = FACE_OUTER_BOUND ( 'NONE', #24302, .T. ) ;
#30331 = ORIENTED_EDGE ( 'NONE', *, *, #22154, .T. ) ;
#30332 = EDGE_LOOP ( 'NONE', ( #19273, #21637, #152, #34758 ) ) ;
#30333 = DIRECTION ( 'NONE',  ( -1.000000000000000000, 0.000000000000000000, 0.000000000000000000 ) ) ;
#30334 = ORIENTED_EDGE ( 'NONE', *, *, #20597, .T. ) ;
#30335 = DIRECTION ( 'NONE',  ( -1.000000000000000000, 0.000000000000000000, -0.000000000000000000 ) ) ;
#30336 = CARTESIAN_POINT ( 'NONE',  ( 16.30584220631899228, -140.9432449716519784, 5.500000000000000000 ) ) ;
#30337 = CARTESIAN_POINT ( 'NONE',  ( 0.000000000000000000, 35.91791733033475253, 68.67312586195009771 ) ) ;
#30338 = CARTESIAN_POINT ( 'NONE',  ( 0.000000000000000000, -33.79645857604501913, -16.45098606841161626 ) ) ;
#30339 = ORIENTED_EDGE ( 'NONE', *, *, #18602, .T. ) ;
#30340 =( GEOMETRIC_REPRESENTATION_CONTEXT ( 3 ) GLOBAL_UNCERTAINTY_ASSIGNED_CONTEXT ( ( #17868 ) ) GLOBAL_UNIT_ASSIGNED_CONTEXT ( ( #38906, #9752, #20775 ) ) REPRESENTATION_CONTEXT ( 'NONE', 'WORKASPACE' ) );
#30341 = DIRECTION ( 'NONE',  ( -0.000000000000000000, -0.000000000000000000, -1.000000000000000000 ) ) ;
#30342 = DIRECTION ( 'NONE',  ( 0.000000000000000000, -0.7071067811865536790, 0.7071067811865413555 ) ) ;
#30343 = CIRCLE ( 'NONE', #42079, 31.99999999999998579 ) ;
#30344 = FACE_OUTER_BOUND ( 'NONE', #44046, .T. ) ;
#30345 = DIRECTION ( 'NONE',  ( 0.000000000000000000, -0.07845909572785234043, 0.9969173337331274087 ) ) ;
#30346 = CARTESIAN_POINT ( 'NONE',  ( 11.99999999999999822, 0.000000000000000000, 0.000000000000000000 ) ) ;
#30347 = ORIENTED_EDGE ( 'NONE', *, *, #21564, .F. ) ;
#30348 = ADVANCED_FACE ( 'NONE', ( #4876 ), #45592, .T. ) ;
#30349 = CARTESIAN_POINT ( 'NONE',  ( 11.99999999999999822, -68.26794271651239399, -31.47745569255214093 ) ) ;
#30350 = CYLINDRICAL_SURFACE ( 'NONE', #408, 31.99999999999998579 ) ;
#30351 = EDGE_CURVE ( 'NONE', #28723, #39648, #42574, .T. ) ;
#30352 = FILL_AREA_STYLE_COLOUR ( '', #40569 ) ;
#30353 = DIRECTION ( 'NONE',  ( -0.08130631524010117905, 0.9966891607226784355, 0.000000000000000000 ) ) ;
#30354 = ORIENTED_EDGE ( 'NONE', *, *, #4953, .T. ) ;
#30355 = CIRCLE ( 'NONE', #14696, 32.00000000000000000 ) ;
#30356 = DIRECTION ( 'NONE',  ( 0.000000000000000000, -0.9876883405951394357, 0.1564344650402205716 ) ) ;
#30357 = EDGE_CURVE ( 'NONE', #15686, #22230, #28412, .T. ) ;
#30358 = AXIS2_PLACEMENT_3D ( 'NONE', #17377, #9324, #9807 ) ;
#30359 = EDGE_CURVE ( 'NONE', #39281, #46639, #36232, .T. ) ;
#30360 = DIRECTION ( 'NONE',  ( -0.000000000000000000, -0.000000000000000000, -1.000000000000000000 ) ) ;
#30361 = DIRECTION ( 'NONE',  ( 0.000000000000000000, -0.4539904997395352027, -0.8910065241883737830 ) ) ;
#30362 = AXIS2_PLACEMENT_3D ( 'NONE', #36852, #35895, #14355 ) ;
#30363 = ORIENTED_EDGE ( 'NONE', *, *, #1973, .T. ) ;
#30364 = ORIENTED_EDGE ( 'NONE', *, *, #30802, .T. ) ;
#30365 = CARTESIAN_POINT ( 'NONE',  ( 11.99999999999999822, 0.000000000000000000, 0.000000000000000000 ) ) ;
#30366 = VERTEX_POINT ( 'NONE', #27161 ) ;
#30367 = ORIENTED_EDGE ( 'NONE', *, *, #351, .T. ) ;
#30368 = EDGE_CURVE ( 'NONE', #2137, #29124, #47439, .T. ) ;
#30369 = VERTEX_POINT ( 'NONE', #28116 ) ;
#30370 = ORIENTED_EDGE ( 'NONE', *, *, #48028, .T. ) ;
#30371 = EDGE_LOOP ( 'NONE', ( #8994, #7297, #12561, #29626 ) ) ;
#30372 = AXIS2_PLACEMENT_3D ( 'NONE', #44377, #41203, #25521 ) ;
#30373 = VECTOR ( 'NONE', #20105, 1000.000000000000000 ) ;
#30374 = DIRECTION ( 'NONE',  ( 0.000000000000000000, 0.8090169943749504489, -0.5877852522924689183 ) ) ;
#30375 = ORIENTED_EDGE ( 'NONE', *, *, #7687, .F. ) ;
#30376 = VERTEX_POINT ( 'NONE', #46488 ) ;
#30377 = CARTESIAN_POINT ( 'NONE',  ( 0.000000000000000000, -73.95703589263958122, -23.16143007188506431 ) ) ;
#30378 = EDGE_LOOP ( 'NONE', ( #3947, #1252, #33490, #29020 ) ) ;
#30379 = DIRECTION ( 'NONE',  ( -1.000000000000000000, 0.000000000000000000, 0.000000000000000000 ) ) ;
#30380 = LINE ( 'NONE', #7372, #17362 ) ;
#30381 = VERTEX_POINT ( 'NONE', #20521 ) ;
#30382 = FACE_OUTER_BOUND ( 'NONE', #34382, .T. ) ;
#30383 = ORIENTED_EDGE ( 'NONE', *, *, #36575, .F. ) ;
#30385 = VERTEX_POINT ( 'NONE', #21007 ) ;
#30384 = DIRECTION ( 'NONE',  ( 0.000000000000000000, 0.000000000000000000, -1.000000000000000000 ) ) ;
#30386 = EDGE_CURVE ( 'NONE', #29705, #13671, #278, .T. ) ;
#30387 = CARTESIAN_POINT ( 'NONE',  ( 15.00000000000000000, 9.615535125378766423, -24.73947219025917121 ) ) ;
#30388 = ORIENTED_EDGE ( 'NONE', *, *, #42273, .T. ) ;
#30389 = CARTESIAN_POINT ( 'NONE',  ( 0.000000000000000000, 12.24744871391589207, 2.500000000000000000 ) ) ;
#30390 = VERTEX_POINT ( 'NONE', #35934 ) ;
#30391 = ORIENTED_EDGE ( 'NONE', *, *, #6303, .T. ) ;
#30392 = CARTESIAN_POINT ( 'NONE',  ( 0.000000000000000000, 16.61724383029390140, -20.69703378468904020 ) ) ;
#30393 = DIRECTION ( 'NONE',  ( 0.000000000000000000, -0.7071067811865389130, -0.7071067811865563435 ) ) ;
#30394 = EDGE_LOOP ( 'NONE', ( #43356, #20416, #16353, #23359 ) ) ;
#30395 = EDGE_CURVE ( 'NONE', #15125, #16632, #4212, .T. ) ;
#30396 = PLANE ( 'NONE',  #1206 ) ;
#30397 = DIRECTION ( 'NONE',  ( -0.000000000000000000, 0.000000000000000000, 1.000000000000000000 ) ) ;
#30398 = CARTESIAN_POINT ( 'NONE',  ( 0.000000000000000000, -29.01471420065506379, -76.69515212746047439 ) ) ;
#30399 = EDGE_CURVE ( 'NONE', #30212, #30126, #27649, .T. ) ;
#30400 = CARTESIAN_POINT ( 'NONE',  ( 10.00000000000000000, 35.53030884539102630, -12.26510123303222599 ) ) ;
#30401 = CARTESIAN_POINT ( 'NONE',  ( 10.00000000000000000, 0.000000000000000000, 0.000000000000000000 ) ) ;
#30402 = LINE ( 'NONE', #15468, #22394 ) ;
#30403 = DIRECTION ( 'NONE',  ( 0.000000000000000000, -0.000000000000000000, -1.000000000000000000 ) ) ;
#30404 = CARTESIAN_POINT ( 'NONE',  ( 15.00000000000000000, -14.54903810567676636, -22.19967320028755964 ) ) ;
#30405 = DIRECTION ( 'NONE',  ( -1.000000000000000000, -0.000000000000000000, -0.000000000000000000 ) ) ;
#30406 = DIRECTION ( 'NONE',  ( 0.9827303690289279636, 0.1850432970638682395, -0.000000000000000000 ) ) ;
#30407 = DIRECTION ( 'NONE',  ( -1.000000000000000000, -0.000000000000000000, -0.000000000000000000 ) ) ;
#30408 = CARTESIAN_POINT ( 'NONE',  ( 10.00000000000000000, -35.47612816024506088, -22.48208911017539435 ) ) ;
#30409 = EDGE_CURVE ( 'NONE', #36805, #28599, #13191, .T. ) ;
#30410 = DIRECTION ( 'NONE',  ( -1.000000000000000000, -0.000000000000000000, -0.000000000000000000 ) ) ;
#30411 = EDGE_CURVE ( 'NONE', #12511, #23540, #32045, .T. ) ;
#30412 = EDGE_CURVE ( 'NONE', #1469, #13012, #27903, .T. ) ;
#30413 = ORIENTED_EDGE ( 'NONE', *, *, #14596, .T. ) ;
#30414 = FACE_BOUND ( 'NONE', #13225, .T. ) ;
#30415 = ORIENTED_EDGE ( 'NONE', *, *, #4114, .T. ) ;
#30416 = DIRECTION ( 'NONE',  ( -1.000000000000000000, 0.000000000000000000, 0.000000000000000000 ) ) ;
#30417 = SHAPE_DEFINITION_REPRESENTATION ( #35474, #9091 ) ;
#30418 = CARTESIAN_POINT ( 'NONE',  ( 11.99999999999999822, 0.000000000000000000, 0.000000000000000000 ) ) ;
#30419 = EDGE_LOOP ( 'NONE', ( #42847, #14669, #10926, #46237 ) ) ;
#30420 = AXIS2_PLACEMENT_3D ( 'NONE', #8494, #18780, #44992 ) ;
#30421 = DIRECTION ( 'NONE',  ( -1.000000000000000000, 0.000000000000000000, 0.000000000000000000 ) ) ;
#30422 = CIRCLE ( 'NONE', #42935, 82.00000000000000000 ) ;
#30423 = ORIENTED_EDGE ( 'NONE', *, *, #48138, .F. ) ;
#30424 = AXIS2_PLACEMENT_3D ( 'NONE', #21390, #3027, #36329 ) ;
#30425 = CARTESIAN_POINT ( 'NONE',  ( 0.000000000000000000, -31.52238457039579345, -27.75498641678775158 ) ) ;
#30426 = LINE ( 'NONE', #22105, #39921 ) ;
#30428 = EDGE_LOOP ( 'NONE', ( #43842, #41394, #38198, #30868 ) ) ;
#30427 = DIRECTION ( 'NONE',  ( 0.4796670183876317051, -0.8774505977381971134, 0.000000000000000000 ) ) ;
#30429 = ORIENTED_EDGE ( 'NONE', *, *, #15522, .F. ) ;
#30430 = DIRECTION ( 'NONE',  ( -1.000000000000000000, 0.000000000000000000, -0.000000000000000000 ) ) ;
#30431 = CARTESIAN_POINT ( 'NONE',  ( -3.000000000000000000, -22.32062822937469804, -14.36278369418829826 ) ) ;
#30432 = EDGE_CURVE ( 'NONE', #46205, #44922, #6542, .T. ) ;
#30433 = FACE_OUTER_BOUND ( 'NONE', #45254, .T. ) ;
#30434 = COLOUR_RGB ( '', 0.31764706, 0.68627451, 0.89019608) ;
#30435 = DIRECTION ( 'NONE',  ( 0.8541291221503265474, -0.5200609990133007177, 0.000000000000000000 ) ) ;
#30436 = ADVANCED_FACE ( 'NONE', ( #32274 ), #36171, .T. ) ;
#30437 = ORIENTED_EDGE ( 'NONE', *, *, #29147, .T. ) ;
#30438 = LINE ( 'NONE', #16243, #38890 ) ;
#30439 = ORIENTED_EDGE ( 'NONE', *, *, #43592, .F. ) ;
#30440 = VERTEX_POINT ( 'NONE', #10229 ) ;
#30441 = CARTESIAN_POINT ( 'NONE',  ( 0.000000000000000000, -14.66109333815410487, -73.73191006444587003 ) ) ;
#30442 = ADVANCED_FACE ( 'NONE', ( #16868 ), #24920, .T. ) ;
#30443 = DIRECTION ( 'NONE',  ( -0.7071067811865474617, 0.000000000000000000, 0.7071067811865474617 ) ) ;
#30444 = CYLINDRICAL_SURFACE ( 'NONE', #35968, 82.00000000000000000 ) ;
#30445 = DIRECTION ( 'NONE',  ( -1.000000000000000000, -0.000000000000000000, 0.000000000000000000 ) ) ;
#30446 = VERTEX_POINT ( 'NONE', #28607 ) ;
#30447 = CARTESIAN_POINT ( 'NONE',  ( 11.99999999999999822, -62.50884508063453637, 41.76106447765467777 ) ) ;
#30448 = EDGE_CURVE ( 'NONE', #25278, #4532, #16678, .T. ) ;
#30449 = CARTESIAN_POINT ( 'NONE',  ( 5.000000000000000000, -15.48615015657555993, -39.04073710021360455 ) ) ;
#30450 = CARTESIAN_POINT ( 'NONE',  ( -10.00000000000000000, 0.000000000000000000, 0.000000000000000000 ) ) ;
#30451 = DIRECTION ( 'NONE',  ( 0.000000000000000000, 0.000000000000000000, 1.000000000000000000 ) ) ;
#30453 = VECTOR ( 'NONE', #40212, 1000.000000000000000 ) ;
#30452 = CARTESIAN_POINT ( 'NONE',  ( 0.000000000000000000, -59.46389618801929089, -49.70050353004953081 ) ) ;
#30454 = AXIS2_PLACEMENT_3D ( 'NONE', #24642, #20239, #39590 ) ;
#30455 = CARTESIAN_POINT ( 'NONE',  ( 11.99999999999999822, 75.11764819372149304, -2.946379043146603482 ) ) ;
#30456 = DIRECTION ( 'NONE',  ( -1.000000000000000000, 0.000000000000000000, 0.000000000000000000 ) ) ;
#30457 = FACE_OUTER_BOUND ( 'NONE', #46525, .T. ) ;
#30458 = CIRCLE ( 'NONE', #43761, 82.00000000000000000 ) ;
#30459 = DIRECTION ( 'NONE',  ( -1.000000000000000000, -0.000000000000000000, -0.000000000000000000 ) ) ;
#30460 = CARTESIAN_POINT ( 'NONE',  ( -3.000000000000000000, 23.50000000000000000, 1.499999999999997780 ) ) ;
#30461 = ADVANCED_FACE ( 'NONE', ( #43050 ), #21493, .F. ) ;
#30462 = EDGE_CURVE ( 'NONE', #9384, #6289, #1693, .T. ) ;
#30463 = PLANE ( 'NONE',  #17639 ) ;
#30464 = ORIENTED_EDGE ( 'NONE', *, *, #40304, .F. ) ;
#30465 = DIRECTION ( 'NONE',  ( -1.000000000000000000, 0.000000000000000000, -0.000000000000000000 ) ) ;
#30466 = PLANE ( 'NONE',  #30838 ) ;
#30467 = CIRCLE ( 'NONE', #42980, 12.49999999999999822 ) ;
#30468 = CYLINDRICAL_SURFACE ( 'NONE', #34860, 16.00000000000000000 ) ;
#30469 = ORIENTED_EDGE ( 'NONE', *, *, #22006, .T. ) ;
#30470 = DIRECTION ( 'NONE',  ( 0.000000000000000000, 0.000000000000000000, 1.000000000000000000 ) ) ;
#30471 = ORIENTED_EDGE ( 'NONE', *, *, #10893, .F. ) ;
#30472 = EDGE_CURVE ( 'NONE', #20366, #45561, #1826, .T. ) ;
#30473 = EDGE_LOOP ( 'NONE', ( #8059, #2639, #39097, #1575 ) ) ;
#30474 = ORIENTED_EDGE ( 'NONE', *, *, #39145, .F. ) ;
#30475 = DIRECTION ( 'NONE',  ( -1.000000000000000000, -0.000000000000000000, 0.000000000000000000 ) ) ;
#30476 = ORIENTED_EDGE ( 'NONE', *, *, #18405, .F. ) ;
#30477 = FACE_OUTER_BOUND ( 'NONE', #13976, .T. ) ;
#30478 = CIRCLE ( 'NONE', #38303, 16.00000000000000355 ) ;
#30479 = LINE ( 'NONE', #33428, #21845 ) ;
#30480 = DIRECTION ( 'NONE',  ( 1.000000000000000000, 0.000000000000000000, -0.000000000000000000 ) ) ;
#30481 = VECTOR ( 'NONE', #11753, 1000.000000000000000 ) ;
#30482 = ORIENTED_EDGE ( 'NONE', *, *, #41234, .F. ) ;
#30483 = DIRECTION ( 'NONE',  ( 0.000000000000000000, 0.9238795325112851842, 0.3826834323650937786 ) ) ;
#30484 = ORIENTED_EDGE ( 'NONE', *, *, #25614, .T. ) ;
#30485 = VECTOR ( 'NONE', #14373, 1000.000000000000000 ) ;
#30486 = DIRECTION ( 'NONE',  ( 0.000000000000000000, -0.1564344650402382242, 0.9876883405951366601 ) ) ;
#30487 = CARTESIAN_POINT ( 'NONE',  ( 11.99999999999999822, -80.28980883073745645, -16.65972982745018172 ) ) ;
#30488 = ORIENTED_EDGE ( 'NONE', *, *, #39829, .T. ) ;
#30489 = ORIENTED_EDGE ( 'NONE', *, *, #6612, .F. ) ;
#30490 = CIRCLE ( 'NONE', #7039, 32.50000000000000000 ) ;
#30491 = CARTESIAN_POINT ( 'NONE',  ( 10.00000000000000000, 0.000000000000000000, 0.000000000000000000 ) ) ;
#30492 = EDGE_LOOP ( 'NONE', ( #29320, #4364, #9991, #27197 ) ) ;
#30493 = FACE_OUTER_BOUND ( 'NONE', #15860, .T. ) ;
#30494 = ADVANCED_FACE ( 'NONE', ( #16614 ), #39135, .T. ) ;
#30495 = CARTESIAN_POINT ( 'NONE',  ( 10.00000000000000000, 33.79645857604513992, 16.45098606841138178 ) ) ;
#30496 = DIRECTION ( 'NONE',  ( 0.000000000000000000, 0.000000000000000000, 1.000000000000000000 ) ) ;
#30497 = CARTESIAN_POINT ( 'NONE',  ( 0.000000000000000000, 0.000000000000000000, 0.000000000000000000 ) ) ;
#30498 = CARTESIAN_POINT ( 'NONE',  ( -10.00000000000000000, 0.000000000000000000, 0.000000000000000000 ) ) ;
#30499 = DIRECTION ( 'NONE',  ( -1.000000000000000000, 0.000000000000000000, 0.000000000000000000 ) ) ;
#30500 = EDGE_CURVE ( 'NONE', #956, #28068, #1081, .T. ) ;
#30501 = DIRECTION ( 'NONE',  ( -1.000000000000000000, 0.000000000000000000, -0.000000000000000000 ) ) ;
#30502 = EDGE_LOOP ( 'NONE', ( #26129, #19801, #31099, #11307 ) ) ;
#30503 = CARTESIAN_POINT ( 'NONE',  ( 19.29194287201271862, -133.5026271600380880, 2.500000000000000000 ) ) ;
#30504 = PLANE ( 'NONE',  #42567 ) ;
#30505 = EDGE_LOOP ( 'NONE', ( #11068, #28025, #6035, #13968 ) ) ;
#30506 = CARTESIAN_POINT ( 'NONE',  ( 0.000000000000000000, -71.27951684758045303, 30.41916302227090085 ) ) ;
#30507 = DIRECTION ( 'NONE',  ( -1.000000000000000000, 0.000000000000000000, -0.000000000000000000 ) ) ;
#30508 = ORIENTED_EDGE ( 'NONE', *, *, #17706, .T. ) ;
#30509 = VERTEX_POINT ( 'NONE', #39634 ) ;
#30510 = EDGE_CURVE ( 'NONE', #11988, #45060, #11263, .T. ) ;
#30511 = FACE_OUTER_BOUND ( 'NONE', #47157, .T. ) ;
#30512 = DIRECTION ( 'NONE',  ( -1.000000000000000000, -0.000000000000000000, -0.000000000000000000 ) ) ;
#30513 = CARTESIAN_POINT ( 'NONE',  ( 10.00000000000000000, 0.000000000000000000, 0.000000000000000000 ) ) ;
#30514 = CARTESIAN_POINT ( 'NONE',  ( -20.30386590532152979, -102.9045904027214959, 5.500000000000000000 ) ) ;
#30515 = EDGE_CURVE ( 'NONE', #45549, #5995, #13599, .T. ) ;
#30516 = CARTESIAN_POINT ( 'NONE',  ( 11.99999999999999822, -11.30684508768393748, 76.66974797899833050 ) ) ;
#30517 = DIRECTION ( 'NONE',  ( -1.000000000000000000, 0.000000000000000000, -0.000000000000000000 ) ) ;
#30518 = AXIS2_PLACEMENT_3D ( 'NONE', #45178, #16044, #4311 ) ;
#30519 = VERTEX_POINT ( 'NONE', #37145 ) ;
#30520 = CARTESIAN_POINT ( 'NONE',  ( 10.00000000000000000, -46.21855187248673502, 62.20884554314003623 ) ) ;
#30521 = CARTESIAN_POINT ( 'NONE',  ( 11.99999999999999822, 73.44644590900094272, -24.73286445877629802 ) ) ;
#30522 = VECTOR ( 'NONE', #47510, 1000.000000000000000 ) ;
#30523 = ADVANCED_FACE ( 'NONE', ( #22467 ), #10956, .F. ) ;
#30524 = AXIS2_PLACEMENT_3D ( 'NONE', #24352, #9663, #24609 ) ;
#30525 = CARTESIAN_POINT ( 'NONE',  ( 0.000000000000000000, -46.11716303203136391, -67.80270845531939017 ) ) ;
#30526 = VECTOR ( 'NONE', #43374, 1000.000000000000000 ) ;
#30527 = VERTEX_POINT ( 'NONE', #7275 ) ;
#30528 = EDGE_CURVE ( 'NONE', #7347, #31342, #47904, .T. ) ;
#30529 = AXIS2_PLACEMENT_3D ( 'NONE', #46272, #20306, #12742 ) ;
#30530 = ORIENTED_EDGE ( 'NONE', *, *, #9724, .T. ) ;
#30531 = ORIENTED_EDGE ( 'NONE', *, *, #36786, .T. ) ;
#30532 = CARTESIAN_POINT ( 'NONE',  ( 11.99999999999999822, 71.91182617369190666, 28.89263327155770966 ) ) ;
#30533 = CARTESIAN_POINT ( 'NONE',  ( 0.000000000000000000, 0.000000000000000000, 0.000000000000000000 ) ) ;
#30534 = ORIENTED_EDGE ( 'NONE', *, *, #37365, .T. ) ;
#30535 = LINE ( 'NONE', #7549, #48398 ) ;
#30536 = VERTEX_POINT ( 'NONE', #18542 ) ;
#30537 = CARTESIAN_POINT ( 'NONE',  ( 10.00000000000000000, -6.555932627142676772, 37.01155633439056203 ) ) ;
#30538 = DIRECTION ( 'NONE',  ( 0.000000000000000000, -0.9510565162951502005, -0.3090169943749581094 ) ) ;
#30539 = CIRCLE ( 'NONE', #14129, 12.49999999999999822 ) ;
#30540 = DIRECTION ( 'NONE',  ( 0.000000000000000000, -0.2079116908177671419, 0.9781476007338040235 ) ) ;
#30542 = ORIENTED_EDGE ( 'NONE', *, *, #16317, .T. ) ;
#30541 = VECTOR ( 'NONE', #24651, 1000.000000000000114 ) ;
#30543 = CARTESIAN_POINT ( 'NONE',  ( 5.999999999999999112, 63.97538442413426907, 51.29473840253246664 ) ) ;
#30544 = ORIENTED_EDGE ( 'NONE', *, *, #33102, .F. ) ;
#30545 = ORIENTED_EDGE ( 'NONE', *, *, #16114, .F. ) ;
#30546 = EDGE_CURVE ( 'NONE', #17177, #30774, #14150, .T. ) ;
#30547 = CARTESIAN_POINT ( 'NONE',  ( 11.99999999999999822, 0.000000000000000000, 0.000000000000000000 ) ) ;
#30548 = AXIS2_PLACEMENT_3D ( 'NONE', #33394, #48314, #44646 ) ;
#30549 = AXIS2_PLACEMENT_3D ( 'NONE', #37648, #29577, #37406 ) ;
#30550 = EDGE_CURVE ( 'NONE', #913, #35715, #17503, .T. ) ;
#30551 = DIRECTION ( 'NONE',  ( -1.000000000000000000, 0.000000000000000000, 0.000000000000000000 ) ) ;
#30552 = DIRECTION ( 'NONE',  ( -1.000000000000000000, -0.000000000000000000, 0.000000000000000000 ) ) ;
#30553 = ORIENTED_EDGE ( 'NONE', *, *, #2127, .F. ) ;
#30554 = EDGE_CURVE ( 'NONE', #17275, #45171, #44865, .T. ) ;
#30555 = AXIS2_PLACEMENT_3D ( 'NONE', #30387, #23030, #11544 ) ;
#30556 = VERTEX_POINT ( 'NONE', #14875 ) ;
#30557 = CIRCLE ( 'NONE', #29015, 31.99999999999998579 ) ;
#30558 = DIRECTION ( 'NONE',  ( 0.3853207896976533209, -0.9227826878668545785, 0.000000000000000000 ) ) ;
#30559 = DIRECTION ( 'NONE',  ( -1.000000000000000000, -0.000000000000000000, 0.000000000000000000 ) ) ;
#30561 = ADVANCED_FACE ( 'NONE', ( #44724 ), #36650, .F. ) ;
#30560 = VERTEX_POINT ( 'NONE', #36883 ) ;
#30562 = EDGE_CURVE ( 'NONE', #8858, #13574, #40194, .T. ) ;
#30563 = PLANE ( 'NONE',  #21263 ) ;
#30564 = ORIENTED_EDGE ( 'NONE', *, *, #5747, .T. ) ;
#30565 = DIRECTION ( 'NONE',  ( -1.000000000000000000, 0.000000000000000000, 0.000000000000000000 ) ) ;
#30566 = DIRECTION ( 'NONE',  ( 1.000000000000000000, 0.000000000000000000, 0.000000000000000000 ) ) ;
#30567 = FACE_OUTER_BOUND ( 'NONE', #37575, .T. ) ;
#30568 = DIRECTION ( 'NONE',  ( 0.000000000000000000, -0.3090169943749548342, 0.9510565162951511997 ) ) ;
#30569 = DIRECTION ( 'NONE',  ( 0.000000000000000000, 0.000000000000000000, -1.000000000000000000 ) ) ;
#30570 = DIRECTION ( 'NONE',  ( -0.2306669878475648139, -0.9730327541852491491, 0.000000000000000000 ) ) ;
#30571 = CARTESIAN_POINT ( 'NONE',  ( 10.00000000000000000, -41.19522573413780009, 65.64334221924896440 ) ) ;
#30572 = FACE_OUTER_BOUND ( 'NONE', #18636, .T. ) ;
#30573 = DIRECTION ( 'NONE',  ( -1.000000000000000000, -0.000000000000000000, -0.000000000000000000 ) ) ;
#30574 = ORIENTED_EDGE ( 'NONE', *, *, #46085, .T. ) ;
#30575 = DIRECTION ( 'NONE',  ( -0.7273375899149793211, 0.6862798483830554463, 0.000000000000000000 ) ) ;
#30576 = DIRECTION ( 'NONE',  ( 0.000000000000000000, 0.000000000000000000, 1.000000000000000000 ) ) ;
#30577 = PLANE ( 'NONE',  #42848 ) ;
#30578 = ORIENTED_EDGE ( 'NONE', *, *, #19603, .F. ) ;
#30579 = AXIS2_PLACEMENT_3D ( 'NONE', #30633, #41905, #8357 ) ;
#30580 = EDGE_CURVE ( 'NONE', #8066, #28131, #46443, .T. ) ;
#30581 = CIRCLE ( 'NONE', #32913, 37.49900000000000944 ) ;
#30582 = UNCERTAINTY_MEASURE_WITH_UNIT (LENGTH_MEASURE( 1.000000000000000082E-05 ), #38116, 'distance_accuracy_value', 'NONE');
#30583 = CARTESIAN_POINT ( 'NONE',  ( -32.50000000000000000, -120.0000000000000000, 2.500000000000000000 ) ) ;
#30584 = VECTOR ( 'NONE', #35243, 1000.000000000000000 ) ;
#30585 = CIRCLE ( 'NONE', #16548, 82.00000000000000000 ) ;
#30586 = DIRECTION ( 'NONE',  ( -1.000000000000000000, -0.000000000000000000, -0.000000000000000000 ) ) ;
#30587 = ADVANCED_FACE ( 'NONE', ( #7536 ), #29324, .T. ) ;
#30588 = CYLINDRICAL_SURFACE ( 'NONE', #8134, 82.00000000000000000 ) ;
#30589 = ORIENTED_EDGE ( 'NONE', *, *, #32861, .F. ) ;
#30590 = CIRCLE ( 'NONE', #1668, 16.00000000000000355 ) ;
#30591 = AXIS2_PLACEMENT_3D ( 'NONE', #41589, #48203, #22002 ) ;
#30592 = EDGE_LOOP ( 'NONE', ( #38946, #13832, #13947, #4618 ) ) ;
#30593 = ADVANCED_FACE ( 'NONE', ( #41309 ), #32979, .F. ) ;
#30594 = PLANE ( 'NONE',  #7033 ) ;
#30595 = VECTOR ( 'NONE', #13455, 1000.000000000000114 ) ;
#30596 = ORIENTED_EDGE ( 'NONE', *, *, #8418, .F. ) ;
#30597 = ORIENTED_EDGE ( 'NONE', *, *, #14653, .F. ) ;
#30598 = ORIENTED_EDGE ( 'NONE', *, *, #32493, .T. ) ;
#30599 = ORIENTED_EDGE ( 'NONE', *, *, #45150, .F. ) ;
#30600 = VECTOR ( 'NONE', #37002, 1000.000000000000227 ) ;
#30601 = DIRECTION ( 'NONE',  ( 0.000000000000000000, -0.4539904997395542430, 0.8910065241883641241 ) ) ;
#30602 = EDGE_LOOP ( 'NONE', ( #32039, #47868, #13663, #24816 ) ) ;
#30603 = LINE ( 'NONE', #31350, #22355 ) ;
#30604 = ORIENTED_EDGE ( 'NONE', *, *, #22151, .T. ) ;
#30605 = EDGE_CURVE ( 'NONE', #15986, #37774, #17810, .T. ) ;
#30606 = CARTESIAN_POINT ( 'NONE',  ( 10.00000000000000000, 63.97538442413500093, -51.29473840253157135 ) ) ;
#30607 = ORIENTED_EDGE ( 'NONE', *, *, #10679, .T. ) ;
#30608 = LINE ( 'NONE', #23499, #5140 ) ;
#30609 = EDGE_CURVE ( 'NONE', #20108, #6477, #7338, .T. ) ;
#30610 = DIRECTION ( 'NONE',  ( -1.000000000000000000, -0.000000000000000000, -0.000000000000000000 ) ) ;
#30611 = VERTEX_POINT ( 'NONE', #21730 ) ;
#30612 = DIRECTION ( 'NONE',  ( 0.000000000000000000, 0.000000000000000000, 1.000000000000000000 ) ) ;
#30613 = ORIENTED_EDGE ( 'NONE', *, *, #12520, .T. ) ;
#30614 = VECTOR ( 'NONE', #36877, 1000.000000000000000 ) ;
#30615 = DIRECTION ( 'NONE',  ( -1.000000000000000000, -0.000000000000000000, -0.000000000000000000 ) ) ;
#30616 = LINE ( 'NONE', #34509, #14903 ) ;
#30617 = ORIENTED_EDGE ( 'NONE', *, *, #42987, .T. ) ;
#30618 = VECTOR ( 'NONE', #32650, 1000.000000000000114 ) ;
#30619 = LINE ( 'NONE', #41891, #1391 ) ;
#30620 = ORIENTED_EDGE ( 'NONE', *, *, #18720, .T. ) ;
#30621 = VERTEX_POINT ( 'NONE', #3111 ) ;
#30622 = EDGE_CURVE ( 'NONE', #2200, #5341, #3416, .T. ) ;
#30623 = DIRECTION ( 'NONE',  ( -0.000000000000000000, -0.000000000000000000, -1.000000000000000000 ) ) ;
#30624 = FACE_OUTER_BOUND ( 'NONE', #30502, .T. ) ;
#30625 = AXIS2_PLACEMENT_3D ( 'NONE', #516, #26460, #15211 ) ;
#30626 = DIRECTION ( 'NONE',  ( -1.000000000000000000, 0.000000000000000000, 0.000000000000000000 ) ) ;
#30627 = EDGE_CURVE ( 'NONE', #20927, #28215, #19838, .T. ) ;
#30628 = DIRECTION ( 'NONE',  ( 0.000000000000000000, 0.000000000000000000, -1.000000000000000000 ) ) ;
#30629 = DIRECTION ( 'NONE',  ( 0.000000000000000000, 0.000000000000000000, 1.000000000000000000 ) ) ;
#30630 = CIRCLE ( 'NONE', #15661, 31.99999999999999289 ) ;
#30631 = DIRECTION ( 'NONE',  ( 0.000000000000000000, 0.000000000000000000, 1.000000000000000000 ) ) ;
#30632 = CIRCLE ( 'NONE', #42332, 82.00000000000000000 ) ;
#30633 = CARTESIAN_POINT ( 'NONE',  ( 0.000000000000000000, -37.01155633439063308, 6.555932627142289526 ) ) ;
#30634 = CYLINDRICAL_SURFACE ( 'NONE', #3656, 31.99999999999998579 ) ;
#30635 = ORIENTED_EDGE ( 'NONE', *, *, #25627, .T. ) ;
#30636 = DIRECTION ( 'NONE',  ( 0.000000000000000000, 0.000000000000000000, 1.000000000000000000 ) ) ;
#30637 = DIRECTION ( 'NONE',  ( -1.000000000000000000, 0.000000000000000000, 0.000000000000000000 ) ) ;
#30638 = DIRECTION ( 'NONE',  ( -1.000000000000000000, -0.000000000000000000, -0.000000000000000000 ) ) ;
#30639 = ORIENTED_EDGE ( 'NONE', *, *, #10779, .T. ) ;
#30640 = VECTOR ( 'NONE', #31291, 1000.000000000000000 ) ;
#30641 = CYLINDRICAL_SURFACE ( 'NONE', #32292, 16.00000000000000000 ) ;
#30642 = DIRECTION ( 'NONE',  ( -1.000000000000000000, -0.000000000000000000, 0.000000000000000000 ) ) ;
#30643 = CARTESIAN_POINT ( 'NONE',  ( 16.30584220631899228, -140.9432449716519784, 2.500000000000000000 ) ) ;
#30644 = DIRECTION ( 'NONE',  ( -1.000000000000000000, -0.000000000000000000, 0.000000000000000000 ) ) ;
#30645 = ORIENTED_EDGE ( 'NONE', *, *, #13295, .F. ) ;
#30646 = ORIENTED_EDGE ( 'NONE', *, *, #19269, .T. ) ;
#30647 = CARTESIAN_POINT ( 'NONE',  ( 0.000000000000000000, -16.23288003029521320, 33.80338159004277543 ) ) ;
#30648 = VERTEX_POINT ( 'NONE', #14642 ) ;
#30649 = DIRECTION ( 'NONE',  ( -1.000000000000000000, 0.000000000000000000, 0.000000000000000000 ) ) ;
#30650 = PRODUCT_CONTEXT ( 'NONE', #22579, 'mechanical' ) ;
#30651 = DIRECTION ( 'NONE',  ( 0.000000000000000000, -6.938893903907228378E-15, 1.000000000000000000 ) ) ;
#30652 = ORIENTED_EDGE ( 'NONE', *, *, #7714, .T. ) ;
#30653 = AXIS2_PLACEMENT_3D ( 'NONE', #37555, #22623, #33406 ) ;
#30654 = AXIS2_PLACEMENT_3D ( 'NONE', #31844, #32072, #42603 ) ;
#30655 = EDGE_CURVE ( 'NONE', #27838, #16956, #37627, .T. ) ;
#30656 = DIRECTION ( 'NONE',  ( 1.000000000000000000, 0.000000000000000000, -0.000000000000000000 ) ) ;
#30657 = ORIENTED_EDGE ( 'NONE', *, *, #37072, .F. ) ;
#30658 = CIRCLE ( 'NONE', #4077, 16.00000000000000000 ) ;
#30659 = FACE_OUTER_BOUND ( 'NONE', #29507, .T. ) ;
#30660 = CARTESIAN_POINT ( 'NONE',  ( 10.00000000000000000, 30.00120703465236716, -22.64427369931138756 ) ) ;
#30662 = VERTEX_POINT ( 'NONE', #24089 ) ;
#30661 = DIRECTION ( 'NONE',  ( 0.000000000000000000, -0.8910065241883722287, 0.4539904997395383113 ) ) ;
#30663 = ORIENTED_EDGE ( 'NONE', *, *, #18822, .T. ) ;
#30664 = EDGE_CURVE ( 'NONE', #43729, #48169, #6573, .T. ) ;
#30665 = ORIENTED_EDGE ( 'NONE', *, *, #28014, .T. ) ;
#30666 = ADVANCED_FACE ( 'NONE', ( #5254 ), #9156, .T. ) ;
#30667 = EDGE_CURVE ( 'NONE', #37239, #46298, #25322, .T. ) ;
#30668 = DIRECTION ( 'NONE',  ( -1.000000000000000000, -0.000000000000000000, 0.000000000000000000 ) ) ;
#30669 = DIRECTION ( 'NONE',  ( -1.000000000000000000, -0.000000000000000000, 0.000000000000000000 ) ) ;
#30670 = DIRECTION ( 'NONE',  ( -1.000000000000000000, -0.000000000000000000, -0.000000000000000000 ) ) ;
#30671 = DIRECTION ( 'NONE',  ( -0.000000000000000000, -0.000000000000000000, -1.000000000000000000 ) ) ;
#30672 = EDGE_LOOP ( 'NONE', ( #29856, #32948, #5944, #27020 ) ) ;
#30673 = DIRECTION ( 'NONE',  ( 0.000000000000000000, 0.7431448254773878048, -0.6691306063588654540 ) ) ;
#30674 = VERTEX_POINT ( 'NONE', #46355 ) ;
#30675 = ORIENTED_EDGE ( 'NONE', *, *, #45586, .F. ) ;
#30676 = ADVANCED_FACE ( 'NONE', ( #5486 ), #8654, .F. ) ;
#30677 = DIRECTION ( 'NONE',  ( 0.000000000000000000, 0.000000000000000000, 1.000000000000000000 ) ) ;
#30678 = ORIENTED_EDGE ( 'NONE', *, *, #31510, .T. ) ;
#30679 = AXIS2_PLACEMENT_3D ( 'NONE', #15879, #26418, #37425 ) ;
#30680 = LINE ( 'NONE', #26529, #47285 ) ;
#30681 = ADVANCED_FACE ( 'NONE', ( #5002 ), #16746, .T. ) ;
#30682 = DIRECTION ( 'NONE',  ( 0.000000000000000000, 0.000000000000000000, 1.000000000000000000 ) ) ;
#30683 = CARTESIAN_POINT ( 'NONE',  ( 5.999999999999999112, -67.80270845531921964, 46.11716303203162681 ) ) ;
#30684 = ORIENTED_EDGE ( 'NONE', *, *, #19235, .F. ) ;
#30685 = CARTESIAN_POINT ( 'NONE',  ( 23.11608002360578240, -124.4885236261218182, 5.500000000000000000 ) ) ;
#30686 = LINE ( 'NONE', #1319, #34625 ) ;
#30687 = CARTESIAN_POINT ( 'NONE',  ( 0.000000000000000000, 23.16143007188532366, -73.95703589263949596 ) ) ;
#30688 = CIRCLE ( 'NONE', #200, 31.99999999999997868 ) ;
#30689 = CARTESIAN_POINT ( 'NONE',  ( 11.99999999999999822, 26.02418014898407961, -70.52718814184231633 ) ) ;
#30690 = DIRECTION ( 'NONE',  ( -1.000000000000000000, 0.000000000000000000, 0.000000000000000000 ) ) ;
#30691 = DIRECTION ( 'NONE',  ( 0.000000000000000000, 0.3826834323650904479, -0.9238795325112865164 ) ) ;
#30692 = CARTESIAN_POINT ( 'NONE',  ( 10.00000000000000000, 0.000000000000000000, 0.000000000000000000 ) ) ;
#30693 = CARTESIAN_POINT ( 'NONE',  ( 10.00000000000000000, -33.17418723428294669, -17.67226234102862747 ) ) ;
#30694 = ADVANCED_FACE ( 'NONE', ( #24324 ), #12590, .T. ) ;
#30695 = AXIS2_PLACEMENT_3D ( 'NONE', #1918, #24410, #12934 ) ;
#30696 = CARTESIAN_POINT ( 'NONE',  ( 10.00000000000000000, 0.8828120875900632436, 37.48860685352291000 ) ) ;
#30697 = LINE ( 'NONE', #42192, #41710 ) ;
#30698 = AXIS2_PLACEMENT_3D ( 'NONE', #3159, #24078, #43407 ) ;
#30699 = EDGE_LOOP ( 'NONE', ( #15843, #8557, #18141, #5236 ) ) ;
#30700 = CARTESIAN_POINT ( 'NONE',  ( 10.00000000000000000, 17.80606268964540462, 33.00180498840053644 ) ) ;
#30701 = ORIENTED_EDGE ( 'NONE', *, *, #14392, .F. ) ;
#30702 = CARTESIAN_POINT ( 'NONE',  ( 11.99999999999999822, 0.000000000000000000, 0.000000000000000000 ) ) ;
#30703 = DIRECTION ( 'NONE',  ( -1.000000000000000000, 0.000000000000000000, 0.000000000000000000 ) ) ;
#30704 = VECTOR ( 'NONE', #39554, 1000.000000000000000 ) ;
#30705 = ORIENTED_EDGE ( 'NONE', *, *, #949, .F. ) ;
#30706 = ORIENTED_EDGE ( 'NONE', *, *, #21771, .F. ) ;
#30707 = CIRCLE ( 'NONE', #4157, 82.00000000000000000 ) ;
#30708 = CARTESIAN_POINT ( 'NONE',  ( 10.00000000000000000, 0.000000000000000000, 0.000000000000000000 ) ) ;
#30709 = ORIENTED_EDGE ( 'NONE', *, *, #35136, .F. ) ;
#30710 = EDGE_CURVE ( 'NONE', #30299, #10059, #28010, .T. ) ;
#30711 = EDGE_CURVE ( 'NONE', #35361, #14109, #42447, .T. ) ;
#30712 = ORIENTED_EDGE ( 'NONE', *, *, #16202, .T. ) ;
#30713 = EDGE_CURVE ( 'NONE', #17850, #1046, #47966, .T. ) ;
#30714 = EDGE_LOOP ( 'NONE', ( #19274, #1762, #47309, #28627 ) ) ;
#30715 = CARTESIAN_POINT ( 'NONE',  ( 5.999999999999999112, 68.55367621811141987, 44.99326035066079044 ) ) ;
#30716 = VECTOR ( 'NONE', #25758, 1000.000000000000227 ) ;
#30717 = ORIENTED_EDGE ( 'NONE', *, *, #41853, .F. ) ;
#30718 = EDGE_CURVE ( 'NONE', #35674, #45129, #20167, .T. ) ;
#30719 = ORIENTED_EDGE ( 'NONE', *, *, #40716, .F. ) ;
#30720 = CIRCLE ( 'NONE', #4133, 77.49900000000000944 ) ;
#30721 = AXIS2_PLACEMENT_3D ( 'NONE', #17132, #42616, #24481 ) ;
#30722 = DIRECTION ( 'NONE',  ( -1.000000000000000000, 0.000000000000000000, 0.000000000000000000 ) ) ;
#30723 = APPLICATION_CONTEXT ( 'automotive_design' ) ;
#30724 = DIRECTION ( 'NONE',  ( -1.000000000000000000, -0.000000000000000000, 0.000000000000000000 ) ) ;
#30725 = CIRCLE ( 'NONE', #45566, 37.49900000000000944 ) ;
#30726 = CIRCLE ( 'NONE', #20656, 31.99999999999998579 ) ;
#30728 = ORIENTED_EDGE ( 'NONE', *, *, #36951, .T. ) ;
#30727 = DIRECTION ( 'NONE',  ( -1.000000000000000000, -0.000000000000000000, -0.000000000000000000 ) ) ;
#30729 = EDGE_LOOP ( 'NONE', ( #41257, #2598, #29395, #16715 ) ) ;
#30730 = DIRECTION ( 'NONE',  ( -1.000000000000000000, 0.000000000000000000, 0.000000000000000000 ) ) ;
#30731 = VECTOR ( 'NONE', #48371, 1000.000000000000000 ) ;
#30732 = ORIENTED_EDGE ( 'NONE', *, *, #77, .F. ) ;
#30733 = AXIS2_PLACEMENT_3D ( 'NONE', #34715, #9260, #46229 ) ;
#30734 = ORIENTED_EDGE ( 'NONE', *, *, #12362, .T. ) ;
#30735 = ADVANCED_FACE ( 'NONE', ( #13313 ), #43173, .T. ) ;
#30736 = ADVANCED_FACE ( 'NONE', ( #15370 ), #23593, .T. ) ;
#30737 = LINE ( 'NONE', #38082, #35033 ) ;
#30738 = CARTESIAN_POINT ( 'NONE',  ( 0.000000000000000000, 0.000000000000000000, 0.000000000000000000 ) ) ;
#30739 = AXIS2_PLACEMENT_3D ( 'NONE', #19650, #4276, #30948 ) ;
#30740 = VERTEX_POINT ( 'NONE', #19919 ) ;
#30741 = ORIENTED_EDGE ( 'NONE', *, *, #13635, .T. ) ;
#30742 = PLANE ( 'NONE',  #42764 ) ;
#30743 = EDGE_LOOP ( 'NONE', ( #39896, #19498, #34940 ) ) ;
#30744 = CYLINDRICAL_SURFACE ( 'NONE', #36364, 31.99999999999998579 ) ;
#30745 = CARTESIAN_POINT ( 'NONE',  ( 11.99999999999999822, 62.50329211542435104, 41.76937507738811917 ) ) ;
#30746 = CARTESIAN_POINT ( 'NONE',  ( 0.000000000000000000, 46.54456581323888997, -59.03342792756214408 ) ) ;
#30747 = DIRECTION ( 'NONE',  ( -0.1850432970638656582, 0.9827303690289285187, 0.000000000000000000 ) ) ;
#30748 = CARTESIAN_POINT ( 'NONE',  ( 10.00000000000000000, 0.000000000000000000, 0.000000000000000000 ) ) ;
#30749 = CARTESIAN_POINT ( 'NONE',  ( -15.44521549751111422, -137.7748507232956001, 5.500000000000000000 ) ) ;
#30750 = CARTESIAN_POINT ( 'NONE',  ( -3.000000000000000000, -22.67460108101783334, 6.353146135317912169 ) ) ;
#30751 = ORIENTED_EDGE ( 'NONE', *, *, #10008, .T. ) ;
#30753 = EDGE_CURVE ( 'NONE', #29847, #41101, #16712, .T. ) ;
#30752 = DIRECTION ( 'NONE',  ( 0.000000000000000000, 0.000000000000000000, 1.000000000000000000 ) ) ;
#30754 = DIRECTION ( 'NONE',  ( -1.000000000000000000, 0.000000000000000000, 0.000000000000000000 ) ) ;
#30755 = DIRECTION ( 'NONE',  ( -1.000000000000000000, 0.000000000000000000, 0.000000000000000000 ) ) ;
#30756 = EDGE_LOOP ( 'NONE', ( #6358, #39470, #10199, #24116 ) ) ;
#30757 = EDGE_LOOP ( 'NONE', ( #1043, #15013, #21875, #6351 ) ) ;
#30758 = CARTESIAN_POINT ( 'NONE',  ( 10.00000000000000000, 0.000000000000000000, 0.000000000000000000 ) ) ;
#30759 = CARTESIAN_POINT ( 'NONE',  ( 0.000000000000000000, -10.45096189432344147, 21.10159698893425784 ) ) ;
#30760 = LINE ( 'NONE', #4092, #33714 ) ;
#30761 = CARTESIAN_POINT ( 'NONE',  ( 5.000000000000000000, 27.74655509720669500, 77.16300072079670258 ) ) ;
#30762 = DIRECTION ( 'NONE',  ( -1.000000000000000000, -0.000000000000000000, -0.000000000000000000 ) ) ;
#30764 = AXIS2_PLACEMENT_3D ( 'NONE', #22744, #3409, #3665 ) ;
#30763 = DIRECTION ( 'NONE',  ( 0.000000000000000000, 0.3090169943749482839, -0.9510565162951533091 ) ) ;
#30765 = VERTEX_POINT ( 'NONE', #31203 ) ;
#30766 = DIRECTION ( 'NONE',  ( -1.000000000000000000, 0.000000000000000000, 0.000000000000000000 ) ) ;
#30767 = FACE_OUTER_BOUND ( 'NONE', #3809, .T. ) ;
#30768 = CIRCLE ( 'NONE', #19799, 15.99999999999999645 ) ;
#30769 = AXIS2_PLACEMENT_3D ( 'NONE', #7617, #45067, #33554 ) ;
#30770 = VECTOR ( 'NONE', #8976, 1000.000000000000000 ) ;
#30771 = ORIENTED_EDGE ( 'NONE', *, *, #36523, .T. ) ;
#30772 = CIRCLE ( 'NONE', #9645, 15.99999999999999645 ) ;
#30773 = CYLINDRICAL_SURFACE ( 'NONE', #36146, 31.99999999999998579 ) ;
#30774 = VERTEX_POINT ( 'NONE', #34853 ) ;
#30775 = ORIENTED_EDGE ( 'NONE', *, *, #9739, .F. ) ;
#30776 = ORIENTED_EDGE ( 'NONE', *, *, #19100, .F. ) ;
#30777 = EDGE_CURVE ( 'NONE', #39062, #17273, #14372, .T. ) ;
#30778 = AXIS2_PLACEMENT_3D ( 'NONE', #46563, #10066, #28429 ) ;
#30779 = CIRCLE ( 'NONE', #9657, 31.99999999999998934 ) ;
#30780 = ORIENTED_EDGE ( 'NONE', *, *, #31801, .T. ) ;
#30781 = EDGE_CURVE ( 'NONE', #9766, #12926, #18267, .T. ) ;
#30782 = ORIENTED_EDGE ( 'NONE', *, *, #13321, .T. ) ;
#30783 = ORIENTED_EDGE ( 'NONE', *, *, #40473, .F. ) ;
#30784 = CARTESIAN_POINT ( 'NONE',  ( 0.000000000000000000, 0.000000000000000000, 0.000000000000000000 ) ) ;
#30785 = ORIENTED_EDGE ( 'NONE', *, *, #46493, .T. ) ;
#30786 = EDGE_CURVE ( 'NONE', #23469, #4226, #24573, .T. ) ;
#30787 = AXIS2_PLACEMENT_3D ( 'NONE', #15654, #30586, #4640 ) ;
#30788 = VERTEX_POINT ( 'NONE', #17450 ) ;
#30789 = CARTESIAN_POINT ( 'NONE',  ( 10.00000000000000000, 22.74946021919175720, -29.81001611430984255 ) ) ;
#30790 = ORIENTED_EDGE ( 'NONE', *, *, #17789, .F. ) ;
#30791 = VERTEX_POINT ( 'NONE', #5984 ) ;
#30792 = EDGE_CURVE ( 'NONE', #38227, #39318, #39988, .T. ) ;
#30793 = EDGE_CURVE ( 'NONE', #12477, #38938, #9678, .T. ) ;
#30794 = AXIS2_PLACEMENT_3D ( 'NONE', #18766, #29073, #41078 ) ;
#30795 = FACE_OUTER_BOUND ( 'NONE', #20461, .T. ) ;
#30797 = EDGE_LOOP ( 'NONE', ( #34745, #19437, #3682, #20964 ) ) ;
#30796 = DIRECTION ( 'NONE',  ( 0.000000000000000000, 0.9238795325112851842, 0.3826834323650937786 ) ) ;
#30799 = DIRECTION ( 'NONE',  ( -1.000000000000000000, -0.000000000000000000, -0.000000000000000000 ) ) ;
#30798 = AXIS2_PLACEMENT_3D ( 'NONE', #25978, #25497, #44584 ) ;
#30800 = ORIENTED_EDGE ( 'NONE', *, *, #1583, .F. ) ;
#30801 = DIRECTION ( 'NONE',  ( -0.5200609990132993854, -0.8541291221503274356, 0.000000000000000000 ) ) ;
#30802 = EDGE_CURVE ( 'NONE', #38611, #35831, #3238, .T. ) ;
#30803 = ORIENTED_EDGE ( 'NONE', *, *, #15031, .T. ) ;
#30804 = ORIENTED_EDGE ( 'NONE', *, *, #2764, .F. ) ;
#30805 = DIRECTION ( 'NONE',  ( 0.000000000000000000, 0.1045284632676570791, -0.9945218953682730678 ) ) ;
#30806 = CIRCLE ( 'NONE', #310, 16.00000000000000000 ) ;
#30807 = AXIS2_PLACEMENT_3D ( 'NONE', #15567, #11901, #27081 ) ;
#30808 = DIRECTION ( 'NONE',  ( -1.000000000000000000, -0.000000000000000000, 0.000000000000000000 ) ) ;
#30809 = CIRCLE ( 'NONE', #9686, 15.39727592589476579 ) ;
#30810 = ORIENTED_EDGE ( 'NONE', *, *, #27463, .F. ) ;
#30811 = CARTESIAN_POINT ( 'NONE',  ( 0.000000000000000000, 81.96053171279902472, 2.543863470248670211 ) ) ;
#30812 = LINE ( 'NONE', #23689, #40857 ) ;
#30813 = ORIENTED_EDGE ( 'NONE', *, *, #17459, .F. ) ;
#30814 = VERTEX_POINT ( 'NONE', #20903 ) ;
#30815 = DIRECTION ( 'NONE',  ( 0.000000000000000000, 0.000000000000000000, -1.000000000000000000 ) ) ;
#30816 = ADVANCED_FACE ( 'NONE', ( #2770 ), #28953, .T. ) ;
#30817 = CARTESIAN_POINT ( 'NONE',  ( 10.00000000000000000, 37.22597642581158084, -5.202137450156524068 ) ) ;
#30818 = AXIS2_PLACEMENT_3D ( 'NONE', #32157, #24317, #25992 ) ;
#30819 = VERTEX_POINT ( 'NONE', #10612 ) ;
#30820 = AXIS2_PLACEMENT_3D ( 'NONE', #16367, #16140, #19304 ) ;
#30821 = CARTESIAN_POINT ( 'NONE',  ( 0.000000000000000000, -63.97538442413463855, 51.29473840253199057 ) ) ;
#30822 = ORIENTED_EDGE ( 'NONE', *, *, #6626, .T. ) ;
#30823 = CIRCLE ( 'NONE', #9696, 31.99999999999997868 ) ;
#30824 = PLANE ( 'NONE',  #34762 ) ;
#30825 = LINE ( 'NONE', #23226, #46658 ) ;
#30826 = CARTESIAN_POINT ( 'NONE',  ( -16.07206065793331007, -141.0698568150738197, -2.500000000000000000 ) ) ;
#30827 = DIRECTION ( 'NONE',  ( 1.000000000000000000, 0.000000000000000000, 0.000000000000000000 ) ) ;
#30828 = CARTESIAN_POINT ( 'NONE',  ( 10.00000000000000000, 0.000000000000000000, 0.000000000000000000 ) ) ;
#30829 = CARTESIAN_POINT ( 'NONE',  ( 0.000000000000000000, -120.0000000000000000, 2.500000000000000000 ) ) ;
#30830 = FACE_OUTER_BOUND ( 'NONE', #21735, .T. ) ;
#30831 = ORIENTED_EDGE ( 'NONE', *, *, #16147, .F. ) ;
#30832 = DIRECTION ( 'NONE',  ( 0.000000000000000000, 0.000000000000000000, -1.000000000000000000 ) ) ;
#30833 = DIRECTION ( 'NONE',  ( -1.000000000000000000, -0.000000000000000000, -0.000000000000000000 ) ) ;
#30834 = EDGE_LOOP ( 'NONE', ( #19873, #736, #19107, #6171 ) ) ;
#30835 = ORIENTED_EDGE ( 'NONE', *, *, #18230, .F. ) ;
#30836 = CIRCLE ( 'NONE', #19866, 16.00000000000000000 ) ;
#30837 = LINE ( 'NONE', #643, #46480 ) ;
#30838 = AXIS2_PLACEMENT_3D ( 'NONE', #45381, #39252, #5982 ) ;
#30839 = ADVANCED_FACE ( 'NONE', ( #43889 ), #47330, .T. ) ;
#30840 = DIRECTION ( 'NONE',  ( -1.000000000000000000, 0.000000000000000000, -0.000000000000000000 ) ) ;
#30841 = DIRECTION ( 'NONE',  ( -1.000000000000000000, -0.000000000000000000, -0.000000000000000000 ) ) ;
#30842 = EDGE_CURVE ( 'NONE', #12261, #42331, #36946, .T. ) ;
#30843 = ORIENTED_EDGE ( 'NONE', *, *, #42371, .T. ) ;
#30844 = EDGE_CURVE ( 'NONE', #47607, #1817, #12725, .T. ) ;
#30845 = EDGE_CURVE ( 'NONE', #38290, #32306, #29198, .T. ) ;
#30846 = AXIS2_PLACEMENT_3D ( 'NONE', #2841, #35663, #5811 ) ;
#30847 = VECTOR ( 'NONE', #31138, 1000.000000000000000 ) ;
#30848 = EDGE_CURVE ( 'NONE', #28620, #35445, #9622, .T. ) ;
#30849 = VECTOR ( 'NONE', #33460, 1000.000000000000000 ) ;
#30850 = DIRECTION ( 'NONE',  ( 0.000000000000000000, 0.4539904997395412534, 0.8910065241883706744 ) ) ;
#30851 = ORIENTED_EDGE ( 'NONE', *, *, #22151, .F. ) ;
#30852 = ORIENTED_EDGE ( 'NONE', *, *, #16102, .T. ) ;
#30853 = VERTEX_POINT ( 'NONE', #24810 ) ;
#30854 = ORIENTED_EDGE ( 'NONE', *, *, #3795, .F. ) ;
#30855 = VERTEX_POINT ( 'NONE', #28727 ) ;
#30856 = AXIS2_PLACEMENT_3D ( 'NONE', #16154, #5134, #23470 ) ;
#30857 = ADVANCED_FACE ( 'NONE', ( #10118 ), #45557, .F. ) ;
#30858 = LINE ( 'NONE', #45788, #23524 ) ;
#30859 = ORIENTED_EDGE ( 'NONE', *, *, #17001, .F. ) ;
#30860 = VERTEX_POINT ( 'NONE', #21847 ) ;
#30861 = CARTESIAN_POINT ( 'NONE',  ( 0.000000000000000000, 65.64334221924966073, -41.19522573413664190 ) ) ;
#30862 = EDGE_CURVE ( 'NONE', #26881, #42399, #23688, .T. ) ;
#30863 = VERTEX_POINT ( 'NONE', #35825 ) ;
#30864 = CARTESIAN_POINT ( 'NONE',  ( 10.00000000000000000, -35.47612816024506088, -22.48208911017539435 ) ) ;
#30865 = ORIENTED_EDGE ( 'NONE', *, *, #17969, .F. ) ;
#30866 = DIRECTION ( 'NONE',  ( 0.000000000000000000, -0.9238795325112906243, 0.3826834323650805114 ) ) ;
#30867 = DIRECTION ( 'NONE',  ( -1.000000000000000000, 0.000000000000000000, 0.000000000000000000 ) ) ;
#30868 = ORIENTED_EDGE ( 'NONE', *, *, #5158, .T. ) ;
#30869 = DIRECTION ( 'NONE',  ( -1.000000000000000000, -0.000000000000000000, 0.000000000000000000 ) ) ;
#30870 = ORIENTED_EDGE ( 'NONE', *, *, #22373, .T. ) ;
#30872 = ORIENTED_EDGE ( 'NONE', *, *, #32639, .F. ) ;
#30871 = CARTESIAN_POINT ( 'NONE',  ( 4.999999999999999112, -40.98264845739743123, -9.188173127307734944 ) ) ;
#30873 = EDGE_CURVE ( 'NONE', #32923, #45066, #18185, .T. ) ;
#30874 = CIRCLE ( 'NONE', #23069, 12.49999999999999822 ) ;
#30875 = LINE ( 'NONE', #1248, #25821 ) ;
#30876 = ORIENTED_EDGE ( 'NONE', *, *, #35259, .F. ) ;
#30877 = CARTESIAN_POINT ( 'NONE',  ( 0.000000000000000000, -74.65491531819111515, 23.16904090965678265 ) ) ;
#30878 = ORIENTED_EDGE ( 'NONE', *, *, #20434, .F. ) ;
#30879 = CARTESIAN_POINT ( 'NONE',  ( -14.87942725330654348, -141.9795960975983178, 5.500000000000000000 ) ) ;
#30880 = AXIS2_PLACEMENT_3D ( 'NONE', #11118, #6959, #25307 ) ;
#30881 = CARTESIAN_POINT ( 'NONE',  ( 10.00000000000000000, -75.16055320797043748, 18.89407956138229494 ) ) ;
#30882 = ORIENTED_EDGE ( 'NONE', *, *, #23105, .F. ) ;
#30883 = DIRECTION ( 'NONE',  ( 1.000000000000000000, -0.000000000000000000, -0.000000000000000000 ) ) ;
#30884 = PLANE ( 'NONE',  #47766 ) ;
#30885 = DIRECTION ( 'NONE',  ( -1.000000000000000000, 0.000000000000000000, 0.000000000000000000 ) ) ;
#30886 = PRODUCT_DEFINITION_SHAPE ( 'NONE', 'NONE',  #48463 ) ;
#30887 = LINE ( 'NONE', #999, #6213 ) ;
#30888 = CARTESIAN_POINT ( 'NONE',  ( 10.00000000000000000, 0.000000000000000000, 0.000000000000000000 ) ) ;
#30889 = CARTESIAN_POINT ( 'NONE',  ( 12.49999999999999645, 1.530808498934191127E-15, 125.0000000000000000 ) ) ;
#30890 = EDGE_CURVE ( 'NONE', #23694, #46638, #1794, .T. ) ;
#30891 = VECTOR ( 'NONE', #30106, 1000.000000000000000 ) ;
#30892 = CARTESIAN_POINT ( 'NONE',  ( 11.99999999999999822, 0.000000000000000000, 0.000000000000000000 ) ) ;
#30893 = DIRECTION ( 'NONE',  ( 0.000000000000000000, -0.9510565162951543083, 0.3090169943749448977 ) ) ;
#30894 = DIRECTION ( 'NONE',  ( 0.000000000000000000, -0.7604059656000227152, -0.6494480483301933171 ) ) ;
#30895 = VERTEX_POINT ( 'NONE', #36304 ) ;
#30896 = AXIS2_PLACEMENT_3D ( 'NONE', #19965, #8699, #31010 ) ;
#30897 = CARTESIAN_POINT ( 'NONE',  ( 10.00000000000000000, 41.81611651403861885, 3.925862922256313503 ) ) ;
#30898 = DIRECTION ( 'NONE',  ( 0.000000000000000000, 0.000000000000000000, 1.000000000000000000 ) ) ;
#30899 = LINE ( 'NONE', #35272, #17799 ) ;
#30900 = DIRECTION ( 'NONE',  ( 0.000000000000000000, 0.000000000000000000, 1.000000000000000000 ) ) ;
#30901 = CIRCLE ( 'NONE', #33224, 82.00000000000000000 ) ;
#30902 = AXIS2_PLACEMENT_3D ( 'NONE', #18623, #14479, #33551 ) ;
#30903 = EDGE_LOOP ( 'NONE', ( #23318, #44204, #9115, #7094 ) ) ;
#30904 = EDGE_CURVE ( 'NONE', #27674, #9216, #7266, .T. ) ;
#30905 = VERTEX_POINT ( 'NONE', #39755 ) ;
#30906 = PLANE ( 'NONE',  #26966 ) ;
#30907 = ORIENTED_EDGE ( 'NONE', *, *, #10186, .F. ) ;
#30908 = EDGE_CURVE ( 'NONE', #27887, #24885, #33045, .T. ) ;
#30909 = DIRECTION ( 'NONE',  ( -1.000000000000000000, 0.000000000000000000, 0.000000000000000000 ) ) ;
#30910 = AXIS2_PLACEMENT_3D ( 'NONE', #20826, #17623, #29115 ) ;
#30911 = DIRECTION ( 'NONE',  ( -1.000000000000000000, 0.000000000000000000, 0.000000000000000000 ) ) ;
#30912 = VERTEX_POINT ( 'NONE', #22821 ) ;
#30913 = EDGE_CURVE ( 'NONE', #22056, #38126, #8793, .T. ) ;
#30914 = VECTOR ( 'NONE', #38045, 1000.000000000000000 ) ;
#30915 = EDGE_CURVE ( 'NONE', #42540, #6202, #29128, .T. ) ;
#30916 = AXIS2_PLACEMENT_3D ( 'NONE', #29164, #43628, #10324 ) ;
#30917 = EDGE_LOOP ( 'NONE', ( #34618, #1512, #45203, #18249 ) ) ;
#30918 = FACE_OUTER_BOUND ( 'NONE', #20127, .T. ) ;
#30919 = ORIENTED_EDGE ( 'NONE', *, *, #23662, .F. ) ;
#30920 = VECTOR ( 'NONE', #2030, 1000.000000000000000 ) ;
#30921 = CIRCLE ( 'NONE', #12169, 77.49900000000000944 ) ;
#30922 = CARTESIAN_POINT ( 'NONE',  ( 10.00000000000000000, -4.992566952384716927, -37.16516213103282951 ) ) ;
#30923 = ORIENTED_EDGE ( 'NONE', *, *, #13487, .F. ) ;
#30924 = DIRECTION ( 'NONE',  ( 0.000000000000000000, 0.7071067811865439090, 0.7071067811865512365 ) ) ;
#30926 = ORIENTED_EDGE ( 'NONE', *, *, #21041, .F. ) ;
#30925 = DIRECTION ( 'NONE',  ( -1.000000000000000000, -0.000000000000000000, 0.000000000000000000 ) ) ;
#30927 = ORIENTED_EDGE ( 'NONE', *, *, #26584, .T. ) ;
#30928 = AXIS2_PLACEMENT_3D ( 'NONE', #19189, #34115, #37314 ) ;
#30929 = ORIENTED_EDGE ( 'NONE', *, *, #12331, .F. ) ;
#30930 = VECTOR ( 'NONE', #16296, 1000.000000000000114 ) ;
#30931 = AXIS2_PLACEMENT_3D ( 'NONE', #11535, #27188, #4663 ) ;
#30932 = DIRECTION ( 'NONE',  ( -1.000000000000000000, -0.000000000000000000, 0.000000000000000000 ) ) ;
#30933 = DIRECTION ( 'NONE',  ( -1.000000000000000000, 0.000000000000000000, 0.000000000000000000 ) ) ;
#30934 = CARTESIAN_POINT ( 'NONE',  ( -12.49999999999999645, 0.000000000000000000, -44.99999999999998579 ) ) ;
#30935 = CARTESIAN_POINT ( 'NONE',  ( 0.000000000000000000, 37.01155633439059756, 6.555932627142549762 ) ) ;
#30936 = ORIENTED_EDGE ( 'NONE', *, *, #10049, .F. ) ;
#30937 = CARTESIAN_POINT ( 'NONE',  ( 10.00000000000000000, 0.000000000000000000, 0.000000000000000000 ) ) ;
#30938 = VERTEX_POINT ( 'NONE', #552 ) ;
#30939 = ORIENTED_EDGE ( 'NONE', *, *, #16809, .T. ) ;
#30940 = DIRECTION ( 'NONE',  ( -1.000000000000000000, 0.000000000000000000, 0.000000000000000000 ) ) ;
#30941 = ORIENTED_EDGE ( 'NONE', *, *, #24212, .T. ) ;
#30942 = CARTESIAN_POINT ( 'NONE',  ( 0.000000000000000000, 26.08949754953062694, -27.05870788708203989 ) ) ;
#30943 = CIRCLE ( 'NONE', #7483, 15.99999999999999822 ) ;
#30944 = FACE_OUTER_BOUND ( 'NONE', #20288, .T. ) ;
#30945 = CYLINDRICAL_SURFACE ( 'NONE', #27414, 31.99999999999998579 ) ;
#30946 = ORIENTED_EDGE ( 'NONE', *, *, #24758, .T. ) ;
#30947 = DIRECTION ( 'NONE',  ( 0.000000000000000000, -0.7604059656000227152, -0.6494480483301933171 ) ) ;
#30948 = DIRECTION ( 'NONE',  ( 0.000000000000000000, 0.6691306063588563502, 0.7431448254773960205 ) ) ;
#30949 = DIRECTION ( 'NONE',  ( -1.000000000000000000, -0.000000000000000000, -0.000000000000000000 ) ) ;
#30950 = CARTESIAN_POINT ( 'NONE',  ( 10.00000000000000000, 51.02545421589402252, -55.20638768913705263 ) ) ;
#30951 = CIRCLE ( 'NONE', #39543, 16.00000000000000000 ) ;
#30952 = CARTESIAN_POINT ( 'NONE',  ( 10.00000000000000000, 71.27951684758026829, 30.41916302227139113 ) ) ;
#30953 = ADVANCED_FACE ( 'NONE', ( #45103 ), #34305, .T. ) ;
#30954 = PLANE ( 'NONE',  #2766 ) ;
#30955 = DIRECTION ( 'NONE',  ( -1.000000000000000000, 0.000000000000000000, -0.000000000000000000 ) ) ;
#30956 = CARTESIAN_POINT ( 'NONE',  ( 0.000000000000000000, -36.88895765772637247, 6.736453364083436313 ) ) ;
#30957 = LINE ( 'NONE', #45883, #29097 ) ;
#30958 = CARTESIAN_POINT ( 'NONE',  ( 10.00000000000000000, 22.90783923731741112, -78.73519480814930205 ) ) ;
#30959 = VERTEX_POINT ( 'NONE', #22350 ) ;
#30960 = EDGE_CURVE ( 'NONE', #16242, #23540, #8133, .T. ) ;
#30961 = VECTOR ( 'NONE', #40838, 1000.000000000000000 ) ;
#30962 = DIRECTION ( 'NONE',  ( -1.000000000000000000, 0.000000000000000000, 0.000000000000000000 ) ) ;
#30963 = FACE_OUTER_BOUND ( 'NONE', #23752, .T. ) ;
#30964 = ORIENTED_EDGE ( 'NONE', *, *, #5688, .F. ) ;
#30965 = ORIENTED_EDGE ( 'NONE', *, *, #46704, .F. ) ;
#30966 = EDGE_CURVE ( 'NONE', #41833, #15455, #8027, .T. ) ;
#30967 = CARTESIAN_POINT ( 'NONE',  ( 10.00000000000000000, 0.000000000000000000, 0.000000000000000000 ) ) ;
#30968 = AXIS2_PLACEMENT_3D ( 'NONE', #47317, #28714, #13790 ) ;
#30969 = EDGE_CURVE ( 'NONE', #1904, #22493, #11809, .T. ) ;
#30970 = DIRECTION ( 'NONE',  ( 0.000000000000000000, 0.5877852522924684742, 0.8090169943749506709 ) ) ;
#30971 = CIRCLE ( 'NONE', #2035, 82.00000000000000000 ) ;
#30972 = EDGE_LOOP ( 'NONE', ( #45343, #26684, #25225, #42990 ) ) ;
#30973 = AXIS2_PLACEMENT_3D ( 'NONE', #29732, #41722, #26063 ) ;
#30974 = EDGE_CURVE ( 'NONE', #7137, #25598, #38002, .T. ) ;
#30975 = ORIENTED_EDGE ( 'NONE', *, *, #47329, .F. ) ;
#30976 = AXIS2_PLACEMENT_3D ( 'NONE', #284, #3972, #33812 ) ;
#30978 = EDGE_CURVE ( 'NONE', #27571, #13807, #40949, .T. ) ;
#30977 = ORIENTED_EDGE ( 'NONE', *, *, #2422, .T. ) ;
#30979 = AXIS2_PLACEMENT_3D ( 'NONE', #11136, #17502, #14810 ) ;
#30980 = ORIENTED_EDGE ( 'NONE', *, *, #6251, .T. ) ;
#30981 = AXIS2_PLACEMENT_3D ( 'NONE', #31618, #24742, #38722 ) ;
#30982 = DIRECTION ( 'NONE',  ( 1.000000000000000000, 0.000000000000000000, 0.000000000000000000 ) ) ;
#30983 = CARTESIAN_POINT ( 'NONE',  ( 7.893099573151324044, -11.68370571044642503, -1.199999999999999956 ) ) ;
#30984 = DIRECTION ( 'NONE',  ( -0.3311129884571295534, -0.9435911131814398445, 0.000000000000000000 ) ) ;
#30985 = EDGE_CURVE ( 'NONE', #20241, #19341, #19378, .T. ) ;
#30986 = ORIENTED_EDGE ( 'NONE', *, *, #36373, .F. ) ;
#30987 = DIRECTION ( 'NONE',  ( 0.000000000000000000, -0.8910065241883626808, -0.4539904997395570740 ) ) ;
#30988 = ORIENTED_EDGE ( 'NONE', *, *, #30359, .F. ) ;
#30989 = AXIS2_PLACEMENT_3D ( 'NONE', #41063, #26601, #7981 ) ;
#30990 = EDGE_LOOP ( 'NONE', ( #11282, #31997, #39944, #5163 ) ) ;
#30991 = CARTESIAN_POINT ( 'NONE',  ( 0.000000000000000000, 41.76937507738875155, -62.50329211542393892 ) ) ;
#30992 = LINE ( 'NONE', #16999, #45008 ) ;
#30993 = DIRECTION ( 'NONE',  ( -1.000000000000000000, 0.000000000000000000, 0.000000000000000000 ) ) ;
#30994 = AXIS2_PLACEMENT_3D ( 'NONE', #15394, #37408, #7785 ) ;
#30995 = ORIENTED_EDGE ( 'NONE', *, *, #28962, .F. ) ;
#30996 = ORIENTED_EDGE ( 'NONE', *, *, #9280, .F. ) ;
#30997 = LINE ( 'NONE', #26582, #1323 ) ;
#30998 = EDGE_LOOP ( 'NONE', ( #4834, #28468, #832 ) ) ;
#30999 = DIRECTION ( 'NONE',  ( -1.000000000000000000, 0.000000000000000000, 0.000000000000000000 ) ) ;
#31000 = AXIS2_PLACEMENT_3D ( 'NONE', #31615, #43808, #39682 ) ;
#31001 = DIRECTION ( 'NONE',  ( 0.9827303690289282967, 0.1850432970638667407, -0.000000000000000000 ) ) ;
#31002 = DIRECTION ( 'NONE',  ( 0.000000000000000000, 0.8526401643540897357, 0.5224985647159527957 ) ) ;
#31003 = LINE ( 'NONE', #6017, #33127 ) ;
#31004 = DIRECTION ( 'NONE',  ( 0.000000000000000000, 0.6494480483301793283, 0.7604059656000345946 ) ) ;
#31005 = DIRECTION ( 'NONE',  ( 0.000000000000000000, 0.9510565162951523099, 0.3090169943749517811 ) ) ;
#31006 = LINE ( 'NONE', #4797, #47121 ) ;
#31007 =( LENGTH_UNIT ( ) NAMED_UNIT ( * ) SI_UNIT ( .MILLI., .METRE. ) );
#31008 = DIRECTION ( 'NONE',  ( -0.1850432970638667129, 0.9827303690289281857, 0.000000000000000000 ) ) ;
#31009 = CYLINDRICAL_SURFACE ( 'NONE', #39996, 16.00000000000000000 ) ;
#31010 = DIRECTION ( 'NONE',  ( 0.000000000000000000, 0.000000000000000000, -1.000000000000000000 ) ) ;
#31011 = EDGE_CURVE ( 'NONE', #29568, #19113, #44376, .T. ) ;
#31012 = ORIENTED_EDGE ( 'NONE', *, *, #25161, .T. ) ;
#31013 = AXIS2_PLACEMENT_3D ( 'NONE', #2961, #17890, #14228 ) ;
#31014 = EDGE_CURVE ( 'NONE', #40883, #43442, #4932, .T. ) ;
#31015 = CARTESIAN_POINT ( 'NONE',  ( 6.000000000000000000, 10.30890764327382136, 81.34940948281339956 ) ) ;
#31016 = AXIS2_PLACEMENT_3D ( 'NONE', #28165, #24493, #31620 ) ;
#31017 = CARTESIAN_POINT ( 'NONE',  ( 10.00000000000000000, 2.946379043146343246, 75.11764819372150725 ) ) ;
#31018 = CARTESIAN_POINT ( 'NONE',  ( 0.000000000000000000, 37.48860685352291000, -0.8828120875901940279 ) ) ;
#31019 = CIRCLE ( 'NONE', #43515, 42.00000000000000000 ) ;
#31020 = ADVANCED_FACE ( 'NONE', ( #11340 ), #40698, .T. ) ;
#31021 = FILL_AREA_STYLE ('',( #8710 ) ) ;
#31022 = DIRECTION ( 'NONE',  ( 0.08130631524010120681, -0.9966891607226784355, 0.000000000000000000 ) ) ;
#31023 = VECTOR ( 'NONE', #3851, 1000.000000000000000 ) ;
#31024 = CARTESIAN_POINT ( 'NONE',  ( 11.99999999999999822, -77.19088730480518734, -6.903761155838607166 ) ) ;
#31025 = DIRECTION ( 'NONE',  ( -1.000000000000000000, 0.000000000000000000, 0.000000000000000000 ) ) ;
#31026 = ORIENTED_EDGE ( 'NONE', *, *, #34639, .T. ) ;
#31027 = VERTEX_POINT ( 'NONE', #37508 ) ;
#31028 = ADVANCED_FACE ( 'NONE', ( #37271 ), #48282, .T. ) ;
#31029 = DIRECTION ( 'NONE',  ( 1.000000000000000000, 0.000000000000000000, 0.000000000000000000 ) ) ;
#31030 = EDGE_CURVE ( 'NONE', #17149, #13012, #44614, .T. ) ;
#31031 = EDGE_CURVE ( 'NONE', #26821, #22916, #15253, .T. ) ;
#31032 = ORIENTED_EDGE ( 'NONE', *, *, #15647, .T. ) ;
#31033 = VECTOR ( 'NONE', #18513, 1000.000000000000000 ) ;
#31034 = ORIENTED_EDGE ( 'NONE', *, *, #9166, .T. ) ;
#31035 = ORIENTED_EDGE ( 'NONE', *, *, #1799, .F. ) ;
#31036 = CARTESIAN_POINT ( 'NONE',  ( 10.00000000000000000, -74.65374052328654386, 8.840884882374837161 ) ) ;
#31037 = ORIENTED_EDGE ( 'NONE', *, *, #1025, .T. ) ;
#31038 = EDGE_CURVE ( 'NONE', #40126, #38600, #3736, .T. ) ;
#31039 = ORIENTED_EDGE ( 'NONE', *, *, #45493, .T. ) ;
#31040 = AXIS2_PLACEMENT_3D ( 'NONE', #20638, #31687, #13071 ) ;
#31041 = LINE ( 'NONE', #9226, #3067 ) ;
#31042 = CYLINDRICAL_SURFACE ( 'NONE', #14388, 82.00000000000000000 ) ;
#31043 = ORIENTED_EDGE ( 'NONE', *, *, #4104, .T. ) ;
#31044 = ORIENTED_EDGE ( 'NONE', *, *, #43410, .F. ) ;
#31045 = CIRCLE ( 'NONE', #23980, 82.00000000000000000 ) ;
#31046 = DIRECTION ( 'NONE',  ( 0.000000000000000000, 0.000000000000000000, 1.000000000000000000 ) ) ;
#31048 = ORIENTED_EDGE ( 'NONE', *, *, #21551, .F. ) ;
#31047 = CYLINDRICAL_SURFACE ( 'NONE', #21906, 31.99999999999999289 ) ;
#31049 = CIRCLE ( 'NONE', #22449, 77.49900000000002365 ) ;
#31050 = CARTESIAN_POINT ( 'NONE',  ( 10.00000000000000000, -33.00180498840060039, 17.80606268964528027 ) ) ;
#31051 = EDGE_LOOP ( 'NONE', ( #10258, #26929, #34457, #34814 ) ) ;
#31052 = CARTESIAN_POINT ( 'NONE',  ( 2.874421927457452952, -143.3717286177755739, -5.500000000000000000 ) ) ;
#31053 = VERTEX_POINT ( 'NONE', #7653 ) ;
#31054 = ORIENTED_EDGE ( 'NONE', *, *, #19673, .F. ) ;
#31055 = CARTESIAN_POINT ( 'NONE',  ( 10.00000000000000000, 0.000000000000000000, 0.000000000000000000 ) ) ;
#31056 = CARTESIAN_POINT ( 'NONE',  ( 11.99999999999999822, 65.64334221924909230, 41.19522573413756561 ) ) ;
#31057 = VERTEX_POINT ( 'NONE', #30181 ) ;
#31058 = CYLINDRICAL_SURFACE ( 'NONE', #7239, 37.49900000000000233 ) ;
#31059 = DIRECTION ( 'NONE',  ( 0.000000000000000000, 0.000000000000000000, 1.000000000000000000 ) ) ;
#31060 = CARTESIAN_POINT ( 'NONE',  ( 10.00000000000000000, 6.736453364083557105, 36.88895765772635826 ) ) ;
#31061 = EDGE_LOOP ( 'NONE', ( #44769, #29982, #14015, #19486 ) ) ;
#31062 = EDGE_LOOP ( 'NONE', ( #25995, #47753, #45471, #7776 ) ) ;
#31063 = CIRCLE ( 'NONE', #27918, 31.99999999999999645 ) ;
#31064 = DIRECTION ( 'NONE',  ( 0.000000000000000000, 0.000000000000000000, 1.000000000000000000 ) ) ;
#31065 = CARTESIAN_POINT ( 'NONE',  ( 12.50000000000000000, -132.5000000000000000, 2.500000000000000000 ) ) ;
#31066 = AXIS2_PLACEMENT_3D ( 'NONE', #45352, #11598, #4262 ) ;
#31067 = EDGE_CURVE ( 'NONE', #34023, #12855, #22580, .T. ) ;
#31068 = ORIENTED_EDGE ( 'NONE', *, *, #31188, .F. ) ;
#31069 = CARTESIAN_POINT ( 'NONE',  ( 10.00000000000000000, -51.03279382321048985, -55.19960302592120627 ) ) ;
#31070 = ORIENTED_EDGE ( 'NONE', *, *, #40964, .F. ) ;
#31071 = EDGE_CURVE ( 'NONE', #40610, #40065, #33826, .T. ) ;
#31072 = FACE_OUTER_BOUND ( 'NONE', #30050, .T. ) ;
#31073 = CIRCLE ( 'NONE', #13072, 77.49900000000000944 ) ;
#31074 = DIRECTION ( 'NONE',  ( 0.000000000000000000, 0.000000000000000000, 1.000000000000000000 ) ) ;
#31075 = DIRECTION ( 'NONE',  ( -1.000000000000000000, 0.000000000000000000, 0.000000000000000000 ) ) ;
#31076 = CARTESIAN_POINT ( 'NONE',  ( -2.500000000000000000, 16.00000000000000000, 0.000000000000000000 ) ) ;
#31077 = EDGE_CURVE ( 'NONE', #27912, #42537, #20339, .T. ) ;
#31078 = DIRECTION ( 'NONE',  ( -0.9997280174009349762, 0.02332147558787671729, 0.000000000000000000 ) ) ;
#31079 = FACE_OUTER_BOUND ( 'NONE', #47673, .T. ) ;
#31080 = DIRECTION ( 'NONE',  ( -1.000000000000000000, -0.000000000000000000, -0.000000000000000000 ) ) ;
#31081 = FACE_OUTER_BOUND ( 'NONE', #11091, .T. ) ;
#31082 = ORIENTED_EDGE ( 'NONE', *, *, #3472, .F. ) ;
#31083 = CARTESIAN_POINT ( 'NONE',  ( 0.000000000000000000, -21.32104025579135964, 30.84782396557210760 ) ) ;
#31084 = EDGE_CURVE ( 'NONE', #20902, #27256, #37742, .T. ) ;
#31085 = EDGE_CURVE ( 'NONE', #21091, #7113, #34543, .T. ) ;
#31086 = VERTEX_POINT ( 'NONE', #46068 ) ;
#31087 = CARTESIAN_POINT ( 'NONE',  ( 11.99999999999999822, -36.73666225445940370, 65.58780272294062286 ) ) ;
#31088 = VERTEX_POINT ( 'NONE', #42388 ) ;
#31089 = DIRECTION ( 'NONE',  ( 1.000000000000000000, 0.000000000000000000, 0.000000000000000000 ) ) ;
#31090 = CARTESIAN_POINT ( 'NONE',  ( 0.000000000000000000, -51.03279382321125723, 55.19960302592048862 ) ) ;
#31091 = ORIENTED_EDGE ( 'NONE', *, *, #28596, .T. ) ;
#31092 = EDGE_CURVE ( 'NONE', #44962, #18546, #15063, .T. ) ;
#31093 = AXIS2_PLACEMENT_3D ( 'NONE', #26468, #26960, #33562 ) ;
#31094 = LINE ( 'NONE', #37945, #40641 ) ;
#31095 = AXIS2_PLACEMENT_3D ( 'NONE', #4096, #164, #31022 ) ;
#31096 = ORIENTED_EDGE ( 'NONE', *, *, #1083, .T. ) ;
#31097 = ORIENTED_EDGE ( 'NONE', *, *, #20536, .F. ) ;
#31098 = VERTEX_POINT ( 'NONE', #35041 ) ;
#31099 = ORIENTED_EDGE ( 'NONE', *, *, #33218, .F. ) ;
#31100 = CARTESIAN_POINT ( 'NONE',  ( 15.00000000000000000, -26.23277895567251505, -4.042438405569750870 ) ) ;
#31101 = ORIENTED_EDGE ( 'NONE', *, *, #33929, .F. ) ;
#31102 = CIRCLE ( 'NONE', #24834, 37.49900000000000233 ) ;
#31103 = ORIENTED_EDGE ( 'NONE', *, *, #44084, .T. ) ;
#31104 = FACE_OUTER_BOUND ( 'NONE', #5488, .T. ) ;
#31105 = ORIENTED_EDGE ( 'NONE', *, *, #20999, .T. ) ;
#31106 = DIRECTION ( 'NONE',  ( -1.000000000000000000, 0.000000000000000000, 0.000000000000000000 ) ) ;
#31107 = DIRECTION ( 'NONE',  ( -1.000000000000000000, 0.000000000000000000, 0.000000000000000000 ) ) ;
#31108 = FACE_OUTER_BOUND ( 'NONE', #856, .T. ) ;
#31109 = ORIENTED_EDGE ( 'NONE', *, *, #11664, .T. ) ;
#31110 = DIRECTION ( 'NONE',  ( -1.000000000000000000, -0.000000000000000000, -0.000000000000000000 ) ) ;
#31111 = VERTEX_POINT ( 'NONE', #9332 ) ;
#31112 = AXIS2_PLACEMENT_3D ( 'NONE', #1113, #31001, #23625 ) ;
#31113 = CARTESIAN_POINT ( 'NONE',  ( 0.000000000000000000, 0.000000000000000000, 53.20000000000001705 ) ) ;
#31114 = DIRECTION ( 'NONE',  ( 0.000000000000000000, 0.000000000000000000, 1.000000000000000000 ) ) ;
#31115 = ORIENTED_EDGE ( 'NONE', *, *, #35146, .F. ) ;
#31116 = CARTESIAN_POINT ( 'NONE',  ( 10.00000000000000000, 65.59268652807263322, -36.72794159290169347 ) ) ;
#31117 = ORIENTED_EDGE ( 'NONE', *, *, #101, .T. ) ;
#31118 = ORIENTED_EDGE ( 'NONE', *, *, #40004, .T. ) ;
#31119 = CARTESIAN_POINT ( 'NONE',  ( 10.00000000000000000, 30.84782396557218931, 21.32104025579126017 ) ) ;
#31120 = DIRECTION ( 'NONE',  ( -1.000000000000000000, -0.000000000000000000, -0.000000000000000000 ) ) ;
#31121 = ADVANCED_FACE ( 'NONE', ( #5669 ), #16440, .T. ) ;
#31122 = DIRECTION ( 'NONE',  ( 0.000000000000000000, 0.000000000000000000, 1.000000000000000000 ) ) ;
#31123 = DIRECTION ( 'NONE',  ( -1.000000000000000000, -0.000000000000000000, -0.000000000000000000 ) ) ;
#31124 = PLANE ( 'NONE',  #3392 ) ;
#31125 = CARTESIAN_POINT ( 'NONE',  ( -3.961125083139900749, -143.2122702051246677, 5.500000000000000000 ) ) ;
#31126 = EDGE_CURVE ( 'NONE', #17075, #1904, #22109, .T. ) ;
#31127 = DIRECTION ( 'NONE',  ( 0.000000000000000000, 0.8090169943749486725, -0.5877852522924713607 ) ) ;
#31128 = EDGE_CURVE ( 'NONE', #28820, #9321, #42146, .T. ) ;
#31129 = CARTESIAN_POINT ( 'NONE',  ( 0.000000000000000000, 17.67226234102874116, -33.17418723428288274 ) ) ;
#31130 = AXIS2_PLACEMENT_3D ( 'NONE', #1728, #38944, #5397 ) ;
#31131 = ORIENTED_EDGE ( 'NONE', *, *, #11842, .F. ) ;
#31132 = CARTESIAN_POINT ( 'NONE',  ( 10.00000000000000000, 0.000000000000000000, 0.000000000000000000 ) ) ;
#31133 = ADVANCED_FACE ( 'NONE', ( #27711 ), #35527, .T. ) ;
#31134 = CARTESIAN_POINT ( 'NONE',  ( 10.00000000000000000, -31.47745569255092235, -68.26794271651296242 ) ) ;
#31135 = DIRECTION ( 'NONE',  ( 0.000000000000000000, 0.000000000000000000, -1.000000000000000000 ) ) ;
#31136 = VECTOR ( 'NONE', #33816, 1000.000000000000000 ) ;
#31137 = FACE_OUTER_BOUND ( 'NONE', #26012, .T. ) ;
#31138 = DIRECTION ( 'NONE',  ( 0.000000000000000000, -0.2079116908177532363, -0.9781476007338069101 ) ) ;
#31140 = CIRCLE ( 'NONE', #7670, 32.00000000000000000 ) ;
#31139 = CARTESIAN_POINT ( 'NONE',  ( 10.00000000000000000, 34.44570377933695227, -69.42325613327405165 ) ) ;
#31141 = EDGE_LOOP ( 'NONE', ( #18990, #35546, #556, #1170 ) ) ;
#31142 = ADVANCED_FACE ( 'NONE', ( #9102 ), #26994, .T. ) ;
#31143 = ORIENTED_EDGE ( 'NONE', *, *, #2414, .T. ) ;
#31144 = CARTESIAN_POINT ( 'NONE',  ( 10.00000000000000000, 28.89263327155746097, 71.91182617369197771 ) ) ;
#31145 = ORIENTED_EDGE ( 'NONE', *, *, #24569, .T. ) ;
#31146 = ADVANCED_FACE ( 'NONE', ( #31635 ), #16682, .T. ) ;
#31147 = DIRECTION ( 'NONE',  ( -1.000000000000000000, 0.000000000000000000, 0.000000000000000000 ) ) ;
#31148 = SHAPE_DEFINITION_REPRESENTATION ( #19804, #12525 ) ;
#31149 = CARTESIAN_POINT ( 'NONE',  ( 10.00000000000000000, 41.19522573413731692, 65.64334221924924861 ) ) ;
#31150 = ORIENTED_EDGE ( 'NONE', *, *, #17228, .F. ) ;
#31151 = AXIS2_PLACEMENT_3D ( 'NONE', #20331, #20833, #28407 ) ;
#31152 = EDGE_CURVE ( 'NONE', #47426, #38615, #12066, .T. ) ;
#31153 = ORIENTED_EDGE ( 'NONE', *, *, #21419, .F. ) ;
#31154 = CARTESIAN_POINT ( 'NONE',  ( 0.000000000000000000, -9.188173127307592836, 40.98264845739746676 ) ) ;
#31155 = ORIENTED_EDGE ( 'NONE', *, *, #36824, .T. ) ;
#31156 = CARTESIAN_POINT ( 'NONE',  ( 0.000000000000000000, -120.0000000000000000, -40.00000000000000711 ) ) ;
#31157 = EDGE_CURVE ( 'NONE', #31088, #25106, #47134, .T. ) ;
#31158 = LINE ( 'NONE', #1531, #30007 ) ;
#31159 = FACE_OUTER_BOUND ( 'NONE', #20369, .T. ) ;
#31160 = ORIENTED_EDGE ( 'NONE', *, *, #561, .F. ) ;
#31162 = ORIENTED_EDGE ( 'NONE', *, *, #40768, .T. ) ;
#31161 = CARTESIAN_POINT ( 'NONE',  ( -21.67772167707813935, -110.8034581014852762, 2.500000000000000000 ) ) ;
#31163 = ORIENTED_EDGE ( 'NONE', *, *, #14480, .F. ) ;
#31164 = AXIS2_PLACEMENT_3D ( 'NONE', #42789, #20015, #5576 ) ;
#31165 = VECTOR ( 'NONE', #33219, 1000.000000000000114 ) ;
#31166 = VECTOR ( 'NONE', #41038, 1000.000000000000114 ) ;
#31167 = DIRECTION ( 'NONE',  ( 0.000000000000000000, 0.000000000000000000, 1.000000000000000000 ) ) ;
#31168 = CARTESIAN_POINT ( 'NONE',  ( 0.000000000000000000, 26.79245525562714292, 32.34446384429980981 ) ) ;
#31169 = DIRECTION ( 'NONE',  ( 0.000000000000000000, 0.000000000000000000, 1.000000000000000000 ) ) ;
#31170 = FACE_OUTER_BOUND ( 'NONE', #41114, .T. ) ;
#31172 = ORIENTED_EDGE ( 'NONE', *, *, #5142, .F. ) ;
#31171 = CARTESIAN_POINT ( 'NONE',  ( 12.49999999999999645, 1.530808498934191127E-15, 125.0000000000000000 ) ) ;
#31173 = EDGE_LOOP ( 'NONE', ( #39804, #43670, #20062, #22107, #34602, #34044 ) ) ;
#31174 = DIRECTION ( 'NONE',  ( 1.000000000000000000, 0.000000000000000000, 0.000000000000000000 ) ) ;
#31175 = VERTEX_POINT ( 'NONE', #8845 ) ;
#31176 = ORIENTED_EDGE ( 'NONE', *, *, #38017, .F. ) ;
#31177 = EDGE_CURVE ( 'NONE', #35793, #24691, #12306, .T. ) ;
#31178 = FACE_OUTER_BOUND ( 'NONE', #20174, .T. ) ;
#31179 = ORIENTED_EDGE ( 'NONE', *, *, #6507, .F. ) ;
#31180 = EDGE_CURVE ( 'NONE', #26444, #33012, #33084, .T. ) ;
#31181 = DIRECTION ( 'NONE',  ( -1.000000000000000000, -0.000000000000000000, 0.000000000000000000 ) ) ;
#31182 = DIRECTION ( 'NONE',  ( 0.000000000000000000, 0.000000000000000000, 1.000000000000000000 ) ) ;
#31183 = CARTESIAN_POINT ( 'NONE',  ( 11.99999999999999822, 0.000000000000000000, 0.000000000000000000 ) ) ;
#31184 = ORIENTED_EDGE ( 'NONE', *, *, #38812, .F. ) ;
#31185 = ADVANCED_FACE ( 'NONE', ( #21059 ), #10047, .T. ) ;
#31186 = FACE_OUTER_BOUND ( 'NONE', #39315, .T. ) ;
#31187 = DIRECTION ( 'NONE',  ( 1.000000000000000000, -0.000000000000000000, -0.000000000000000000 ) ) ;
#31188 = EDGE_CURVE ( 'NONE', #32575, #12049, #4939, .T. ) ;
#31189 = CARTESIAN_POINT ( 'NONE',  ( 10.00000000000000000, 0.000000000000000000, 0.000000000000000000 ) ) ;
#31190 = CARTESIAN_POINT ( 'NONE',  ( 11.99999999999999822, 0.000000000000000000, 0.000000000000000000 ) ) ;
#31191 = FACE_OUTER_BOUND ( 'NONE', #33252, .T. ) ;
#31192 = CARTESIAN_POINT ( 'NONE',  ( 0.000000000000000000, -13.04903810567647682, -19.60159698893442481 ) ) ;
#31194 = EDGE_CURVE ( 'NONE', #18006, #29561, #1282, .T. ) ;
#31193 = DIRECTION ( 'NONE',  ( 0.000000000000000000, 0.000000000000000000, 1.000000000000000000 ) ) ;
#31195 = FACE_OUTER_BOUND ( 'NONE', #18248, .T. ) ;
#31196 = CARTESIAN_POINT ( 'NONE',  ( -3.000000000000000000, 5.835314593368772229, -22.81335362449846826 ) ) ;
#31197 = CYLINDRICAL_SURFACE ( 'NONE', #22940, 82.00000000000000000 ) ;
#31198 = EDGE_LOOP ( 'NONE', ( #17443, #45577, #46512, #34364 ) ) ;
#31199 = ORIENTED_EDGE ( 'NONE', *, *, #22325, .F. ) ;
#31200 = DIRECTION ( 'NONE',  ( -1.000000000000000000, 0.000000000000000000, -0.000000000000000000 ) ) ;
#31201 = EDGE_LOOP ( 'NONE', ( #24459, #5976, #19825, #21184 ) ) ;
#31202 = ORIENTED_EDGE ( 'NONE', *, *, #2653, .F. ) ;
#31203 = CARTESIAN_POINT ( 'NONE',  ( -34.02017708624680381, -109.8571428571428470, 2.500000000000000000 ) ) ;
#31204 = VECTOR ( 'NONE', #44963, 1000.000000000000000 ) ;
#31205 = CIRCLE ( 'NONE', #32746, 31.99999999999998579 ) ;
#31206 = DIRECTION ( 'NONE',  ( 1.000000000000000000, 0.000000000000000000, 0.000000000000000000 ) ) ;
#31207 = ORIENTED_EDGE ( 'NONE', *, *, #45700, .F. ) ;
#31208 = ADVANCED_FACE ( 'NONE', ( #27470 ), #40164, .T. ) ;
#31209 = ORIENTED_EDGE ( 'NONE', *, *, #27223, .T. ) ;
#31210 = VERTEX_POINT ( 'NONE', #6627 ) ;
#31211 = ADVANCED_FACE ( 'NONE', ( #40411 ), #17151, .T. ) ;
#31212 = ORIENTED_EDGE ( 'NONE', *, *, #1704, .F. ) ;
#31213 = AXIS2_PLACEMENT_3D ( 'NONE', #16434, #31873, #46788 ) ;
#31214 = EDGE_CURVE ( 'NONE', #960, #21976, #43265, .T. ) ;
#31215 = CARTESIAN_POINT ( 'NONE',  ( 10.00000000000000000, 30.80686688397041451, -21.53537804866048688 ) ) ;
#31216 = DIRECTION ( 'NONE',  ( 0.02332147558787931590, 0.9997280174009348652, -0.000000000000000000 ) ) ;
#31218 = ORIENTED_EDGE ( 'NONE', *, *, #146, .T. ) ;
#31217 = CARTESIAN_POINT ( 'NONE',  ( 11.99999999999999822, 0.000000000000000000, 0.000000000000000000 ) ) ;
#31219 = VERTEX_POINT ( 'NONE', #47270 ) ;
#31220 = CARTESIAN_POINT ( 'NONE',  ( 11.99999999999999822, -62.50884508063453637, 41.76106447765467777 ) ) ;
#31221 = ORIENTED_EDGE ( 'NONE', *, *, #47902, .T. ) ;
#31222 = ORIENTED_EDGE ( 'NONE', *, *, #29940, .T. ) ;
#31223 = CARTESIAN_POINT ( 'NONE',  ( 0.000000000000000000, 0.000000000000000000, -54.99999999999998579 ) ) ;
#31224 = CYLINDRICAL_SURFACE ( 'NONE', #40341, 82.00000000000000000 ) ;
#31225 = DIRECTION ( 'NONE',  ( -1.000000000000000000, 0.000000000000000000, -0.000000000000000000 ) ) ;
#31226 = CIRCLE ( 'NONE', #32038, 82.00000000000000000 ) ;
#31227 = ORIENTED_EDGE ( 'NONE', *, *, #3609, .T. ) ;
#31228 = ORIENTED_EDGE ( 'NONE', *, *, #21709, .T. ) ;
#31229 = VECTOR ( 'NONE', #19443, 1000.000000000000000 ) ;
#31230 = CARTESIAN_POINT ( 'NONE',  ( 5.000000000000002665, 81.34940948281337114, 10.30890764327411979 ) ) ;
#31231 = ORIENTED_EDGE ( 'NONE', *, *, #37310, .F. ) ;
#31232 = EDGE_CURVE ( 'NONE', #35055, #27526, #17636, .T. ) ;
#31233 = LINE ( 'NONE', #1605, #30930 ) ;
#31234 = VECTOR ( 'NONE', #22699, 1000.000000000000000 ) ;
#31235 = CARTESIAN_POINT ( 'NONE',  ( 0.000000000000000000, 77.16300072079700101, -27.74655509720590985 ) ) ;
#31236 = DIRECTION ( 'NONE',  ( -1.000000000000000000, -0.000000000000000000, -0.000000000000000000 ) ) ;
#31237 = CARTESIAN_POINT ( 'NONE',  ( 23.49916127795269460, -121.5130826919798039, 5.500000000000000000 ) ) ;
#31238 = DIRECTION ( 'NONE',  ( -1.000000000000000000, -0.000000000000000000, 0.000000000000000000 ) ) ;
#31239 = EDGE_CURVE ( 'NONE', #31422, #43255, #22148, .T. ) ;
#31240 = DIRECTION ( 'NONE',  ( -1.000000000000000000, 0.000000000000000000, -0.000000000000000000 ) ) ;
#31241 = DIRECTION ( 'NONE',  ( 0.000000000000000000, 0.000000000000000000, 1.000000000000000000 ) ) ;
#31242 = ORIENTED_EDGE ( 'NONE', *, *, #37322, .T. ) ;
#31243 = CARTESIAN_POINT ( 'NONE',  ( -0.9515373497862389396, -96.47140937769621871, 5.500000000000000000 ) ) ;
#31244 = CYLINDRICAL_SURFACE ( 'NONE', #45737, 16.00000000000000000 ) ;
#31245 = CARTESIAN_POINT ( 'NONE',  ( 0.000000000000000000, 0.000000000000000000, 0.000000000000000000 ) ) ;
#31246 = PLANE ( 'NONE',  #16840 ) ;
#31247 = ORIENTED_EDGE ( 'NONE', *, *, #37250, .T. ) ;
#31248 = AXIS2_PLACEMENT_3D ( 'NONE', #22116, #37297, #21870 ) ;
#31250 = ADVANCED_FACE ( 'NONE', ( #29126 ), #39922, .F. ) ;
#31249 = DIRECTION ( 'NONE',  ( -0.000000000000000000, -0.000000000000000000, -1.000000000000000000 ) ) ;
#31251 = DIRECTION ( 'NONE',  ( -1.000000000000000000, 0.000000000000000000, -0.000000000000000000 ) ) ;
#31252 = EDGE_CURVE ( 'NONE', #31274, #9220, #10412, .T. ) ;
#31253 = DIRECTION ( 'NONE',  ( 0.000000000000000000, 0.000000000000000000, 1.000000000000000000 ) ) ;
#31254 = CARTESIAN_POINT ( 'NONE',  ( 0.000000000000000000, 58.39081064771751528, 50.95692526931350841 ) ) ;
#31255 = CARTESIAN_POINT ( 'NONE',  ( 15.00000000000000000, -0.9646360437372099028, 23.52805723605590771 ) ) ;
#31256 = CARTESIAN_POINT ( 'NONE',  ( -10.00000000000000000, 0.000000000000000000, 0.000000000000000000 ) ) ;
#31257 = DIRECTION ( 'NONE',  ( 0.000000000000000000, 0.000000000000000000, 1.000000000000000000 ) ) ;
#31258 = DIRECTION ( 'NONE',  ( 0.000000000000000000, 0.000000000000000000, 1.000000000000000000 ) ) ;
#31259 = ORIENTED_EDGE ( 'NONE', *, *, #23250, .F. ) ;
#31260 = SHAPE_REPRESENTATION ( 'big gear_ISO - Spur gear 2M 80T 20PA 10FW ---S80A75H50L20.0N', ( #11636 ), #725 ) ;
#31261 = ORIENTED_EDGE ( 'NONE', *, *, #15276, .F. ) ;
#31262 = SURFACE_STYLE_FILL_AREA ( #24147 ) ;
#31263 = LINE ( 'NONE', #12653, #1773 ) ;
#31264 = ORIENTED_EDGE ( 'NONE', *, *, #23695, .F. ) ;
#31265 = ORIENTED_EDGE ( 'NONE', *, *, #32346, .T. ) ;
#31266 = AXIS2_PLACEMENT_3D ( 'NONE', #27945, #43094, #20319 ) ;
#31267 = EDGE_LOOP ( 'NONE', ( #4612, #40630 ) ) ;
#31268 = AXIS2_PLACEMENT_3D ( 'NONE', #31947, #16764, #31714 ) ;
#31269 = ORIENTED_EDGE ( 'NONE', *, *, #2701, .T. ) ;
#31270 = AXIS2_PLACEMENT_3D ( 'NONE', #5931, #13497, #20849 ) ;
#31271 = CARTESIAN_POINT ( 'NONE',  ( 10.00000000000000000, 0.000000000000000000, 0.000000000000000000 ) ) ;
#31272 = ORIENTED_EDGE ( 'NONE', *, *, #2324, .F. ) ;
#31273 = STYLED_ITEM ( 'NONE', ( #33921 ), #19494 ) ;
#31274 = VERTEX_POINT ( 'NONE', #32573 ) ;
#31275 = VECTOR ( 'NONE', #32823, 1000.000000000000000 ) ;
#31276 = FACE_OUTER_BOUND ( 'NONE', #40326, .T. ) ;
#31277 = DIRECTION ( 'NONE',  ( 0.000000000000000000, 0.000000000000000000, 1.000000000000000000 ) ) ;
#31278 = ADVANCED_FACE ( 'NONE', ( #43822 ), #32794, .F. ) ;
#31279 = ORIENTED_EDGE ( 'NONE', *, *, #953, .T. ) ;
#31280 = ORIENTED_EDGE ( 'NONE', *, *, #1158, .T. ) ;
#31281 = ADVANCED_FACE ( 'NONE', ( #47495 ), #28417, .T. ) ;
#31282 = LINE ( 'NONE', #24166, #3754 ) ;
#31284 = ORIENTED_EDGE ( 'NONE', *, *, #45761, .T. ) ;
#31283 = DIRECTION ( 'NONE',  ( -0.9997280174009349762, 0.02332147558787671729, 0.000000000000000000 ) ) ;
#31285 = DIRECTION ( 'NONE',  ( 1.000000000000000000, 0.000000000000000000, 0.000000000000000000 ) ) ;
#31286 = ORIENTED_EDGE ( 'NONE', *, *, #38795, .F. ) ;
#31287 = ORIENTED_EDGE ( 'NONE', *, *, #31332, .F. ) ;
#31288 = DIRECTION ( 'NONE',  ( -0.9848077530122080203, -0.1736481776669309696, 0.000000000000000000 ) ) ;
#31289 = EDGE_LOOP ( 'NONE', ( #9131, #13454, #237, #1638 ) ) ;
#31290 = ORIENTED_EDGE ( 'NONE', *, *, #10842, .T. ) ;
#31291 = DIRECTION ( 'NONE',  ( -0.000000000000000000, -0.000000000000000000, -1.000000000000000000 ) ) ;
#31292 = CARTESIAN_POINT ( 'NONE',  ( -3.000000000000000000, 23.59884966291521380, 12.14883922797262805 ) ) ;
#31293 = ORIENTED_EDGE ( 'NONE', *, *, #25734, .T. ) ;
#31294 = CYLINDRICAL_SURFACE ( 'NONE', #32273, 82.00000000000000000 ) ;
#31295 = LINE ( 'NONE', #46214, #7303 ) ;
#31296 = ADVANCED_FACE ( 'NONE', ( #28667 ), #21787, .F. ) ;
#31297 = CYLINDRICAL_SURFACE ( 'NONE', #20520, 77.49899999999999523 ) ;
#31298 = ORIENTED_EDGE ( 'NONE', *, *, #47895, .T. ) ;
#31299 = EDGE_CURVE ( 'NONE', #38112, #28664, #21346, .T. ) ;
#31300 = EDGE_CURVE ( 'NONE', #11246, #5925, #28887, .T. ) ;
#31301 = EDGE_LOOP ( 'NONE', ( #44161, #13692, #32698, #41799 ) ) ;
#31302 = DIRECTION ( 'NONE',  ( -1.000000000000000000, -0.000000000000000000, -0.000000000000000000 ) ) ;
#31303 = AXIS2_PLACEMENT_3D ( 'NONE', #6769, #21448, #33660 ) ;
#31304 = LINE ( 'NONE', #27378, #40717 ) ;
#31305 = VERTEX_POINT ( 'NONE', #31879 ) ;
#31306 = DIRECTION ( 'NONE',  ( 0.000000000000000000, 0.000000000000000000, 1.000000000000000000 ) ) ;
#31307 = ORIENTED_EDGE ( 'NONE', *, *, #39233, .T. ) ;
#31308 = CIRCLE ( 'NONE', #19521, 12.79999999999999893 ) ;
#31309 = DIRECTION ( 'NONE',  ( -1.000000000000000000, 0.000000000000000000, 0.000000000000000000 ) ) ;
#31310 = DIRECTION ( 'NONE',  ( 1.000000000000000000, -0.000000000000000000, -0.000000000000000000 ) ) ;
#31311 = CARTESIAN_POINT ( 'NONE',  ( 0.000000000000000000, -37.22597642581161637, 5.202137450156258502 ) ) ;
#31312 = EDGE_CURVE ( 'NONE', #45678, #20008, #36481, .T. ) ;
#31313 = CARTESIAN_POINT ( 'NONE',  ( 0.000000000000000000, 46.54456581323888997, -59.03342792756214408 ) ) ;
#31314 = VECTOR ( 'NONE', #43207, 1000.000000000000000 ) ;
#31315 = DIRECTION ( 'NONE',  ( 0.000000000000000000, 0.000000000000000000, 1.000000000000000000 ) ) ;
#31316 = VECTOR ( 'NONE', #25072, 1000.000000000000000 ) ;
#31317 = DIRECTION ( 'NONE',  ( -1.000000000000000000, -0.000000000000000000, 0.000000000000000000 ) ) ;
#31318 = DIRECTION ( 'NONE',  ( -1.000000000000000000, -0.000000000000000000, -0.000000000000000000 ) ) ;
#31319 = AXIS2_PLACEMENT_3D ( 'NONE', #18575, #2917, #36451 ) ;
#31320 = DIRECTION ( 'NONE',  ( 0.000000000000000000, 0.000000000000000000, 1.000000000000000000 ) ) ;
#31321 = VERTEX_POINT ( 'NONE', #24755 ) ;
#31322 = CARTESIAN_POINT ( 'NONE',  ( 10.00000000000000000, 0.000000000000000000, 0.000000000000000000 ) ) ;
#31323 =( NAMED_UNIT ( * ) PLANE_ANGLE_UNIT ( ) SI_UNIT ( $, .RADIAN. ) );
#31324 = ORIENTED_EDGE ( 'NONE', *, *, #27420, .T. ) ;
#31325 = VERTEX_POINT ( 'NONE', #46794 ) ;
#31326 = CARTESIAN_POINT ( 'NONE',  ( 0.000000000000000000, 69.42325613327489009, -34.44570377933524696 ) ) ;
#31327 = FACE_OUTER_BOUND ( 'NONE', #38709, .T. ) ;
#31328 = FACE_OUTER_BOUND ( 'NONE', #17202, .T. ) ;
#31329 = VERTEX_POINT ( 'NONE', #2944 ) ;
#31330 = EDGE_CURVE ( 'NONE', #43018, #39693, #9561, .T. ) ;
#31331 = AXIS2_PLACEMENT_3D ( 'NONE', #341, #15518, #44895 ) ;
#31332 = EDGE_CURVE ( 'NONE', #19563, #16462, #10054, .T. ) ;
#31333 = CIRCLE ( 'NONE', #21134, 37.49900000000000233 ) ;
#31334 = DIRECTION ( 'NONE',  ( -1.000000000000000000, -0.000000000000000000, -0.000000000000000000 ) ) ;
#31335 = CIRCLE ( 'NONE', #21137, 11.59999999999999787 ) ;
#31336 = VECTOR ( 'NONE', #33059, 1000.000000000000000 ) ;
#31337 = ORIENTED_EDGE ( 'NONE', *, *, #4641, .T. ) ;
#31338 = ORIENTED_EDGE ( 'NONE', *, *, #31701, .T. ) ;
#31339 = EDGE_CURVE ( 'NONE', #6663, #30146, #29168, .T. ) ;
#31340 = ORIENTED_EDGE ( 'NONE', *, *, #45109, .F. ) ;
#31341 = EDGE_LOOP ( 'NONE', ( #25606, #29039, #14759, #32111 ) ) ;
#31342 = VERTEX_POINT ( 'NONE', #15426 ) ;
#31343 = ORIENTED_EDGE ( 'NONE', *, *, #21586, .T. ) ;
#31344 = ADVANCED_FACE ( 'NONE', ( #41135 ), #26194, .T. ) ;
#31345 = VECTOR ( 'NONE', #37716, 1000.000000000000114 ) ;
#31346 = AXIS2_PLACEMENT_3D ( 'NONE', #12336, #12569, #46335 ) ;
#31347 = DIRECTION ( 'NONE',  ( -1.000000000000000000, -0.000000000000000000, -0.000000000000000000 ) ) ;
#31348 = VECTOR ( 'NONE', #1435, 1000.000000000000000 ) ;
#31349 = ORIENTED_EDGE ( 'NONE', *, *, #41321, .T. ) ;
#31350 = CARTESIAN_POINT ( 'NONE',  ( 5.000000000000000000, 35.47612816024556537, -22.48208911017461631 ) ) ;
#31351 = ORIENTED_EDGE ( 'NONE', *, *, #22727, .T. ) ;
#31352 = DIRECTION ( 'NONE',  ( -1.000000000000000000, 0.000000000000000000, 0.000000000000000000 ) ) ;
#31353 = CARTESIAN_POINT ( 'NONE',  ( 10.00000000000000000, 16.00000000000000000, 2.500000000000000000 ) ) ;
#31354 = CARTESIAN_POINT ( 'NONE',  ( 0.000000000000000000, 0.000000000000000000, 0.000000000000000000 ) ) ;
#31355 = ORIENTED_EDGE ( 'NONE', *, *, #16091, .T. ) ;
#31356 = DIRECTION ( 'NONE',  ( 0.000000000000000000, -0.8090169943749402348, -0.5877852522924830181 ) ) ;
#31357 = EDGE_CURVE ( 'NONE', #43176, #33558, #22521, .T. ) ;
#31358 = ORIENTED_EDGE ( 'NONE', *, *, #46906, .F. ) ;
#31359 = DIRECTION ( 'NONE',  ( 1.000000000000000000, 0.000000000000000000, 0.000000000000000000 ) ) ;
#31360 = CYLINDRICAL_SURFACE ( 'NONE', #19558, 37.49900000000000233 ) ;
#31361 = ORIENTED_EDGE ( 'NONE', *, *, #23342, .T. ) ;
#31362 = CARTESIAN_POINT ( 'NONE',  ( 10.00000000000000000, -2.946379043146863719, 75.11764819372146462 ) ) ;
#31363 = ORIENTED_EDGE ( 'NONE', *, *, #15133, .T. ) ;
#31364 = VERTEX_POINT ( 'NONE', #10785 ) ;
#31365 = DIRECTION ( 'NONE',  ( -1.000000000000000000, -0.000000000000000000, 0.000000000000000000 ) ) ;
#31366 = DIRECTION ( 'NONE',  ( -1.000000000000000000, 0.000000000000000000, 0.000000000000000000 ) ) ;
#31367 = CARTESIAN_POINT ( 'NONE',  ( 0.000000000000000000, -73.73191006444582740, 14.66109333815435889 ) ) ;
#31368 = CARTESIAN_POINT ( 'NONE',  ( 10.00000000000000000, 0.000000000000000000, 0.000000000000000000 ) ) ;
#31369 = CARTESIAN_POINT ( 'NONE',  ( 11.99999999999999822, -65.64334221924882229, -41.19522573413803457 ) ) ;
#31370 = LINE ( 'NONE', #20821, #16373 ) ;
#31371 = DIRECTION ( 'NONE',  ( -1.000000000000000000, -0.000000000000000000, -0.000000000000000000 ) ) ;
#31372 = EDGE_CURVE ( 'NONE', #42048, #31422, #12765, .T. ) ;
#31374 = AXIS2_PLACEMENT_3D ( 'NONE', #23516, #38953, #42370 ) ;
#31373 = DIRECTION ( 'NONE',  ( -1.000000000000000000, 0.000000000000000000, 0.000000000000000000 ) ) ;
#31375 = VERTEX_POINT ( 'NONE', #37448 ) ;
#31376 = VECTOR ( 'NONE', #34682, 1000.000000000000000 ) ;
#31377 = CARTESIAN_POINT ( 'NONE',  ( 0.000000000000000000, 30.00120703465205452, 22.64427369931179967 ) ) ;
#31378 = CARTESIAN_POINT ( 'NONE',  ( 0.000000000000000000, -40.98264845739755202, 9.188173127307159405 ) ) ;
#31379 = DIRECTION ( 'NONE',  ( -1.000000000000000000, 0.000000000000000000, -0.000000000000000000 ) ) ;
#31380 = CIRCLE ( 'NONE', #43860, 31.99999999999998934 ) ;
#31381 = CIRCLE ( 'NONE', #27456, 82.00000000000000000 ) ;
#31382 = ORIENTED_EDGE ( 'NONE', *, *, #34966, .T. ) ;
#31383 = CARTESIAN_POINT ( 'NONE',  ( 0.000000000000000000, -77.19088730480527261, 6.903761155837504049 ) ) ;
#31384 = CARTESIAN_POINT ( 'NONE',  ( 10.00000000000000000, -77.16300072079680206, 27.74655509720639657 ) ) ;
#31385 = FACE_OUTER_BOUND ( 'NONE', #47355, .T. ) ;
#31386 = CARTESIAN_POINT ( 'NONE',  ( 6.377742925735834234, -145.7647898336708181, 5.500000000000000000 ) ) ;
#31387 = AXIS2_PLACEMENT_3D ( 'NONE', #8033, #34456, #22968 ) ;
#31388 = ORIENTED_EDGE ( 'NONE', *, *, #25984, .F. ) ;
#31389 = CIRCLE ( 'NONE', #10247, 12.49999999999999645 ) ;
#31390 = ORIENTED_EDGE ( 'NONE', *, *, #2390, .F. ) ;
#31391 = DIRECTION ( 'NONE',  ( -1.000000000000000000, 0.000000000000000000, -0.000000000000000000 ) ) ;
#31392 = AXIS2_PLACEMENT_3D ( 'NONE', #7975, #642, #37604 ) ;
#31393 = CARTESIAN_POINT ( 'NONE',  ( 6.000000000000000000, 81.34940948281351325, -10.30890764327295450 ) ) ;
#31394 = CARTESIAN_POINT ( 'NONE',  ( 0.000000000000000000, 80.55351364060611274, -15.33399622253396544 ) ) ;
#31395 = ORIENTED_EDGE ( 'NONE', *, *, #37982, .T. ) ;
#31396 = ADVANCED_FACE ( 'NONE', ( #7823 ), #29616, .T. ) ;
#31397 = DIRECTION ( 'NONE',  ( -1.000000000000000000, 0.000000000000000000, 0.000000000000000000 ) ) ;
#31398 = ADVANCED_FACE ( 'NONE', ( #44311 ), #11515, .T. ) ;
#31399 = EDGE_LOOP ( 'NONE', ( #44142, #46167, #39864, #43537 ) ) ;
#31400 = CARTESIAN_POINT ( 'NONE',  ( 11.99999999999999822, 46.21855187248719687, -62.20884554313968806 ) ) ;
#31401 = ADVANCED_FACE ( 'NONE', ( #7097 ), #33291, .T. ) ;
#31402 = AXIS2_PLACEMENT_3D ( 'NONE', #44476, #25385, #47649 ) ;
#31403 = DIRECTION ( 'NONE',  ( -1.000000000000000000, -0.000000000000000000, 0.000000000000000000 ) ) ;
#31404 = AXIS2_PLACEMENT_3D ( 'NONE', #27798, #5509, #42225 ) ;
#31405 = CARTESIAN_POINT ( 'NONE',  ( 5.000000000000000000, 16.65560815589464028, -38.55633173626993226 ) ) ;
#31406 = ORIENTED_EDGE ( 'NONE', *, *, #25522, .F. ) ;
#31407 = LINE ( 'NONE', #27729, #44989 ) ;
#31408 = AXIS2_PLACEMENT_3D ( 'NONE', #4557, #15568, #30274 ) ;
#31409 = CIRCLE ( 'NONE', #43100, 16.00000000000000000 ) ;
#31410 = ORIENTED_EDGE ( 'NONE', *, *, #13217, .T. ) ;
#31411 = VERTEX_POINT ( 'NONE', #18828 ) ;
#31412 = FACE_BOUND ( 'NONE', #32283, .T. ) ;
#31413 = AXIS2_PLACEMENT_3D ( 'NONE', #8698, #37850, #12632 ) ;
#31414 = EDGE_CURVE ( 'NONE', #28248, #34700, #24497, .T. ) ;
#31415 = DIRECTION ( 'NONE',  ( 0.000000000000000000, 0.000000000000000000, 1.000000000000000000 ) ) ;
#31416 = CARTESIAN_POINT ( 'NONE',  ( 11.99999999999999822, 0.000000000000000000, 0.000000000000000000 ) ) ;
#31417 = EDGE_CURVE ( 'NONE', #15994, #2489, #44018, .T. ) ;
#31418 = DIRECTION ( 'NONE',  ( -1.000000000000000000, 0.000000000000000000, -0.000000000000000000 ) ) ;
#31419 = CYLINDRICAL_SURFACE ( 'NONE', #3904, 82.00000000000000000 ) ;
#31420 = ORIENTED_EDGE ( 'NONE', *, *, #47557, .T. ) ;
#31421 = CARTESIAN_POINT ( 'NONE',  ( -12.50000000000000000, -132.5000000000000000, 40.00000000000000000 ) ) ;
#31422 = VERTEX_POINT ( 'NONE', #36945 ) ;
#31423 = VERTEX_POINT ( 'NONE', #33760 ) ;
#31424 = EDGE_CURVE ( 'NONE', #20505, #1277, #3419, .T. ) ;
#31425 = FACE_OUTER_BOUND ( 'NONE', #34555, .T. ) ;
#31426 = VERTEX_POINT ( 'NONE', #226 ) ;
#31427 = CARTESIAN_POINT ( 'NONE',  ( -10.00000000000000000, 0.000000000000000000, 0.000000000000000000 ) ) ;
#31428 = DIRECTION ( 'NONE',  ( 0.000000000000000000, -0.7604059656000369261, 0.6494480483301766638 ) ) ;
#31429 = CARTESIAN_POINT ( 'NONE',  ( 0.000000000000000000, -120.0000000000000000, -2.500000000000000000 ) ) ;
#31430 = ORIENTED_EDGE ( 'NONE', *, *, #22714, .T. ) ;
#31431 = CARTESIAN_POINT ( 'NONE',  ( 11.99999999999999822, 51.29473840253223216, 63.97538442413446091 ) ) ;
#31432 = DIRECTION ( 'NONE',  ( -0.000000000000000000, 0.7431448254773946882, -0.6691306063588577935 ) ) ;
#31433 = FACE_OUTER_BOUND ( 'NONE', #39163, .T. ) ;
#31434 = CARTESIAN_POINT ( 'NONE',  ( -2.500000000000000000, 16.00000000000000000, -19.01812422950394676 ) ) ;
#31435 = EDGE_CURVE ( 'NONE', #40433, #14416, #25247, .T. ) ;
#31436 = CARTESIAN_POINT ( 'NONE',  ( 11.99999999999999822, 0.000000000000000000, 0.000000000000000000 ) ) ;
#31437 = DIRECTION ( 'NONE',  ( -1.000000000000000000, 0.000000000000000000, 0.000000000000000000 ) ) ;
#31438 = CARTESIAN_POINT ( 'NONE',  ( 5.000000000000002665, 81.50828551894240093, -8.966570791699803422 ) ) ;
#31439 = CARTESIAN_POINT ( 'NONE',  ( 25.81725066941077529, -113.8380548628854854, 5.500000000000000000 ) ) ;
#31440 = DIRECTION ( 'NONE',  ( 1.000000000000000000, 0.000000000000000000, 0.000000000000000000 ) ) ;
#31441 = DIRECTION ( 'NONE',  ( 0.000000000000000000, 0.9723699203976773342, -0.2334453638559023381 ) ) ;
#31442 = ORIENTED_EDGE ( 'NONE', *, *, #25767, .T. ) ;
#31443 = DIRECTION ( 'NONE',  ( 0.000000000000000000, 1.000000000000000000, 3.491481338843133750E-15 ) ) ;
#31444 = ORIENTED_EDGE ( 'NONE', *, *, #9055, .F. ) ;
#31445 = DIRECTION ( 'NONE',  ( 1.000000000000000000, 0.000000000000000000, 0.000000000000000000 ) ) ;
#31446 = AXIS2_PLACEMENT_3D ( 'NONE', #20865, #35786, #2250 ) ;
#31447 = CARTESIAN_POINT ( 'NONE',  ( 10.00000000000000000, 0.000000000000000000, 0.000000000000000000 ) ) ;
#31448 = CIRCLE ( 'NONE', #14231, 77.49899999999999523 ) ;
#31449 = EDGE_LOOP ( 'NONE', ( #21477, #45679, #4428, #48408 ) ) ;
#31450 = AXIS2_PLACEMENT_3D ( 'NONE', #35237, #29092, #2908 ) ;
#31451 = DIRECTION ( 'NONE',  ( 0.000000000000000000, 1.000000000000000000, 3.469446951953616555E-15 ) ) ;
#31452 = EDGE_CURVE ( 'NONE', #33441, #6365, #37686, .T. ) ;
#31453 = EDGE_LOOP ( 'NONE', ( #10056, #22846, #7248, #34951 ) ) ;
#31454 = ADVANCED_FACE ( 'NONE', ( #40631 ), #18360, .T. ) ;
#31455 = EDGE_LOOP ( 'NONE', ( #47918, #26980, #17478, #6059 ) ) ;
#31456 = EDGE_CURVE ( 'NONE', #32306, #13449, #2664, .T. ) ;
#31457 = EDGE_CURVE ( 'NONE', #21073, #26395, #8931, .T. ) ;
#31458 = CARTESIAN_POINT ( 'NONE',  ( 11.99999999999999822, -10.30890764327441289, 81.34940948281332851 ) ) ;
#31459 = ADVANCED_FACE ( 'NONE', ( #22750 ), #4165, .T. ) ;
#31460 = DIRECTION ( 'NONE',  ( -1.000000000000000000, -0.000000000000000000, -0.000000000000000000 ) ) ;
#31462 = ORIENTED_EDGE ( 'NONE', *, *, #43057, .T. ) ;
#31461 = DIRECTION ( 'NONE',  ( -1.000000000000000000, 0.000000000000000000, -0.000000000000000000 ) ) ;
#31463 = ORIENTED_EDGE ( 'NONE', *, *, #15191, .F. ) ;
#31464 = CYLINDRICAL_SURFACE ( 'NONE', #3966, 31.99999999999998579 ) ;
#31465 = ORIENTED_EDGE ( 'NONE', *, *, #45162, .T. ) ;
#31466 = DIRECTION ( 'NONE',  ( 0.000000000000000000, 0.000000000000000000, 1.000000000000000000 ) ) ;
#31467 = CYLINDRICAL_SURFACE ( 'NONE', #13742, 42.00000000000000000 ) ;
#31468 = DIRECTION ( 'NONE',  ( -0.000000000000000000, 0.6691306063588672304, 0.7431448254773862505 ) ) ;
#31469 = AXIS2_PLACEMENT_3D ( 'NONE', #45921, #47528, #13109 ) ;
#31470 = EDGE_LOOP ( 'NONE', ( #1527, #26946, #37852, #31293 ) ) ;
#31471 = ORIENTED_EDGE ( 'NONE', *, *, #9048, .F. ) ;
#31472 = PLANE ( 'NONE',  #3679 ) ;
#31473 = ORIENTED_EDGE ( 'NONE', *, *, #12225, .F. ) ;
#31474 = ADVANCED_FACE ( 'NONE', ( #38672 ), #34727, .T. ) ;
#31475 = VECTOR ( 'NONE', #10020, 1000.000000000000000 ) ;
#31476 = DIRECTION ( 'NONE',  ( -1.000000000000000000, -0.000000000000000000, 0.000000000000000000 ) ) ;
#31477 = DIRECTION ( 'NONE',  ( 1.000000000000000000, 0.000000000000000000, 0.000000000000000000 ) ) ;
#31478 = CARTESIAN_POINT ( 'NONE',  ( 15.00000000000000000, -23.29833615347104470, 3.418703333116808629 ) ) ;
#31479 = DIRECTION ( 'NONE',  ( 0.000000000000000000, 0.000000000000000000, -1.000000000000000000 ) ) ;
#31480 = DIRECTION ( 'NONE',  ( 1.000000000000000000, 0.000000000000000000, 0.000000000000000000 ) ) ;
#31481 = CARTESIAN_POINT ( 'NONE',  ( 0.000000000000000000, 0.000000000000000000, 0.000000000000000000 ) ) ;
#31482 = VECTOR ( 'NONE', #2053, 1000.000000000000114 ) ;
#31483 = CARTESIAN_POINT ( 'NONE',  ( -3.000000000000000000, 16.61724383029361718, 20.69703378468926402 ) ) ;
#31484 = VERTEX_POINT ( 'NONE', #30583 ) ;
#31485 = CARTESIAN_POINT ( 'NONE',  ( 19.29194287201271862, -133.5026271600380880, 5.500000000000000000 ) ) ;
#31486 = FACE_OUTER_BOUND ( 'NONE', #39673, .T. ) ;
#31487 = CARTESIAN_POINT ( 'NONE',  ( 11.99999999999999822, -26.01480285779785362, -70.53064760720343429 ) ) ;
#31488 = EDGE_CURVE ( 'NONE', #5219, #5603, #1937, .T. ) ;
#31489 = FACE_OUTER_BOUND ( 'NONE', #5980, .T. ) ;
#31490 = VERTEX_POINT ( 'NONE', #41860 ) ;
#31491 = ORIENTED_EDGE ( 'NONE', *, *, #29576, .T. ) ;
#31492 = AXIS2_PLACEMENT_3D ( 'NONE', #9667, #24611, #14796 ) ;
#31493 = DIRECTION ( 'NONE',  ( -0.6064928550163511956, -0.7950889364178798102, 0.000000000000000000 ) ) ;
#31494 = LINE ( 'NONE', #30514, #37787 ) ;
#31495 = DIRECTION ( 'NONE',  ( -1.000000000000000000, 0.000000000000000000, 0.000000000000000000 ) ) ;
#31496 = DIRECTION ( 'NONE',  ( 1.000000000000000000, 0.000000000000000000, -0.000000000000000000 ) ) ;
#31497 = EDGE_CURVE ( 'NONE', #40640, #31364, #19093, .T. ) ;
#31498 = CYLINDRICAL_SURFACE ( 'NONE', #26358, 31.99999999999998579 ) ;
#31499 = CARTESIAN_POINT ( 'NONE',  ( -3.000000000000000000, 20.85821328998756385, -10.92862929874494959 ) ) ;
#31500 = ORIENTED_EDGE ( 'NONE', *, *, #2987, .F. ) ;
#31501 = CARTESIAN_POINT ( 'NONE',  ( 11.99999999999999822, -14.66109333815410487, -73.73191006444587003 ) ) ;
#31502 = CIRCLE ( 'NONE', #44748, 77.49899999999999523 ) ;
#31503 = ORIENTED_EDGE ( 'NONE', *, *, #41221, .T. ) ;
#31504 = VECTOR ( 'NONE', #38736, 1000.000000000000000 ) ;
#31505 =( NAMED_UNIT ( * ) SI_UNIT ( $, .STERADIAN. ) SOLID_ANGLE_UNIT ( ) );
#31506 = DIRECTION ( 'NONE',  ( -1.000000000000000000, -0.000000000000000000, -0.000000000000000000 ) ) ;
#31507 = ORIENTED_EDGE ( 'NONE', *, *, #31578, .T. ) ;
#31508 = ORIENTED_EDGE ( 'NONE', *, *, #27190, .F. ) ;
#31509 = AXIS2_PLACEMENT_3D ( 'NONE', #14449, #34001, #33031 ) ;
#31510 = EDGE_CURVE ( 'NONE', #8981, #20650, #37875, .T. ) ;
#31511 = CIRCLE ( 'NONE', #37747, 42.00000000000000000 ) ;
#31512 = EDGE_CURVE ( 'NONE', #47535, #44620, #43367, .T. ) ;
#31513 = VERTEX_POINT ( 'NONE', #23976 ) ;
#31514 = AXIS2_PLACEMENT_3D ( 'NONE', #22251, #37656, #18571 ) ;
#31515 = AXIS2_PLACEMENT_3D ( 'NONE', #21988, #11484, #15868 ) ;
#31516 = DIRECTION ( 'NONE',  ( -1.000000000000000000, -0.000000000000000000, 0.000000000000000000 ) ) ;
#31517 = ADVANCED_FACE ( 'NONE', ( #19319 ), #20045, .T. ) ;
#31518 = ORIENTED_EDGE ( 'NONE', *, *, #38914, .T. ) ;
#31519 = VECTOR ( 'NONE', #12460, 1000.000000000000000 ) ;
#31520 = ADVANCED_FACE ( 'NONE', ( #46009 ), #34976, .F. ) ;
#31521 = VERTEX_POINT ( 'NONE', #4414 ) ;
#31522 = EDGE_CURVE ( 'NONE', #28423, #32581, #42323, .T. ) ;
#31523 = FACE_OUTER_BOUND ( 'NONE', #19690, .T. ) ;
#31524 = CIRCLE ( 'NONE', #47123, 31.99999999999998579 ) ;
#31525 = LINE ( 'NONE', #6287, #2699 ) ;
#31526 = ORIENTED_EDGE ( 'NONE', *, *, #39638, .F. ) ;
#31527 = ORIENTED_EDGE ( 'NONE', *, *, #44216, .T. ) ;
#31528 = FACE_OUTER_BOUND ( 'NONE', #32782, .T. ) ;
#31530 = ORIENTED_EDGE ( 'NONE', *, *, #34918, .F. ) ;
#31529 = CARTESIAN_POINT ( 'NONE',  ( -0.1915406271734583221, -121.4877204670710427, -2.500000000000000000 ) ) ;
#31531 = DIRECTION ( 'NONE',  ( -1.000000000000000000, -0.000000000000000000, -0.000000000000000000 ) ) ;
#31532 = ORIENTED_EDGE ( 'NONE', *, *, #9891, .F. ) ;
#31533 = CARTESIAN_POINT ( 'NONE',  ( 10.00000000000000000, 10.41901085202135668, -40.68715046381917944 ) ) ;
#31534 = VERTEX_POINT ( 'NONE', #31326 ) ;
#31535 = ORIENTED_EDGE ( 'NONE', *, *, #19142, .T. ) ;
#31536 = CARTESIAN_POINT ( 'NONE',  ( 0.000000000000000000, -75.54627589209955829, 17.28742895386058009 ) ) ;
#31537 = DIRECTION ( 'NONE',  ( 0.000000000000000000, -0.9969173337331287410, 0.07845909572783495156 ) ) ;
#31538 = ORIENTED_EDGE ( 'NONE', *, *, #30915, .F. ) ;
#31539 = CARTESIAN_POINT ( 'NONE',  ( 0.000000000000000000, -31.52238457039619490, 27.75498641678731104 ) ) ;
#31540 = CARTESIAN_POINT ( 'NONE',  ( 11.99999999999999822, 0.000000000000000000, 0.000000000000000000 ) ) ;
#31541 = VECTOR ( 'NONE', #34794, 1000.000000000000000 ) ;
#31542 = CARTESIAN_POINT ( 'NONE',  ( 11.99999999999999822, 0.000000000000000000, 0.000000000000000000 ) ) ;
#31543 = ORIENTED_EDGE ( 'NONE', *, *, #20532, .T. ) ;
#31544 = ORIENTED_EDGE ( 'NONE', *, *, #24767, .T. ) ;
#31545 = CIRCLE ( 'NONE', #31509, 77.49899999999999523 ) ;
#31546 = DIRECTION ( 'NONE',  ( 0.000000000000000000, 0.000000000000000000, 1.000000000000000000 ) ) ;
#31547 = DIRECTION ( 'NONE',  ( 0.1276937514489694392, 0.9918136447140102341, -0.000000000000000000 ) ) ;
#31548 = VERTEX_POINT ( 'NONE', #46241 ) ;
#31549 = CARTESIAN_POINT ( 'NONE',  ( 6.000000000000000000, -16.65972982744876774, -80.28980883073775487 ) ) ;
#31550 = ORIENTED_EDGE ( 'NONE', *, *, #11344, .T. ) ;
#31551 = AXIS2_PLACEMENT_3D ( 'NONE', #40076, #14368, #6787 ) ;
#31552 = AXIS2_PLACEMENT_3D ( 'NONE', #9008, #12685, #27610 ) ;
#31553 = DIRECTION ( 'NONE',  ( -1.000000000000000000, -0.000000000000000000, 0.000000000000000000 ) ) ;
#31554 = LINE ( 'NONE', #12696, #39603 ) ;
#31555 = LINE ( 'NONE', #46478, #1094 ) ;
#31556 = CYLINDRICAL_SURFACE ( 'NONE', #42442, 31.99999999999999289 ) ;
#31557 = CIRCLE ( 'NONE', #29190, 16.00000000000000000 ) ;
#31558 = CYLINDRICAL_SURFACE ( 'NONE', #11918, 77.49899999999999523 ) ;
#31559 = DIRECTION ( 'NONE',  ( 0.000000000000000000, 0.000000000000000000, 1.000000000000000000 ) ) ;
#31560 = VECTOR ( 'NONE', #37514, 1000.000000000000000 ) ;
#31561 = FACE_OUTER_BOUND ( 'NONE', #40295, .T. ) ;
#31562 = DIRECTION ( 'NONE',  ( -1.000000000000000000, 0.000000000000000000, 0.000000000000000000 ) ) ;
#31563 = CARTESIAN_POINT ( 'NONE',  ( 0.000000000000000000, -20.41045688087876897, 72.35160999960810102 ) ) ;
#31564 = VECTOR ( 'NONE', #19360, 1000.000000000000000 ) ;
#31565 = DIRECTION ( 'NONE',  ( 0.000000000000000000, 0.000000000000000000, 1.000000000000000000 ) ) ;
#31566 = AXIS2_PLACEMENT_3D ( 'NONE', #9167, #16990, #28252 ) ;
#31567 = VERTEX_POINT ( 'NONE', #12710 ) ;
#31568 = ORIENTED_EDGE ( 'NONE', *, *, #6511, .F. ) ;
#31569 = EDGE_CURVE ( 'NONE', #17592, #33075, #42580, .T. ) ;
#31570 = ADVANCED_FACE ( 'NONE', ( #12244 ), #38909, .F. ) ;
#31571 = ADVANCED_BREP_SHAPE_REPRESENTATION ( '', ( #19734, #11636 ), #725 ) ;
#31572 = DIRECTION ( 'NONE',  ( 1.000000000000000000, 0.000000000000000000, 0.000000000000000000 ) ) ;
#31573 = EDGE_CURVE ( 'NONE', #28097, #46278, #45503, .T. ) ;
#31574 = CARTESIAN_POINT ( 'NONE',  ( 10.00000000000000000, 62.50884508063427347, 41.76106447765511831 ) ) ;
#31575 = ORIENTED_EDGE ( 'NONE', *, *, #12459, .T. ) ;
#31576 = AXIS2_PLACEMENT_3D ( 'NONE', #6329, #24440, #5857 ) ;
#31577 = EDGE_CURVE ( 'NONE', #6991, #17121, #26134, .T. ) ;
#31578 = EDGE_CURVE ( 'NONE', #16794, #23303, #30837, .T. ) ;
#31579 = LINE ( 'NONE', #8787, #6279 ) ;
#31580 = AXIS2_PLACEMENT_3D ( 'NONE', #34391, #45671, #31005 ) ;
#31581 = AXIS2_PLACEMENT_3D ( 'NONE', #3856, #30047, #44979 ) ;
#31582 = ORIENTED_EDGE ( 'NONE', *, *, #3030, .T. ) ;
#31583 = VERTEX_POINT ( 'NONE', #44468 ) ;
#31584 = EDGE_CURVE ( 'NONE', #11671, #45038, #22673, .T. ) ;
#31585 = EDGE_LOOP ( 'NONE', ( #17878, #25358, #40592, #42318 ) ) ;
#31586 = DIRECTION ( 'NONE',  ( -1.000000000000000000, 0.000000000000000000, 0.000000000000000000 ) ) ;
#31587 = ORIENTED_EDGE ( 'NONE', *, *, #32863, .T. ) ;
#31588 = AXIS2_PLACEMENT_3D ( 'NONE', #42888, #31889, #25944 ) ;
#31589 = CIRCLE ( 'NONE', #29228, 31.99999999999999289 ) ;
#31590 = VERTEX_POINT ( 'NONE', #4082 ) ;
#31591 = CYLINDRICAL_SURFACE ( 'NONE', #5168, 31.99999999999999289 ) ;
#31592 = ORIENTED_EDGE ( 'NONE', *, *, #26203, .F. ) ;
#31593 = VECTOR ( 'NONE', #45258, 1000.000000000000000 ) ;
#31594 = DIRECTION ( 'NONE',  ( -1.000000000000000000, -0.000000000000000000, 0.000000000000000000 ) ) ;
#31595 = CIRCLE ( 'NONE', #17484, 77.49900000000000944 ) ;
#31596 = CARTESIAN_POINT ( 'NONE',  ( 0.000000000000000000, 0.000000000000000000, 0.000000000000000000 ) ) ;
#31597 = DIRECTION ( 'NONE',  ( -1.000000000000000000, -0.000000000000000000, 0.000000000000000000 ) ) ;
#31599 = ORIENTED_EDGE ( 'NONE', *, *, #31510, .F. ) ;
#31598 = AXIS2_PLACEMENT_3D ( 'NONE', #18671, #2240, #38746 ) ;
#31600 = DIRECTION ( 'NONE',  ( 0.000000000000000000, 0.000000000000000000, 1.000000000000000000 ) ) ;
#31601 = ORIENTED_EDGE ( 'NONE', *, *, #38249, .T. ) ;
#31602 = DIRECTION ( 'NONE',  ( 0.000000000000000000, 0.2334453638558990629, 0.9723699203976782224 ) ) ;
#31603 = CARTESIAN_POINT ( 'NONE',  ( 10.00000000000000000, 27.75498641678742473, 31.52238457039609898 ) ) ;
#31604 = CARTESIAN_POINT ( 'NONE',  ( -3.000000000000000000, 24.81905959214261514, 9.408202855044825341 ) ) ;
#31605 = VERTEX_POINT ( 'NONE', #10939 ) ;
#31606 = ORIENTED_EDGE ( 'NONE', *, *, #5152, .T. ) ;
#31607 = CARTESIAN_POINT ( 'NONE',  ( 0.000000000000000000, 68.55367621811204515, -44.99326035065983120 ) ) ;
#31608 = CARTESIAN_POINT ( 'NONE',  ( 10.00000000000000000, 36.88895765772642932, -6.736453364083163642 ) ) ;
#31609 = FACE_OUTER_BOUND ( 'NONE', #9350, .T. ) ;
#31610 = CARTESIAN_POINT ( 'NONE',  ( 0.000000000000000000, 0.000000000000000000, 0.000000000000000000 ) ) ;
#31611 = DIRECTION ( 'NONE',  ( -1.000000000000000000, -0.000000000000000000, 0.000000000000000000 ) ) ;
#31612 = DIRECTION ( 'NONE',  ( 0.6691306063588671194, -0.7431448254773862505, 0.000000000000000000 ) ) ;
#31613 = DIRECTION ( 'NONE',  ( -1.000000000000000000, 0.000000000000000000, 0.000000000000000000 ) ) ;
#31614 = AXIS2_PLACEMENT_3D ( 'NONE', #27520, #35335, #13079 ) ;
#31615 = CARTESIAN_POINT ( 'NONE',  ( 0.000000000000000000, 73.73191006444551476, 14.66109333815590254 ) ) ;
#31616 = CIRCLE ( 'NONE', #9679, 16.00000000000000000 ) ;
#31617 = EDGE_CURVE ( 'NONE', #31521, #7935, #22193, .T. ) ;
#31618 = CARTESIAN_POINT ( 'NONE',  ( -10.00000000000000000, 0.000000000000000000, 0.000000000000000000 ) ) ;
#31619 = DIRECTION ( 'NONE',  ( -1.000000000000000000, -0.000000000000000000, 0.000000000000000000 ) ) ;
#31620 = DIRECTION ( 'NONE',  ( 0.000000000000000000, 0.000000000000000000, 1.000000000000000000 ) ) ;
#31621 = AXIS2_PLACEMENT_3D ( 'NONE', #6194, #24793, #39968 ) ;
#31622 = AXIS2_PLACEMENT_3D ( 'NONE', #29256, #36592, #17979 ) ;
#31623 = EDGE_CURVE ( 'NONE', #26795, #16364, #3591, .T. ) ;
#31624 = CARTESIAN_POINT ( 'NONE',  ( 10.00000000000000000, -68.27212725128254078, -31.46837873495049465 ) ) ;
#31626 = AXIS2_PLACEMENT_3D ( 'NONE', #40192, #32128, #36502 ) ;
#31625 = CARTESIAN_POINT ( 'NONE',  ( 0.000000000000000000, -22.74946021919153694, 29.81001611431000597 ) ) ;
#31627 = LINE ( 'NONE', #23528, #2945 ) ;
#31628 = DIRECTION ( 'NONE',  ( 0.000000000000000000, -0.8090169943749433434, 0.5877852522924787992 ) ) ;
#31629 = EDGE_CURVE ( 'NONE', #35538, #24295, #15352, .T. ) ;
#31630 = ORIENTED_EDGE ( 'NONE', *, *, #13965, .T. ) ;
#31631 = ORIENTED_EDGE ( 'NONE', *, *, #28874, .F. ) ;
#31633 = CARTESIAN_POINT ( 'NONE',  ( 0.000000000000000000, -76.69515212745996280, -29.01471420065644580 ) ) ;
#31632 = CIRCLE ( 'NONE', #28469, 32.50000000000000000 ) ;
#31634 = CIRCLE ( 'NONE', #10503, 31.99999999999999645 ) ;
#31635 = FACE_OUTER_BOUND ( 'NONE', #42404, .T. ) ;
#31636 = AXIS2_PLACEMENT_3D ( 'NONE', #6336, #44260, #10735 ) ;
#31637 = EDGE_CURVE ( 'NONE', #24133, #35935, #28481, .T. ) ;
#31638 = LINE ( 'NONE', #35042, #33113 ) ;
#31639 = AXIS2_PLACEMENT_3D ( 'NONE', #26923, #8314, #8540 ) ;
#31640 = ORIENTED_EDGE ( 'NONE', *, *, #11006, .F. ) ;
#31641 = ADVANCED_FACE ( 'NONE', ( #18989 ), #37119, .T. ) ;
#31642 = EDGE_CURVE ( 'NONE', #26337, #45282, #33452, .T. ) ;
#31643 = ORIENTED_EDGE ( 'NONE', *, *, #29405, .T. ) ;
#31644 = DIRECTION ( 'NONE',  ( 1.000000000000000000, 0.000000000000000000, 0.000000000000000000 ) ) ;
#31645 = ORIENTED_EDGE ( 'NONE', *, *, #31577, .F. ) ;
#31646 = CARTESIAN_POINT ( 'NONE',  ( 0.000000000000000000, -8.840884882375609877, 74.65374052328647281 ) ) ;
#31647 = ORIENTED_EDGE ( 'NONE', *, *, #27250, .T. ) ;
#31648 = CARTESIAN_POINT ( 'NONE',  ( 0.000000000000000000, 0.000000000000000000, 0.000000000000000000 ) ) ;
#31649 = ADVANCED_FACE ( 'NONE', ( #37367 ), #30504, .F. ) ;
#31650 = VECTOR ( 'NONE', #20562, 999.9999999999998863 ) ;
#31651 = CARTESIAN_POINT ( 'NONE',  ( -42.50000000000000000, 0.000000000000000000, 0.000000000000000000 ) ) ;
#31652 = LINE ( 'NONE', #46079, #4725 ) ;
#31653 = VERTEX_POINT ( 'NONE', #44957 ) ;
#31655 = VERTEX_POINT ( 'NONE', #45426 ) ;
#31654 = LINE ( 'NONE', #35291, #3546 ) ;
#31656 = AXIS2_PLACEMENT_3D ( 'NONE', #38788, #31200, #46121 ) ;
#31657 = ORIENTED_EDGE ( 'NONE', *, *, #29733, .T. ) ;
#31658 = FACE_OUTER_BOUND ( 'NONE', #4113, .T. ) ;
#31659 = CYLINDRICAL_SURFACE ( 'NONE', #24465, 31.99999999999999289 ) ;
#31660 = LINE ( 'NONE', #46325, #4388 ) ;
#31661 = CARTESIAN_POINT ( 'NONE',  ( -3.000000000000000000, 0.000000000000000000, 0.000000000000000000 ) ) ;
#31662 = DIRECTION ( 'NONE',  ( 0.000000000000000000, 0.000000000000000000, 1.000000000000000000 ) ) ;
#31663 = CIRCLE ( 'NONE', #30071, 11.59999999999999787 ) ;
#31664 = AXIS2_PLACEMENT_3D ( 'NONE', #43942, #28777, #39310 ) ;
#31665 = ORIENTED_EDGE ( 'NONE', *, *, #34201, .F. ) ;
#31666 = DIRECTION ( 'NONE',  ( -1.000000000000000000, 0.000000000000000000, 0.000000000000000000 ) ) ;
#31667 = ORIENTED_EDGE ( 'NONE', *, *, #45172, .F. ) ;
#31668 = EDGE_LOOP ( 'NONE', ( #8211, #24085, #36551, #11473 ) ) ;
#31669 = AXIS2_PLACEMENT_3D ( 'NONE', #41778, #30512, #1385 ) ;
#31670 = CARTESIAN_POINT ( 'NONE',  ( 0.000000000000000000, -25.88420570971419821, 27.13269053701087330 ) ) ;
#31671 = CIRCLE ( 'NONE', #46386, 31.99999999999998579 ) ;
#31672 = CARTESIAN_POINT ( 'NONE',  ( 10.00000000000000000, 81.34940948281349904, -10.30890764327296871 ) ) ;
#31673 = VECTOR ( 'NONE', #18635, 1000.000000000000000 ) ;
#31674 = CARTESIAN_POINT ( 'NONE',  ( 22.08297821871651934, -111.8242998470044540, 5.500000000000000000 ) ) ;
#31675 = DIRECTION ( 'NONE',  ( 0.000000000000000000, 0.5224985647159440250, 0.8526401643540951758 ) ) ;
#31676 = EDGE_LOOP ( 'NONE', ( #18186, #42397, #13920, #18452 ) ) ;
#31677 = DIRECTION ( 'NONE',  ( 0.000000000000000000, 0.000000000000000000, 1.000000000000000000 ) ) ;
#31678 = AXIS2_PLACEMENT_3D ( 'NONE', #3043, #43688, #17967 ) ;
#31679 = CARTESIAN_POINT ( 'NONE',  ( 10.00000000000000000, 37.58145647212453611, 16.68533520207917675 ) ) ;
#31680 = DIRECTION ( 'NONE',  ( 1.000000000000000000, -0.000000000000000000, 0.000000000000000000 ) ) ;
#31681 = LINE ( 'NONE', #16730, #9575 ) ;
#31682 = DIRECTION ( 'NONE',  ( 0.000000000000000000, 0.000000000000000000, 1.000000000000000000 ) ) ;
#31683 = ADVANCED_FACE ( 'NONE', ( #22911 ), #4334, .T. ) ;
#31684 = DIRECTION ( 'NONE',  ( -1.000000000000000000, 0.000000000000000000, 0.000000000000000000 ) ) ;
#31685 = CARTESIAN_POINT ( 'NONE',  ( 0.000000000000000000, -19.89357724624987256, -12.59942793731086041 ) ) ;
#31687 = DIRECTION ( 'NONE',  ( -1.000000000000000000, 0.000000000000000000, 0.000000000000000000 ) ) ;
#31686 =( REPRESENTATION_RELATIONSHIP ('NONE','NONE', #5957, #2782 ) REPRESENTATION_RELATIONSHIP_WITH_TRANSFORMATION ( #20113 )SHAPE_REPRESENTATION_RELATIONSHIP( ) );
#31688 = EDGE_CURVE ( 'NONE', #44417, #46514, #21440, .T. ) ;
#31689 = CARTESIAN_POINT ( 'NONE',  ( 0.000000000000000000, 62.50884508063487033, -41.76106447765422303 ) ) ;
#31690 = DIRECTION ( 'NONE',  ( -1.000000000000000000, -0.000000000000000000, 0.000000000000000000 ) ) ;
#31691 = EDGE_CURVE ( 'NONE', #24980, #2713, #1145, .T. ) ;
#31692 = VERTEX_POINT ( 'NONE', #26107 ) ;
#31693 = CIRCLE ( 'NONE', #10560, 31.99999999999999645 ) ;
#31694 = CARTESIAN_POINT ( 'NONE',  ( 12.00000000000000000, 16.83928648764922542, -16.46020748918050458 ) ) ;
#31695 = ORIENTED_EDGE ( 'NONE', *, *, #29900, .F. ) ;
#31696 = DIRECTION ( 'NONE',  ( 0.000000000000000000, 0.000000000000000000, 1.000000000000000000 ) ) ;
#31697 = CIRCLE ( 'NONE', #1157, 35.50000000000000711 ) ;
#31698 = DIRECTION ( 'NONE',  ( 0.000000000000000000, 0.000000000000000000, 1.000000000000000000 ) ) ;
#31699 = EDGE_LOOP ( 'NONE', ( #5409, #11955 ) ) ;
#31700 = EDGE_CURVE ( 'NONE', #6714, #6694, #11667, .T. ) ;
#31701 = EDGE_CURVE ( 'NONE', #29354, #15461, #4275, .T. ) ;
#31702 = CIRCLE ( 'NONE', #41060, 16.00000000000000355 ) ;
#31703 = AXIS2_PLACEMENT_3D ( 'NONE', #36739, #47523, #39953 ) ;
#31704 = CARTESIAN_POINT ( 'NONE',  ( 10.00000000000000000, 10.96151621346487914, 35.95386929396260456 ) ) ;
#31705 = AXIS2_PLACEMENT_3D ( 'NONE', #28865, #36458, #3394 ) ;
#31706 = ORIENTED_EDGE ( 'NONE', *, *, #39463, .F. ) ;
#31707 = ORIENTED_EDGE ( 'NONE', *, *, #27736, .T. ) ;
#31708 = EDGE_LOOP ( 'NONE', ( #11760, #37482, #19035, #41224 ) ) ;
#31709 = CIRCLE ( 'NONE', #37941, 82.00000000000000000 ) ;
#31710 = CIRCLE ( 'NONE', #37163, 37.49900000000000944 ) ;
#31711 = EDGE_CURVE ( 'NONE', #1147, #13754, #27717, .T. ) ;
#31712 = AXIS2_PLACEMENT_3D ( 'NONE', #22071, #18875, #34717 ) ;
#31713 = LINE ( 'NONE', #9396, #40151 ) ;
#31714 = DIRECTION ( 'NONE',  ( 0.000000000000000000, 0.8090169943749487835, -0.5877852522924713607 ) ) ;
#31716 = ORIENTED_EDGE ( 'NONE', *, *, #33962, .F. ) ;
#31715 = PLANE ( 'NONE',  #8234 ) ;
#31717 = ORIENTED_EDGE ( 'NONE', *, *, #15355, .T. ) ;
#31718 = CARTESIAN_POINT ( 'NONE',  ( 10.00000000000000000, 12.26510123303259725, 35.53030884539089840 ) ) ;
#31719 = AXIS2_PLACEMENT_3D ( 'NONE', #13954, #10277, #36470 ) ;
#31720 = ORIENTED_EDGE ( 'NONE', *, *, #47895, .F. ) ;
#31721 = DIRECTION ( 'NONE',  ( 0.000000000000000000, 0.000000000000000000, 1.000000000000000000 ) ) ;
#31722 = DIRECTION ( 'NONE',  ( 0.000000000000000000, 0.000000000000000000, 1.000000000000000000 ) ) ;
#31723 = DIRECTION ( 'NONE',  ( -1.000000000000000000, -0.000000000000000000, 0.000000000000000000 ) ) ;
#31724 = CIRCLE ( 'NONE', #40306, 14.09999999999999964 ) ;
#31725 = ORIENTED_EDGE ( 'NONE', *, *, #40243, .T. ) ;
#31726 = ORIENTED_EDGE ( 'NONE', *, *, #4368, .F. ) ;
#31727 = EDGE_LOOP ( 'NONE', ( #38568, #22948, #31716, #3291 ) ) ;
#31728 = FACE_OUTER_BOUND ( 'NONE', #47965, .T. ) ;
#31729 = VERTEX_POINT ( 'NONE', #11442 ) ;
#31730 = FACE_BOUND ( 'NONE', #22118, .T. ) ;
#31731 = DIRECTION ( 'NONE',  ( 0.3311129884571280546, 0.9435911131814402886, 0.000000000000000000 ) ) ;
#31732 = CARTESIAN_POINT ( 'NONE',  ( 11.99999999999999822, -34.44570377933549565, -69.42325613327476219 ) ) ;
#31733 = CARTESIAN_POINT ( 'NONE',  ( 0.000000000000000000, 0.000000000000000000, 40.00000000000000000 ) ) ;
#31734 = DIRECTION ( 'NONE',  ( -0.000000000000000000, 0.8660254037844368202, 0.5000000000000031086 ) ) ;
#31735 = DIRECTION ( 'NONE',  ( 0.8541291221503261033, -0.5200609990133016058, 0.000000000000000000 ) ) ;
#31736 = DIRECTION ( 'NONE',  ( -1.000000000000000000, 0.000000000000000000, 0.000000000000000000 ) ) ;
#31737 = VERTEX_POINT ( 'NONE', #41292 ) ;
#31738 = DIRECTION ( 'NONE',  ( 1.000000000000000000, 0.000000000000000000, 0.000000000000000000 ) ) ;
#31739 = DIRECTION ( 'NONE',  ( 0.8541291221503275466, -0.5200609990132993854, 0.000000000000000000 ) ) ;
#31740 = CARTESIAN_POINT ( 'NONE',  ( 10.00000000000000000, -35.92658777277502935, -10.74501242461320594 ) ) ;
#31741 = LINE ( 'NONE', #28051, #35634 ) ;
#31742 = AXIS2_PLACEMENT_3D ( 'NONE', #11225, #189, #15145 ) ;
#31743 = ORIENTED_EDGE ( 'NONE', *, *, #12557, .T. ) ;
#31744 = CARTESIAN_POINT ( 'NONE',  ( -3.000000000000000000, -23.29833615347109443, 3.418703333116492438 ) ) ;
#31745 = EDGE_CURVE ( 'NONE', #26295, #43969, #22447, .T. ) ;
#31746 = AXIS2_PLACEMENT_3D ( 'NONE', #24615, #6257, #13847 ) ;
#31747 = DIRECTION ( 'NONE',  ( 0.000000000000000000, 0.000000000000000000, 1.000000000000000000 ) ) ;
#31748 = LINE ( 'NONE', #46662, #8082 ) ;
#31749 = EDGE_CURVE ( 'NONE', #28312, #24194, #15098, .T. ) ;
#31750 = EDGE_CURVE ( 'NONE', #8929, #29160, #5026, .T. ) ;
#31751 = FACE_OUTER_BOUND ( 'NONE', #46508, .T. ) ;
#31752 = CYLINDRICAL_SURFACE ( 'NONE', #32643, 77.49899999999999523 ) ;
#31753 = DIRECTION ( 'NONE',  ( 1.000000000000000000, 0.000000000000000000, 0.000000000000000000 ) ) ;
#31754 = CARTESIAN_POINT ( 'NONE',  ( 10.00000000000000000, 31.47745569255140552, 68.26794271651274926 ) ) ;
#31756 = ADVANCED_FACE ( 'NONE', ( #31486 ), #39058, .F. ) ;
#31755 = ORIENTED_EDGE ( 'NONE', *, *, #5043, .T. ) ;
#31757 = DIRECTION ( 'NONE',  ( -1.000000000000000000, 0.000000000000000000, 0.000000000000000000 ) ) ;
#31758 = VERTEX_POINT ( 'NONE', #34393 ) ;
#31759 =( NAMED_UNIT ( * ) PLANE_ANGLE_UNIT ( ) SI_UNIT ( $, .RADIAN. ) );
#31760 = VECTOR ( 'NONE', #26059, 1000.000000000000000 ) ;
#31761 = DIRECTION ( 'NONE',  ( 0.000000000000000000, -0.9510565162951500895, -0.3090169943749581649 ) ) ;
#31762 = ORIENTED_EDGE ( 'NONE', *, *, #6794, .T. ) ;
#31763 = ORIENTED_EDGE ( 'NONE', *, *, #23607, .T. ) ;
#31764 = EDGE_CURVE ( 'NONE', #26074, #127, #23888, .T. ) ;
#31765 = CIRCLE ( 'NONE', #4394, 16.00000000000000000 ) ;
#31766 = EDGE_CURVE ( 'NONE', #25818, #26295, #16789, .T. ) ;
#31767 = ORIENTED_EDGE ( 'NONE', *, *, #47183, .T. ) ;
#31768 = CARTESIAN_POINT ( 'NONE',  ( 10.00000000000000000, 10.30890764327502573, -81.34940948281324324 ) ) ;
#31769 = CIRCLE ( 'NONE', #10649, 31.99999999999998934 ) ;
#31770 = EDGE_LOOP ( 'NONE', ( #26810, #21902, #39778, #44558 ) ) ;
#31771 = ORIENTED_EDGE ( 'NONE', *, *, #26417, .T. ) ;
#31772 = ADVANCED_FACE ( 'NONE', ( #20207 ), #870, .T. ) ;
#31773 = CIRCLE ( 'NONE', #34116, 31.99999999999998934 ) ;
#31774 = DIRECTION ( 'NONE',  ( -1.000000000000000000, 0.000000000000000000, 0.000000000000000000 ) ) ;
#31775 = CARTESIAN_POINT ( 'NONE',  ( 0.000000000000000000, 27.13269053701096922, 25.88420570971410228 ) ) ;
#31776 = ORIENTED_EDGE ( 'NONE', *, *, #37000, .T. ) ;
#31777 = AXIS2_PLACEMENT_3D ( 'NONE', #2273, #2054, #21104 ) ;
#31778 = ORIENTED_EDGE ( 'NONE', *, *, #826, .F. ) ;
#31779 = CARTESIAN_POINT ( 'NONE',  ( 10.00000000000000000, 0.000000000000000000, 0.000000000000000000 ) ) ;
#31781 = ORIENTED_EDGE ( 'NONE', *, *, #40707, .T. ) ;
#31780 = CARTESIAN_POINT ( 'NONE',  ( 0.5480546763151027401, -96.50639159107802811, 2.500000000000000000 ) ) ;
#31782 = EDGE_CURVE ( 'NONE', #39583, #40958, #4799, .T. ) ;
#31783 = PLANE ( 'NONE',  #878 ) ;
#31784 = ORIENTED_EDGE ( 'NONE', *, *, #13372, .F. ) ;
#31785 = EDGE_LOOP ( 'NONE', ( #20189, #14860, #2599, #20231 ) ) ;
#31786 = DIRECTION ( 'NONE',  ( -1.000000000000000000, -0.000000000000000000, -0.000000000000000000 ) ) ;
#31787 = ORIENTED_EDGE ( 'NONE', *, *, #14648, .F. ) ;
#31788 = CARTESIAN_POINT ( 'NONE',  ( 10.00000000000000000, -16.23288003029473359, -33.80338159004301701 ) ) ;
#31789 = DIRECTION ( 'NONE',  ( 0.000000000000000000, -0.4539904997395541875, 0.8910065241883641241 ) ) ;
#31790 = VECTOR ( 'NONE', #35267, 1000.000000000000114 ) ;
#31791 = DIRECTION ( 'NONE',  ( -1.000000000000000000, -0.000000000000000000, 0.000000000000000000 ) ) ;
#31792 = CARTESIAN_POINT ( 'NONE',  ( 11.99999999999999822, -30.41916302227062019, -71.27951684758059514 ) ) ;
#31793 = CARTESIAN_POINT ( 'NONE',  ( 11.99999999999999822, -62.20884554314051229, 46.21855187248609553 ) ) ;
#31794 = AXIS2_PLACEMENT_3D ( 'NONE', #6891, #36018, #36262 ) ;
#31795 = VERTEX_POINT ( 'NONE', #46404 ) ;
#31796 = ORIENTED_EDGE ( 'NONE', *, *, #2324, .T. ) ;
#31797 = CYLINDRICAL_SURFACE ( 'NONE', #6325, 82.00000000000000000 ) ;
#31798 = VECTOR ( 'NONE', #33749, 1000.000000000000000 ) ;
#31799 = CARTESIAN_POINT ( 'NONE',  ( 11.99999999999999822, 59.03961581697465277, -46.53671651293886669 ) ) ;
#31800 = EDGE_LOOP ( 'NONE', ( #7600, #8876, #46041, #42803 ) ) ;
#31801 = EDGE_CURVE ( 'NONE', #30039, #8075, #18325, .T. ) ;
#31802 = DIRECTION ( 'NONE',  ( 0.000000000000000000, -0.8090169943749402348, -0.5877852522924830181 ) ) ;
#31803 = EDGE_LOOP ( 'NONE', ( #18862, #25579, #46573, #19455 ) ) ;
#31804 = LINE ( 'NONE', #4864, #5079 ) ;
#31805 = EDGE_CURVE ( 'NONE', #5554, #8790, #3490, .T. ) ;
#31806 = DIRECTION ( 'NONE',  ( 0.000000000000000000, 0.9969173337331276308, 0.07845909572784873220 ) ) ;
#31807 = DIRECTION ( 'NONE',  ( -0.000000000000000000, -0.000000000000000000, -1.000000000000000000 ) ) ;
#31808 = ORIENTED_EDGE ( 'NONE', *, *, #7633, .F. ) ;
#31809 = DIRECTION ( 'NONE',  ( -1.000000000000000000, 0.000000000000000000, 0.000000000000000000 ) ) ;
#31810 = EDGE_CURVE ( 'NONE', #42670, #46575, #12630, .T. ) ;
#31811 =( LENGTH_UNIT ( ) NAMED_UNIT ( * ) SI_UNIT ( .MILLI., .METRE. ) );
#31812 = DIRECTION ( 'NONE',  ( -1.000000000000000000, 0.000000000000000000, 0.000000000000000000 ) ) ;
#31813 = AXIS2_PLACEMENT_3D ( 'NONE', #4068, #34160, #15340 ) ;
#31814 = EDGE_LOOP ( 'NONE', ( #11670, #43171, #21397, #12356 ) ) ;
#31815 = CARTESIAN_POINT ( 'NONE',  ( 12.49999999999999645, 1.530808498934191127E-15, 52.00000000000002132 ) ) ;
#31816 = CARTESIAN_POINT ( 'NONE',  ( 10.00000000000000000, 22.74946021919133088, 29.81001611431016229 ) ) ;
#31817 = CARTESIAN_POINT ( 'NONE',  ( 11.99999999999999822, 35.91791733033570466, -68.67312586194960033 ) ) ;
#31818 = ADVANCED_FACE ( 'NONE', ( #45927 ), #16540, .T. ) ;
#31819 = AXIS2_PLACEMENT_3D ( 'NONE', #35750, #2217, #22007 ) ;
#31820 = DIRECTION ( 'NONE',  ( -1.000000000000000000, 0.000000000000000000, 0.000000000000000000 ) ) ;
#31821 = ORIENTED_EDGE ( 'NONE', *, *, #2976, .F. ) ;
#31822 = ORIENTED_EDGE ( 'NONE', *, *, #12761, .T. ) ;
#31823 = VERTEX_POINT ( 'NONE', #12395 ) ;
#31824 = AXIS2_PLACEMENT_3D ( 'NONE', #1194, #46227, #31074 ) ;
#31825 = CARTESIAN_POINT ( 'NONE',  ( 0.000000000000000000, -46.21855187248583974, -62.20884554314070414 ) ) ;
#31826 = VECTOR ( 'NONE', #39567, 1000.000000000000000 ) ;
#31827 = CARTESIAN_POINT ( 'NONE',  ( -3.308722450212110699E-21, 16.95692799528845640, -2.500000000000000000 ) ) ;
#31828 = ORIENTED_EDGE ( 'NONE', *, *, #20504, .T. ) ;
#31829 = VECTOR ( 'NONE', #7030, 1000.000000000000000 ) ;
#31830 = ORIENTED_EDGE ( 'NONE', *, *, #1764, .T. ) ;
#31831 = DIRECTION ( 'NONE',  ( 0.000000000000000000, 0.000000000000000000, -1.000000000000000000 ) ) ;
#31832 = DIRECTION ( 'NONE',  ( 1.000000000000000000, 0.000000000000000000, 0.000000000000000000 ) ) ;
#31833 = VERTEX_POINT ( 'NONE', #42976 ) ;
#31834 = VERTEX_POINT ( 'NONE', #27817 ) ;
#31835 = ORIENTED_EDGE ( 'NONE', *, *, #42243, .F. ) ;
#31836 = AXIS2_PLACEMENT_3D ( 'NONE', #42230, #8685, #19233 ) ;
#31837 = CARTESIAN_POINT ( 'NONE',  ( 10.00000000000000000, -17.67226234102801286, -33.17418723428327354 ) ) ;
#31838 = VERTEX_POINT ( 'NONE', #1861 ) ;
#31839 = CARTESIAN_POINT ( 'NONE',  ( -20.30386590532152979, -102.9045904027214959, 2.500000000000000000 ) ) ;
#31840 = ORIENTED_EDGE ( 'NONE', *, *, #4982, .T. ) ;
#31841 = CARTESIAN_POINT ( 'NONE',  ( 0.000000000000000000, 0.000000000000000000, 0.000000000000000000 ) ) ;
#31842 = CIRCLE ( 'NONE', #2885, 37.49900000000000944 ) ;
#31843 = DIRECTION ( 'NONE',  ( -0.000000000000000000, 0.5000000000000039968, -0.8660254037844363761 ) ) ;
#31844 = CARTESIAN_POINT ( 'NONE',  ( 10.00000000000000000, 0.000000000000000000, 0.000000000000000000 ) ) ;
#31845 = ORIENTED_EDGE ( 'NONE', *, *, #20889, .T. ) ;
#31846 = CARTESIAN_POINT ( 'NONE',  ( 10.00000000000000000, 0.000000000000000000, 0.000000000000000000 ) ) ;
#31847 = ORIENTED_EDGE ( 'NONE', *, *, #40242, .F. ) ;
#31848 = DIRECTION ( 'NONE',  ( -1.000000000000000000, 0.000000000000000000, -0.000000000000000000 ) ) ;
#31849 = CARTESIAN_POINT ( 'NONE',  ( -3.000000000000000000, -26.23277895567245821, -4.042438405570103477 ) ) ;
#31850 = VECTOR ( 'NONE', #35814, 1000.000000000000000 ) ;
#31851 = LINE ( 'NONE', #32722, #15494 ) ;
#31852 = ORIENTED_EDGE ( 'NONE', *, *, #4980, .T. ) ;
#31853 = ORIENTED_EDGE ( 'NONE', *, *, #12310, .T. ) ;
#31854 = ADVANCED_FACE ( 'NONE', ( #27324 ), #19963, .T. ) ;
#31855 = CARTESIAN_POINT ( 'NONE',  ( 5.000000000000000000, 15.48615015657581750, 39.04073710021349797 ) ) ;
#31856 = CYLINDRICAL_SURFACE ( 'NONE', #38725, 82.00000000000000000 ) ;
#31857 = ORIENTED_EDGE ( 'NONE', *, *, #12315, .T. ) ;
#31858 = DIRECTION ( 'NONE',  ( -1.000000000000000000, -0.000000000000000000, -0.000000000000000000 ) ) ;
#31859 = DIRECTION ( 'NONE',  ( -1.000000000000000000, 0.000000000000000000, 0.000000000000000000 ) ) ;
#31860 = CARTESIAN_POINT ( 'NONE',  ( -5.420674214417706693, -142.8662697233533265, 2.500000000000000000 ) ) ;
#31861 = EDGE_CURVE ( 'NONE', #9412, #38298, #18363, .T. ) ;
#31862 = DIRECTION ( 'NONE',  ( 0.000000000000000000, 0.000000000000000000, 1.000000000000000000 ) ) ;
#31863 = AXIS2_PLACEMENT_3D ( 'NONE', #32911, #47837, #6743 ) ;
#31864 = DIRECTION ( 'NONE',  ( -1.000000000000000000, 0.000000000000000000, 0.000000000000000000 ) ) ;
#31865 = CYLINDRICAL_SURFACE ( 'NONE', #1234, 31.99999999999998579 ) ;
#31866 = DIRECTION ( 'NONE',  ( -1.000000000000000000, 0.000000000000000000, 0.000000000000000000 ) ) ;
#31867 = EDGE_CURVE ( 'NONE', #21020, #23818, #23059, .T. ) ;
#31868 = ORIENTED_EDGE ( 'NONE', *, *, #42329, .T. ) ;
#31869 = EDGE_CURVE ( 'NONE', #12683, #27602, #1122, .T. ) ;
#31870 = DIRECTION ( 'NONE',  ( 0.000000000000000000, -0.3826834323650969427, 0.9238795325112837409 ) ) ;
#31871 = CARTESIAN_POINT ( 'NONE',  ( 10.00000000000000000, -12.93880638057259169, -76.41127070299286572 ) ) ;
#31872 = LINE ( 'NONE', #43353, #31940 ) ;
#31873 = DIRECTION ( 'NONE',  ( -1.000000000000000000, -0.000000000000000000, 0.000000000000000000 ) ) ;
#31874 = DIRECTION ( 'NONE',  ( -1.000000000000000000, 0.000000000000000000, 0.000000000000000000 ) ) ;
#31875 = ORIENTED_EDGE ( 'NONE', *, *, #8554, .F. ) ;
#31876 = ORIENTED_EDGE ( 'NONE', *, *, #20434, .T. ) ;
#31877 = AXIS2_PLACEMENT_3D ( 'NONE', #24118, #39046, #35847 ) ;
#31878 = DIRECTION ( 'NONE',  ( -1.000000000000000000, -0.000000000000000000, -0.000000000000000000 ) ) ;
#31879 = CARTESIAN_POINT ( 'NONE',  ( 0.000000000000000000, -27.74655509720725988, 77.16300072079653205 ) ) ;
#31880 = ADVANCED_FACE ( 'NONE', ( #38582 ), #31244, .T. ) ;
#31881 = CIRCLE ( 'NONE', #10750, 16.00000000000000355 ) ;
#31882 = CARTESIAN_POINT ( 'NONE',  ( 12.00000000000000000, -11.95096189432312350, 23.69967320028773017 ) ) ;
#31883 = ORIENTED_EDGE ( 'NONE', *, *, #14237, .T. ) ;
#31884 = EDGE_CURVE ( 'NONE', #38396, #33784, #16036, .T. ) ;
#31885 = ORIENTED_EDGE ( 'NONE', *, *, #42715, .T. ) ;
#31886 = AXIS2_PLACEMENT_3D ( 'NONE', #32154, #25026, #36047 ) ;
#31887 = FACE_OUTER_BOUND ( 'NONE', #42639, .T. ) ;
#31888 = ORIENTED_EDGE ( 'NONE', *, *, #36579, .F. ) ;
#31889 = DIRECTION ( 'NONE',  ( -1.000000000000000000, 0.000000000000000000, -0.000000000000000000 ) ) ;
#31890 = VERTEX_POINT ( 'NONE', #40273 ) ;
#31891 = SURFACE_STYLE_FILL_AREA ( #12786 ) ;
#31892 = AXIS2_PLACEMENT_3D ( 'NONE', #39443, #14205, #22277 ) ;
#31893 = EDGE_CURVE ( 'NONE', #24345, #27291, #17564, .T. ) ;
#31894 = DIRECTION ( 'NONE',  ( 0.000000000000000000, 0.000000000000000000, 1.000000000000000000 ) ) ;
#31895 = CARTESIAN_POINT ( 'NONE',  ( 15.00000000000000000, -14.54903810567644484, 22.19967320028775504 ) ) ;
#31896 = ORIENTED_EDGE ( 'NONE', *, *, #4269, .T. ) ;
#31898 = ORIENTED_EDGE ( 'NONE', *, *, #45402, .F. ) ;
#31897 = DIRECTION ( 'NONE',  ( -0.000000000000000000, -0.3090169943749572767, -0.9510565162951503115 ) ) ;
#31899 = ADVANCED_FACE ( 'NONE', ( #13845 ), #36342, .T. ) ;
#31900 = ORIENTED_EDGE ( 'NONE', *, *, #7698, .F. ) ;
#31901 = ORIENTED_EDGE ( 'NONE', *, *, #20784, .T. ) ;
#31902 = FACE_OUTER_BOUND ( 'NONE', #7619, .T. ) ;
#31903 = EDGE_CURVE ( 'NONE', #8099, #17326, #17492, .T. ) ;
#31904 = CARTESIAN_POINT ( 'NONE',  ( 10.00000000000000000, 0.000000000000000000, 0.000000000000000000 ) ) ;
#31905 = CARTESIAN_POINT ( 'NONE',  ( 10.00000000000000000, 17.28742895386191236, -75.54627589209927407 ) ) ;
#31906 = DIRECTION ( 'NONE',  ( 0.000000000000000000, 0.7431448254773946882, -0.6691306063588577935 ) ) ;
#31907 = ORIENTED_EDGE ( 'NONE', *, *, #35204, .F. ) ;
#31908 = CARTESIAN_POINT ( 'NONE',  ( 0.000000000000000000, 0.000000000000000000, 0.000000000000000000 ) ) ;
#31909 = ORIENTED_EDGE ( 'NONE', *, *, #27715, .T. ) ;
#31910 = CARTESIAN_POINT ( 'NONE',  ( 11.99999999999999822, 29.01471420065673712, -76.69515212745983490 ) ) ;
#31911 = ORIENTED_EDGE ( 'NONE', *, *, #19761, .F. ) ;
#31912 = AXIS2_PLACEMENT_3D ( 'NONE', #18422, #30174, #544 ) ;
#31913 = DIRECTION ( 'NONE',  ( -1.000000000000000000, 0.000000000000000000, 0.000000000000000000 ) ) ;
#31914 = CARTESIAN_POINT ( 'NONE',  ( 0.000000000000000000, 51.29473840253317718, -63.97538442413369353 ) ) ;
#31915 = DIRECTION ( 'NONE',  ( -1.000000000000000000, -0.000000000000000000, 0.000000000000000000 ) ) ;
#31916 = ORIENTED_EDGE ( 'NONE', *, *, #8657, .T. ) ;
#31917 = FACE_OUTER_BOUND ( 'NONE', #30714, .T. ) ;
#31918 = EDGE_CURVE ( 'NONE', #40043, #47056, #1966, .T. ) ;
#31919 = AXIS2_PLACEMENT_3D ( 'NONE', #35668, #39095, #2140 ) ;
#31920 = CARTESIAN_POINT ( 'NONE',  ( 5.999999999999999112, -21.60688246758642705, 79.10210256391358996 ) ) ;
#31921 = EDGE_CURVE ( 'NONE', #45054, #24690, #20716, .T. ) ;
#31922 = EDGE_CURVE ( 'NONE', #5004, #33903, #13353, .T. ) ;
#31923 = DIRECTION ( 'NONE',  ( 0.000000000000000000, 0.000000000000000000, 1.000000000000000000 ) ) ;
#31924 = CYLINDRICAL_SURFACE ( 'NONE', #13503, 16.00000000000000000 ) ;
#31925 = FACE_OUTER_BOUND ( 'NONE', #47505, .T. ) ;
#31926 = DIRECTION ( 'NONE',  ( 0.000000000000000000, 0.000000000000000000, -1.000000000000000000 ) ) ;
#31927 = CARTESIAN_POINT ( 'NONE',  ( 0.000000000000000000, -37.22597642581161637, 5.202137450156258502 ) ) ;
#31928 = DIRECTION ( 'NONE',  ( -0.2079116908177527367, 1.197885328332319922E-16, -0.9781476007338070211 ) ) ;
#31929 = EDGE_CURVE ( 'NONE', #371, #13186, #3513, .T. ) ;
#31930 = CARTESIAN_POINT ( 'NONE',  ( 0.000000000000000000, 71.87247863392413194, 39.47590169984871267 ) ) ;
#31931 = CARTESIAN_POINT ( 'NONE',  ( 5.999999999999999112, 71.21200624218795383, 40.65526001592638039 ) ) ;
#31932 = AXIS2_PLACEMENT_3D ( 'NONE', #716, #45499, #15651 ) ;
#31933 = DIRECTION ( 'NONE',  ( -1.000000000000000000, 0.000000000000000000, 0.000000000000000000 ) ) ;
#31934 = ORIENTED_EDGE ( 'NONE', *, *, #8221, .T. ) ;
#31935 = DIRECTION ( 'NONE',  ( 0.9966891607226785466, 0.08130631524009969413, -0.000000000000000000 ) ) ;
#31936 = EDGE_CURVE ( 'NONE', #14753, #5918, #22287, .T. ) ;
#31937 = DIRECTION ( 'NONE',  ( -1.000000000000000000, -0.000000000000000000, -0.000000000000000000 ) ) ;
#31938 = ORIENTED_EDGE ( 'NONE', *, *, #26790, .T. ) ;
#31939 = CARTESIAN_POINT ( 'NONE',  ( 0.000000000000000000, 0.000000000000000000, -44.99999999999998579 ) ) ;
#31940 = VECTOR ( 'NONE', #39915, 1000.000000000000000 ) ;
#31941 = VERTEX_POINT ( 'NONE', #17244 ) ;
#31942 = VECTOR ( 'NONE', #16998, 1000.000000000000000 ) ;
#31943 = VERTEX_POINT ( 'NONE', #32665 ) ;
#31944 = ADVANCED_FACE ( 'NONE', ( #47116 ), #36580, .T. ) ;
#31945 = EDGE_CURVE ( 'NONE', #34492, #648, #42595, .T. ) ;
#31946 = CARTESIAN_POINT ( 'NONE',  ( 0.000000000000000000, 4.992566952385522505, -37.16516213103271582 ) ) ;
#31947 = CARTESIAN_POINT ( 'NONE',  ( 0.000000000000000000, 33.17418723428307459, 17.67226234102837878 ) ) ;
#31948 = CARTESIAN_POINT ( 'NONE',  ( 6.000000000000000000, 29.01471420065673712, -76.69515212745984911 ) ) ;
#31949 = ADVANCED_FACE ( 'NONE', ( #6255 ), #20691, .T. ) ;
#31950 = ORIENTED_EDGE ( 'NONE', *, *, #39527, .T. ) ;
#31951 = CARTESIAN_POINT ( 'NONE',  ( -2.977765906491215642, 1.932465207890948911E-15, 15.77977592589476608 ) ) ;
#31952 =( GEOMETRIC_REPRESENTATION_CONTEXT ( 3 ) GLOBAL_UNCERTAINTY_ASSIGNED_CONTEXT ( ( #7592 ) ) GLOBAL_UNIT_ASSIGNED_CONTEXT ( ( #10355, #8720, #27839 ) ) REPRESENTATION_CONTEXT ( 'NONE', 'WORKASPACE' ) );
#31953 = EDGE_LOOP ( 'NONE', ( #1313, #17867, #37946, #31575 ) ) ;
#31954 = EDGE_CURVE ( 'NONE', #21662, #36119, #5773, .T. ) ;
#31955 = ORIENTED_EDGE ( 'NONE', *, *, #15963, .F. ) ;
#31956 = DIRECTION ( 'NONE',  ( 0.000000000000000000, 0.000000000000000000, 1.000000000000000000 ) ) ;
#31957 = DIRECTION ( 'NONE',  ( 0.000000000000000000, 0.000000000000000000, 1.000000000000000000 ) ) ;
#31958 = CARTESIAN_POINT ( 'NONE',  ( 0.000000000000000000, 0.000000000000000000, 0.000000000000000000 ) ) ;
#31959 = VERTEX_POINT ( 'NONE', #20939 ) ;
#31960 = ORIENTED_EDGE ( 'NONE', *, *, #28296, .T. ) ;
#31961 = LINE ( 'NONE', #43454, #4493 ) ;
#31962 = VERTEX_POINT ( 'NONE', #2101 ) ;
#31963 = FACE_BOUND ( 'NONE', #2075, .T. ) ;
#31964 = DIRECTION ( 'NONE',  ( -1.000000000000000000, -0.000000000000000000, 0.000000000000000000 ) ) ;
#31965 = LINE ( 'NONE', #42236, #26888 ) ;
#31966 = LINE ( 'NONE', #13349, #38349 ) ;
#31967 = CARTESIAN_POINT ( 'NONE',  ( 6.000000000000000000, 68.55367621811204515, -44.99326035065983120 ) ) ;
#31968 = LINE ( 'NONE', #36340, #47981 ) ;
#31969 = EDGE_CURVE ( 'NONE', #10316, #40419, #30901, .T. ) ;
#31970 = EDGE_CURVE ( 'NONE', #8466, #36706, #8977, .T. ) ;
#31971 = DIRECTION ( 'NONE',  ( -1.000000000000000000, -0.000000000000000000, 0.000000000000000000 ) ) ;
#31972 = DIRECTION ( 'NONE',  ( 0.000000000000000000, 0.000000000000000000, 1.000000000000000000 ) ) ;
#31973 = DIRECTION ( 'NONE',  ( -0.1276937514489679404, -0.9918136447140103451, 0.000000000000000000 ) ) ;
#31974 = CARTESIAN_POINT ( 'NONE',  ( 15.00000000000000000, 16.83928648764945635, 16.46020748918027010 ) ) ;
#31975 = EDGE_LOOP ( 'NONE', ( #20836, #43782, #27178, #7816 ) ) ;
#31976 = ORIENTED_EDGE ( 'NONE', *, *, #40173, .F. ) ;
#31977 = DIRECTION ( 'NONE',  ( 0.000000000000000000, 0.000000000000000000, 1.000000000000000000 ) ) ;
#31978 = AXIS2_PLACEMENT_3D ( 'NONE', #35462, #1953, #16874 ) ;
#31979 = CIRCLE ( 'NONE', #38219, 77.49899999999999523 ) ;
#31980 = CARTESIAN_POINT ( 'NONE',  ( 0.000000000000000000, 38.55633173627034438, -16.65560815589369881 ) ) ;
#31981 = FACE_OUTER_BOUND ( 'NONE', #32710, .T. ) ;
#31982 = AXIS2_PLACEMENT_3D ( 'NONE', #10377, #25542, #40492 ) ;
#31983 = CARTESIAN_POINT ( 'NONE',  ( -11.70000000000000107, 0.000000000000000000, 0.000000000000000000 ) ) ;
#31984 = CARTESIAN_POINT ( 'NONE',  ( 12.00000000000000000, 6.762365576493310826, -25.66652317338400735 ) ) ;
#31985 = EDGE_CURVE ( 'NONE', #28510, #42762, #43208, .T. ) ;
#31986 = ORIENTED_EDGE ( 'NONE', *, *, #13723, .T. ) ;
#31987 = DIRECTION ( 'NONE',  ( 0.000000000000000000, 0.000000000000000000, 1.000000000000000000 ) ) ;
#31988 = DIRECTION ( 'NONE',  ( 0.000000000000000000, -0.4999999999999920064, 0.8660254037844432595 ) ) ;
#31989 = ORIENTED_EDGE ( 'NONE', *, *, #41369, .T. ) ;
#31990 = DIRECTION ( 'NONE',  ( 0.000000000000000000, 0.000000000000000000, 1.000000000000000000 ) ) ;
#31991 = ORIENTED_EDGE ( 'NONE', *, *, #28713, .F. ) ;
#31992 = FACE_OUTER_BOUND ( 'NONE', #33853, .T. ) ;
#31993 = VERTEX_POINT ( 'NONE', #2326 ) ;
#31994 = ORIENTED_EDGE ( 'NONE', *, *, #25576, .F. ) ;
#31995 = AXIS2_PLACEMENT_3D ( 'NONE', #12766, #27704, #24031 ) ;
#31996 = DIRECTION ( 'NONE',  ( 0.000000000000000000, 0.7071067811865486830, -0.7071067811865463515 ) ) ;
#31997 = ORIENTED_EDGE ( 'NONE', *, *, #14247, .T. ) ;
#31998 = VERTEX_POINT ( 'NONE', #32201 ) ;
#31999 = AXIS2_PLACEMENT_3D ( 'NONE', #45715, #41090, #11942 ) ;
#32000 = CARTESIAN_POINT ( 'NONE',  ( 10.00000000000000000, 0.000000000000000000, 0.000000000000000000 ) ) ;
#32001 = CARTESIAN_POINT ( 'NONE',  ( 11.99999999999999822, 0.000000000000000000, 0.000000000000000000 ) ) ;
#32003 = EDGE_CURVE ( 'NONE', #27374, #18460, #13589, .T. ) ;
#32002 = AXIS2_PLACEMENT_3D ( 'NONE', #35657, #16564, #42768 ) ;
#32004 = ORIENTED_EDGE ( 'NONE', *, *, #18278, .F. ) ;
#32005 = VERTEX_POINT ( 'NONE', #24845 ) ;
#32006 = ORIENTED_EDGE ( 'NONE', *, *, #47799, .T. ) ;
#32007 = AXIS2_PLACEMENT_3D ( 'NONE', #16826, #1905, #46694 ) ;
#32008 = EDGE_CURVE ( 'NONE', #42227, #26870, #39493, .T. ) ;
#32009 = CARTESIAN_POINT ( 'NONE',  ( 10.00000000000000000, -2.946379043146863719, 75.11764819372146462 ) ) ;
#32011 = ORIENTED_EDGE ( 'NONE', *, *, #26489, .T. ) ;
#32010 = CARTESIAN_POINT ( 'NONE',  ( 0.000000000000000000, -75.11725578898470701, 2.956366410620372864 ) ) ;
#32012 = DIRECTION ( 'NONE',  ( 0.000000000000000000, 0.000000000000000000, 1.000000000000000000 ) ) ;
#32013 = ORIENTED_EDGE ( 'NONE', *, *, #35655, .T. ) ;
#32014 = ORIENTED_EDGE ( 'NONE', *, *, #14151, .T. ) ;
#32015 = CARTESIAN_POINT ( 'NONE',  ( 4.903647372192503795, -146.0423547792665886, -2.500000000000000000 ) ) ;
#32016 = ORIENTED_EDGE ( 'NONE', *, *, #45602, .T. ) ;
#32017 = LINE ( 'NONE', #12439, #30640 ) ;
#32018 = DIRECTION ( 'NONE',  ( -1.000000000000000000, -0.000000000000000000, -0.000000000000000000 ) ) ;
#32019 = CARTESIAN_POINT ( 'NONE',  ( 10.00000000000000000, -59.75363087400112505, 56.15606465354937882 ) ) ;
#32020 = DIRECTION ( 'NONE',  ( -1.000000000000000000, 0.000000000000000000, 0.000000000000000000 ) ) ;
#32021 = DIRECTION ( 'NONE',  ( 0.000000000000000000, 0.000000000000000000, 1.000000000000000000 ) ) ;
#32022 = ORIENTED_EDGE ( 'NONE', *, *, #3235, .F. ) ;
#32023 = EDGE_CURVE ( 'NONE', #45952, #44798, #25607, .T. ) ;
#32024 =( GEOMETRIC_REPRESENTATION_CONTEXT ( 3 ) GLOBAL_UNCERTAINTY_ASSIGNED_CONTEXT ( ( #29614 ) ) GLOBAL_UNIT_ASSIGNED_CONTEXT ( ( #14152, #18295, #40815 ) ) REPRESENTATION_CONTEXT ( 'NONE', 'WORKASPACE' ) );
#32025 = CYLINDRICAL_SURFACE ( 'NONE', #5550, 82.00000000000000000 ) ;
#32026 = DIRECTION ( 'NONE',  ( -0.5687579148473743684, 0.8225049752423791993, 0.000000000000000000 ) ) ;
#32027 = ORIENTED_EDGE ( 'NONE', *, *, #46299, .T. ) ;
#32028 = EDGE_CURVE ( 'NONE', #13467, #23694, #26347, .T. ) ;
#32029 = DIRECTION ( 'NONE',  ( -1.000000000000000000, -0.000000000000000000, 0.000000000000000000 ) ) ;
#32030 = ORIENTED_EDGE ( 'NONE', *, *, #20268, .F. ) ;
#32031 = CARTESIAN_POINT ( 'NONE',  ( 0.000000000000000000, -120.0000000000000000, -40.00000000000000711 ) ) ;
#32032 = CARTESIAN_POINT ( 'NONE',  ( 0.000000000000000000, 0.000000000000000000, 0.000000000000000000 ) ) ;
#32033 = FACE_OUTER_BOUND ( 'NONE', #41959, .T. ) ;
#32034 = LINE ( 'NONE', #32263, #5722 ) ;
#32035 = CARTESIAN_POINT ( 'NONE',  ( 10.00000000000000000, -3.925862922255855647, -41.81611651403866858 ) ) ;
#32036 = CARTESIAN_POINT ( 'NONE',  ( -10.00000000000000000, 0.000000000000000000, 0.000000000000000000 ) ) ;
#32037 = ADVANCED_FACE ( 'NONE', ( #26098 ), #41517, .F. ) ;
#32038 = AXIS2_PLACEMENT_3D ( 'NONE', #1737, #20565, #8825 ) ;
#32039 = ORIENTED_EDGE ( 'NONE', *, *, #16928, .T. ) ;
#32040 = PLANE ( 'NONE',  #24711 ) ;
#32041 = CYLINDRICAL_SURFACE ( 'NONE', #21433, 16.00000000000000000 ) ;
#32042 = AXIS2_PLACEMENT_3D ( 'NONE', #6286, #2589, #2840 ) ;
#32043 = CARTESIAN_POINT ( 'NONE',  ( 0.000000000000000000, 74.18225833017888249, 34.94270380257665209 ) ) ;
#32044 = CIRCLE ( 'NONE', #8562, 77.49899999999999523 ) ;
#32045 = LINE ( 'NONE', #17319, #34654 ) ;
#32046 = ORIENTED_EDGE ( 'NONE', *, *, #17001, .T. ) ;
#32047 = VERTEX_POINT ( 'NONE', #41048 ) ;
#32048 = AXIS2_PLACEMENT_3D ( 'NONE', #24661, #32248, #40978 ) ;
#32049 = VERTEX_POINT ( 'NONE', #40548 ) ;
#32050 = CARTESIAN_POINT ( 'NONE',  ( 0.000000000000000000, 0.000000000000000000, 0.000000000000000000 ) ) ;
#32051 = PLANE ( 'NONE',  #35528 ) ;
#32052 = EDGE_LOOP ( 'NONE', ( #6829, #5806, #5731, #19556 ) ) ;
#32053 = EDGE_CURVE ( 'NONE', #47967, #4600, #34789, .T. ) ;
#32054 = DIRECTION ( 'NONE',  ( 1.000000000000000000, -0.000000000000000000, -0.000000000000000000 ) ) ;
#32055 = ORIENTED_EDGE ( 'NONE', *, *, #28590, .F. ) ;
#32056 = EDGE_CURVE ( 'NONE', #40015, #36455, #23830, .T. ) ;
#32057 = EDGE_LOOP ( 'NONE', ( #32892, #14645, #14523, #23987 ) ) ;
#32058 = ORIENTED_EDGE ( 'NONE', *, *, #1959, .F. ) ;
#32059 = ORIENTED_EDGE ( 'NONE', *, *, #35798, .F. ) ;
#32060 = EDGE_CURVE ( 'NONE', #41101, #4382, #30017, .T. ) ;
#32061 = CIRCLE ( 'NONE', #4697, 31.99999999999998579 ) ;
#32062 = DIRECTION ( 'NONE',  ( 1.000000000000000000, 0.000000000000000000, 0.000000000000000000 ) ) ;
#32063 = EDGE_CURVE ( 'NONE', #44520, #45891, #22904, .T. ) ;
#32065 = ORIENTED_EDGE ( 'NONE', *, *, #27385, .T. ) ;
#32064 = CIRCLE ( 'NONE', #16397, 31.99999999999998579 ) ;
#32066 = DIRECTION ( 'NONE',  ( 0.000000000000000000, -0.8910065241883626808, -0.4539904997395570740 ) ) ;
#32067 = EDGE_CURVE ( 'NONE', #28383, #13636, #41026, .T. ) ;
#32068 = EDGE_LOOP ( 'NONE', ( #26762, #6622, #26211, #3844 ) ) ;
#32069 = CARTESIAN_POINT ( 'NONE',  ( 0.1219594728601484379, -121.4950337410840149, -2.500000000000000000 ) ) ;
#32070 = CIRCLE ( 'NONE', #45328, 16.00000000000000000 ) ;
#32071 = CARTESIAN_POINT ( 'NONE',  ( 10.00000000000000000, 5.202137450156389953, 37.22597642581160216 ) ) ;
#32072 = DIRECTION ( 'NONE',  ( -1.000000000000000000, -0.000000000000000000, -0.000000000000000000 ) ) ;
#32073 = DIRECTION ( 'NONE',  ( 0.000000000000000000, 0.07845909572783793529, 0.9969173337331285190 ) ) ;
#32074 = ORIENTED_EDGE ( 'NONE', *, *, #41122, .T. ) ;
#32075 = AXIS2_PLACEMENT_3D ( 'NONE', #25308, #40268, #37305 ) ;
#32076 = CARTESIAN_POINT ( 'NONE',  ( 10.00000000000000000, -22.74946021919110706, -29.81001611431033282 ) ) ;
#32077 = LINE ( 'NONE', #28639, #17265 ) ;
#32078 = ORIENTED_EDGE ( 'NONE', *, *, #12186, .T. ) ;
#32079 = VECTOR ( 'NONE', #44093, 1000.000000000000000 ) ;
#32080 = EDGE_LOOP ( 'NONE', ( #30012, #35242, #43838, #10920 ) ) ;
#32081 = DIRECTION ( 'NONE',  ( -1.000000000000000000, 0.000000000000000000, 0.000000000000000000 ) ) ;
#32082 = DIRECTION ( 'NONE',  ( 0.000000000000000000, -0.7071067811865535679, 0.7071067811865413555 ) ) ;
#32083 = VERTEX_POINT ( 'NONE', #15089 ) ;
#32084 = CARTESIAN_POINT ( 'NONE',  ( -10.00000000000000000, 0.000000000000000000, 0.000000000000000000 ) ) ;
#32085 = FACE_OUTER_BOUND ( 'NONE', #34068, .T. ) ;
#32086 = CARTESIAN_POINT ( 'NONE',  ( -35.50000000000000711, -120.0000000000000000, 2.500000000000000000 ) ) ;
#32087 = PLANE ( 'NONE',  #43720 ) ;
#32088 = CARTESIAN_POINT ( 'NONE',  ( 12.13205353604972991, -140.1820037904669789, 2.500000000000000000 ) ) ;
#32089 = EDGE_CURVE ( 'NONE', #21999, #41940, #11654, .T. ) ;
#32090 = LINE ( 'NONE', #16911, #30177 ) ;
#32091 = CARTESIAN_POINT ( 'NONE',  ( -235.0000123116479926, -123.0000000000000284, 2.500000000000000000 ) ) ;
#32092 = DIRECTION ( 'NONE',  ( 0.000000000000000000, 0.000000000000000000, 1.000000000000000000 ) ) ;
#32093 = CARTESIAN_POINT ( 'NONE',  ( 0.000000000000000000, 0.000000000000000000, 0.000000000000000000 ) ) ;
#32094 = DIRECTION ( 'NONE',  ( 1.000000000000000000, -0.000000000000000000, -0.000000000000000000 ) ) ;
#32095 = ADVANCED_FACE ( 'NONE', ( #41281 ), #33913, .T. ) ;
#32096 = DIRECTION ( 'NONE',  ( 1.000000000000000000, 0.000000000000000000, 0.000000000000000000 ) ) ;
#32097 = CARTESIAN_POINT ( 'NONE',  ( 0.000000000000000000, -0.8299999999999999600, -1.199999999999999956 ) ) ;
#32098 = VERTEX_POINT ( 'NONE', #14618 ) ;
#32099 = ORIENTED_EDGE ( 'NONE', *, *, #12501, .T. ) ;
#32100 = AXIS2_PLACEMENT_3D ( 'NONE', #23612, #38556, #8209 ) ;
#32101 = EDGE_CURVE ( 'NONE', #19662, #35253, #36327, .T. ) ;
#32102 = CARTESIAN_POINT ( 'NONE',  ( 0.000000000000000000, -31.47745569255092235, -68.26794271651296242 ) ) ;
#32103 = VECTOR ( 'NONE', #11096, 1000.000000000000000 ) ;
#32104 = DIRECTION ( 'NONE',  ( 1.000000000000000000, 0.000000000000000000, 0.000000000000000000 ) ) ;
#32105 = AXIS2_PLACEMENT_3D ( 'NONE', #28985, #36573, #10390 ) ;
#32106 = CARTESIAN_POINT ( 'NONE',  ( 0.000000000000000000, 0.000000000000000000, 0.000000000000000000 ) ) ;
#32107 = ORIENTED_EDGE ( 'NONE', *, *, #11839, .T. ) ;
#32108 = CIRCLE ( 'NONE', #35999, 82.00000000000000000 ) ;
#32109 = AXIS2_PLACEMENT_3D ( 'NONE', #24300, #16002, #5702 ) ;
#32110 = EDGE_CURVE ( 'NONE', #5207, #18512, #12904, .T. ) ;
#32111 = ORIENTED_EDGE ( 'NONE', *, *, #19618, .T. ) ;
#32112 = AXIS2_PLACEMENT_3D ( 'NONE', #14671, #10511, #40380 ) ;
#32113 = ADVANCED_FACE ( 'NONE', ( #44457 ), #33444, .T. ) ;
#32114 = CARTESIAN_POINT ( 'NONE',  ( -42.50000000000000000, 0.000000000000000000, -20.99999999999999645 ) ) ;
#32115 = ORIENTED_EDGE ( 'NONE', *, *, #10889, .T. ) ;
#32116 = CARTESIAN_POINT ( 'NONE',  ( 10.00000000000000000, 0.000000000000000000, 0.000000000000000000 ) ) ;
#32117 = ORIENTED_EDGE ( 'NONE', *, *, #24262, .F. ) ;
#32119 = EDGE_CURVE ( 'NONE', #20650, #8908, #15248, .T. ) ;
#32118 = DIRECTION ( 'NONE',  ( 0.000000000000000000, -0.3826834323650772363, -0.9238795325112919565 ) ) ;
#32120 = DIRECTION ( 'NONE',  ( 0.000000000000000000, -0.07845909572783058006, -0.9969173337331290741 ) ) ;
#32121 = EDGE_CURVE ( 'NONE', #21044, #32290, #15563, .T. ) ;
#32122 = PLANE ( 'NONE',  #39117 ) ;
#32123 = ORIENTED_EDGE ( 'NONE', *, *, #32656, .T. ) ;
#32124 = CARTESIAN_POINT ( 'NONE',  ( -1.250000000000000444, -16.78109714094927085, -1.199999999999999956 ) ) ;
#32125 = ORIENTED_EDGE ( 'NONE', *, *, #21320, .T. ) ;
#32126 = ORIENTED_EDGE ( 'NONE', *, *, #48444, .F. ) ;
#32127 = FACE_BOUND ( 'NONE', #35236, .T. ) ;
#32128 = DIRECTION ( 'NONE',  ( 0.000000000000000000, -0.6691306063588662312, 0.7431448254773870277 ) ) ;
#32129 = CARTESIAN_POINT ( 'NONE',  ( -3.000000000000000000, 23.50000000000000000, 1.499999999999997780 ) ) ;
#32130 = AXIS2_PLACEMENT_3D ( 'NONE', #13095, #24595, #20671 ) ;
#32131 = CARTESIAN_POINT ( 'NONE',  ( -10.00000000000000000, 0.000000000000000000, 0.000000000000000000 ) ) ;
#32132 = CARTESIAN_POINT ( 'NONE',  ( 11.99999999999999822, 23.16143007188426850, 73.95703589263983702 ) ) ;
#32133 = ORIENTED_EDGE ( 'NONE', *, *, #40462, .T. ) ;
#32134 = VECTOR ( 'NONE', #17054, 1000.000000000000000 ) ;
#32135 = LINE ( 'NONE', #27499, #32637 ) ;
#32136 = VERTEX_POINT ( 'NONE', #3330 ) ;
#32137 = ORIENTED_EDGE ( 'NONE', *, *, #11163, .F. ) ;
#32138 = DIRECTION ( 'NONE',  ( 0.000000000000000000, -1.000000000000000000, -1.047444401652940007E-14 ) ) ;
#32139 = VECTOR ( 'NONE', #7556, 1000.000000000000000 ) ;
#32140 = FACE_OUTER_BOUND ( 'NONE', #28388, .T. ) ;
#32141 = LINE ( 'NONE', #32834, #44608 ) ;
#32142 = DIRECTION ( 'NONE',  ( 0.000000000000000000, 0.000000000000000000, 1.000000000000000000 ) ) ;
#32143 = ORIENTED_EDGE ( 'NONE', *, *, #44024, .F. ) ;
#32144 = DIRECTION ( 'NONE',  ( 0.000000000000000000, 0.000000000000000000, 1.000000000000000000 ) ) ;
#32145 = CARTESIAN_POINT ( 'NONE',  ( 10.00000000000000000, 0.000000000000000000, 0.000000000000000000 ) ) ;
#32146 = AXIS2_PLACEMENT_3D ( 'NONE', #2430, #2918, #6600 ) ;
#32147 = CARTESIAN_POINT ( 'NONE',  ( -12.00000000000000000, 0.000000000000000000, -17.30399999999999849 ) ) ;
#32148 = VECTOR ( 'NONE', #5176, 1000.000000000000114 ) ;
#32149 = DIRECTION ( 'NONE',  ( -1.000000000000000000, 0.000000000000000000, 0.000000000000000000 ) ) ;
#32150 = CARTESIAN_POINT ( 'NONE',  ( 5.000000000000002665, -15.33399622253423722, -80.55351364060604169 ) ) ;
#32151 = CIRCLE ( 'NONE', #19609, 16.00000000000000355 ) ;
#32152 = DIRECTION ( 'NONE',  ( 1.000000000000000000, -0.000000000000000000, 0.000000000000000000 ) ) ;
#32153 = DIRECTION ( 'NONE',  ( 1.000000000000000000, 0.000000000000000000, 0.000000000000000000 ) ) ;
#32154 = CARTESIAN_POINT ( 'NONE',  ( 10.00000000000000000, 0.000000000000000000, 0.000000000000000000 ) ) ;
#32155 = DIRECTION ( 'NONE',  ( 0.000000000000000000, 0.2079116908177664758, -0.9781476007338042455 ) ) ;
#32156 = CARTESIAN_POINT ( 'NONE',  ( -42.50000000000000000, 0.000000000000000000, 0.000000000000000000 ) ) ;
#32157 = CARTESIAN_POINT ( 'NONE',  ( 10.00000000000000000, 5.202137450156389953, 37.22597642581160216 ) ) ;
#32158 = EDGE_LOOP ( 'NONE', ( #13613, #27234, #15664, #28729 ) ) ;
#32159 = CARTESIAN_POINT ( 'NONE',  ( 10.00000000000000000, -20.40083707022935400, 72.35432306680478121 ) ) ;
#32160 = ORIENTED_EDGE ( 'NONE', *, *, #4442, .F. ) ;
#32161 = CARTESIAN_POINT ( 'NONE',  ( 0.000000000000000000, 0.000000000000000000, 0.000000000000000000 ) ) ;
#32162 = EDGE_CURVE ( 'NONE', #28196, #2440, #23083, .T. ) ;
#32163 = DIRECTION ( 'NONE',  ( 0.000000000000000000, 0.000000000000000000, -1.000000000000000000 ) ) ;
#32164 = ORIENTED_EDGE ( 'NONE', *, *, #645, .T. ) ;
#32165 = CIRCLE ( 'NONE', #29806, 15.77977592589476608 ) ;
#32166 = AXIS2_PLACEMENT_3D ( 'NONE', #8274, #8995, #5334 ) ;
#32167 = DIRECTION ( 'NONE',  ( -1.000000000000000000, -0.000000000000000000, -0.000000000000000000 ) ) ;
#32168 = VERTEX_POINT ( 'NONE', #3581 ) ;
#32170 = ADVANCED_FACE ( 'NONE', ( #14849 ), #29764, .T. ) ;
#32169 = ORIENTED_EDGE ( 'NONE', *, *, #19388, .F. ) ;
#32171 = ORIENTED_EDGE ( 'NONE', *, *, #7667, .T. ) ;
#32172 = VECTOR ( 'NONE', #19295, 1000.000000000000000 ) ;
#32173 = ADVANCED_FACE ( 'NONE', ( #23383 ), #42233, .T. ) ;
#32174 = EDGE_CURVE ( 'NONE', #47607, #35673, #28582, .T. ) ;
#32175 = EDGE_CURVE ( 'NONE', #1742, #337, #29340, .T. ) ;
#32176 = DIRECTION ( 'NONE',  ( 0.000000000000000000, 0.3090169943749450088, -0.9510565162951543083 ) ) ;
#32177 = AXIS2_PLACEMENT_3D ( 'NONE', #15287, #18458, #44890 ) ;
#32178 = EDGE_CURVE ( 'NONE', #17758, #32256, #34886, .T. ) ;
#32179 = CARTESIAN_POINT ( 'NONE',  ( 0.000000000000000000, 63.18004540533029001, 44.88180994100398635 ) ) ;
#32180 = CARTESIAN_POINT ( 'NONE',  ( 5.822613034544236399, -142.8165987265839476, -2.500000000000000000 ) ) ;
#32181 = CIRCLE ( 'NONE', #24337, 37.49900000000000233 ) ;
#32182 = ORIENTED_EDGE ( 'NONE', *, *, #46680, .T. ) ;
#32183 = CARTESIAN_POINT ( 'NONE',  ( 6.000000000000000000, -8.966570791701288456, 81.50828551894223040 ) ) ;
#32184 = EDGE_CURVE ( 'NONE', #2237, #26319, #1112, .T. ) ;
#32185 = VERTEX_POINT ( 'NONE', #1368 ) ;
#32186 = DIRECTION ( 'NONE',  ( -1.000000000000000000, 0.000000000000000000, 0.000000000000000000 ) ) ;
#32187 = LINE ( 'NONE', #47571, #6977 ) ;
#32188 = CARTESIAN_POINT ( 'NONE',  ( 3.429551818649054340, -146.3199197248623875, -2.500000000000000444 ) ) ;
#32189 = ORIENTED_EDGE ( 'NONE', *, *, #31077, .F. ) ;
#32190 = CARTESIAN_POINT ( 'NONE',  ( 10.00000000000000000, -54.21277698773636899, -55.38113227695839669 ) ) ;
#32191 = EDGE_LOOP ( 'NONE', ( #15308, #36552, #9653, #25815 ) ) ;
#32192 = DIRECTION ( 'NONE',  ( 0.000000000000000000, 0.9723699203976773342, -0.2334453638559024213 ) ) ;
#32193 = ADVANCED_FACE ( 'NONE', ( #35120 ), #39048, .T. ) ;
#32194 = DIRECTION ( 'NONE',  ( -1.000000000000000000, -0.000000000000000000, -0.000000000000000000 ) ) ;
#32195 = CARTESIAN_POINT ( 'NONE',  ( 10.00000000000000000, 21.32104025579114648, 30.84782396557224970 ) ) ;
#32196 = CARTESIAN_POINT ( 'NONE',  ( 0.000000000000000000, 55.19960302592141232, -51.03279382321027668 ) ) ;
#32197 = CYLINDRICAL_SURFACE ( 'NONE', #13564, 77.49899999999999523 ) ;
#32198 = DIRECTION ( 'NONE',  ( 0.000000000000000000, 0.000000000000000000, 1.000000000000000000 ) ) ;
#32199 = EDGE_CURVE ( 'NONE', #33470, #33708, #9187, .T. ) ;
#32200 = CARTESIAN_POINT ( 'NONE',  ( -8.637688417678527131, 13.69818742750669394, 42.00000000000001421 ) ) ;
#32201 = CARTESIAN_POINT ( 'NONE',  ( 10.00000000000000000, -71.91182617369167929, -28.89263327155822481 ) ) ;
#32202 = VECTOR ( 'NONE', #20566, 1000.000000000000000 ) ;
#32203 = CARTESIAN_POINT ( 'NONE',  ( 5.000000000000002665, 16.65972982744934683, 80.28980883073764119 ) ) ;
#32204 = CARTESIAN_POINT ( 'NONE',  ( 0.000000000000000000, 0.000000000000000000, 0.000000000000000000 ) ) ;
#32205 = ORIENTED_EDGE ( 'NONE', *, *, #30842, .F. ) ;
#32206 = CONICAL_SURFACE ( 'NONE', #47792, 17.30399999999999849, 0.2094395102393129815 ) ;
#32207 = ORIENTED_EDGE ( 'NONE', *, *, #17572, .T. ) ;
#32208 = DIRECTION ( 'NONE',  ( 0.000000000000000000, 0.000000000000000000, 1.000000000000000000 ) ) ;
#32209 = AXIS2_PLACEMENT_3D ( 'NONE', #14723, #10806, #7123 ) ;
#32210 = PLANE ( 'NONE',  #11891 ) ;
#32211 = CARTESIAN_POINT ( 'NONE',  ( -3.249999999999999556, -13.95926121303099343, -1.199999999999999956 ) ) ;
#32212 = CIRCLE ( 'NONE', #22832, 31.99999999999998579 ) ;
#32213 = CARTESIAN_POINT ( 'NONE',  ( 0.000000000000000000, 0.000000000000000000, 0.000000000000000000 ) ) ;
#32214 = EDGE_CURVE ( 'NONE', #30774, #47208, #31233, .T. ) ;
#32215 = CARTESIAN_POINT ( 'NONE',  ( -17.26469406256017791, -140.1601175325492648, 5.500000000000000000 ) ) ;
#32216 = DIRECTION ( 'NONE',  ( -1.000000000000000000, 0.000000000000000000, -0.000000000000000000 ) ) ;
#32217 = ORIENTED_EDGE ( 'NONE', *, *, #5083, .T. ) ;
#32218 = CARTESIAN_POINT ( 'NONE',  ( 0.000000000000000000, 80.55351364060611274, -15.33399622253397609 ) ) ;
#32219 = AXIS2_PLACEMENT_3D ( 'NONE', #20014, #28092, #35677 ) ;
#32220 = ADVANCED_FACE ( 'NONE', ( #46156 ), #16532, .T. ) ;
#32221 = VERTEX_POINT ( 'NONE', #34386 ) ;
#32222 = ADVANCED_FACE ( 'NONE', ( #27315 ), #30744, .T. ) ;
#32223 = DIRECTION ( 'NONE',  ( -1.000000000000000000, 0.000000000000000000, 0.000000000000000000 ) ) ;
#32224 = ORIENTED_EDGE ( 'NONE', *, *, #7893, .F. ) ;
#32225 = EDGE_LOOP ( 'NONE', ( #27055, #22794, #21620, #24908 ) ) ;
#32226 = ORIENTED_EDGE ( 'NONE', *, *, #46970, .T. ) ;
#32227 = CIRCLE ( 'NONE', #27536, 77.49899999999999523 ) ;
#32228 = DIRECTION ( 'NONE',  ( 0.000000000000000000, 0.000000000000000000, 1.000000000000000000 ) ) ;
#32229 = ORIENTED_EDGE ( 'NONE', *, *, #11804, .T. ) ;
#32230 = EDGE_CURVE ( 'NONE', #15196, #41616, #8242, .T. ) ;
#32231 = EDGE_CURVE ( 'NONE', #48059, #24460, #34819, .T. ) ;
#32232 = AXIS2_PLACEMENT_3D ( 'NONE', #39564, #47125, #14077 ) ;
#32233 = CARTESIAN_POINT ( 'NONE',  ( 0.000000000000000000, 77.16300072079660310, 27.74655509720697211 ) ) ;
#32234 = CARTESIAN_POINT ( 'NONE',  ( 10.00000000000000000, -30.84782396557201878, -21.32104025579148399 ) ) ;
#32235 = ORIENTED_EDGE ( 'NONE', *, *, #36679, .F. ) ;
#32236 = VERTEX_POINT ( 'NONE', #38824 ) ;
#32237 = ORIENTED_EDGE ( 'NONE', *, *, #12606, .T. ) ;
#32238 = CIRCLE ( 'NONE', #3319, 31.99999999999998934 ) ;
#32239 = CYLINDRICAL_SURFACE ( 'NONE', #17036, 77.49899999999999523 ) ;
#32240 = PRODUCT_RELATED_PRODUCT_CATEGORY ( 'part', '', ( #6195 ) ) ;
#32242 = EDGE_LOOP ( 'NONE', ( #40650, #11537, #43196, #2234 ) ) ;
#32241 = DIRECTION ( 'NONE',  ( 0.000000000000000000, 0.000000000000000000, 1.000000000000000000 ) ) ;
#32243 = CARTESIAN_POINT ( 'NONE',  ( 0.000000000000000000, 0.000000000000000000, 0.000000000000000000 ) ) ;
#32244 = EDGE_LOOP ( 'NONE', ( #34624, #36204, #84, #8030 ) ) ;
#32245 = ORIENTED_EDGE ( 'NONE', *, *, #21828, .T. ) ;
#32246 = CARTESIAN_POINT ( 'NONE',  ( 114.1267819554180392, -82.91796067500511924, -5.500000000000000000 ) ) ;
#32247 = ORIENTED_EDGE ( 'NONE', *, *, #507, .T. ) ;
#32248 = DIRECTION ( 'NONE',  ( -1.000000000000000000, -0.000000000000000000, 0.000000000000000000 ) ) ;
#32249 = CARTESIAN_POINT ( 'NONE',  ( 0.000000000000000000, -22.67460108101774807, -6.353146135318215038 ) ) ;
#32250 = AXIS2_PLACEMENT_3D ( 'NONE', #16560, #45222, #26615 ) ;
#32251 = FACE_BOUND ( 'NONE', #47785, .T. ) ;
#32252 = CARTESIAN_POINT ( 'NONE',  ( 0.000000000000000000, 70.53064760720316428, -26.01480285779861035 ) ) ;
#32253 = CARTESIAN_POINT ( 'NONE',  ( -21.33958957442910886, -129.9559990355020034, 5.500000000000000000 ) ) ;
#32254 = CARTESIAN_POINT ( 'NONE',  ( 10.00000000000000000, 0.000000000000000000, 0.000000000000000000 ) ) ;
#32255 = DIRECTION ( 'NONE',  ( 0.000000000000000000, 0.000000000000000000, 1.000000000000000000 ) ) ;
#32256 = VERTEX_POINT ( 'NONE', #45665 ) ;
#32257 = CARTESIAN_POINT ( 'NONE',  ( 10.00000000000000000, 76.41127070299273782, 12.93880638057342836 ) ) ;
#32258 = VERTEX_POINT ( 'NONE', #5284 ) ;
#32259 = AXIS2_PLACEMENT_3D ( 'NONE', #14912, #18334, #25664 ) ;
#32260 = DIRECTION ( 'NONE',  ( -1.000000000000000000, -0.000000000000000000, -0.000000000000000000 ) ) ;
#32261 = FACE_OUTER_BOUND ( 'NONE', #27404, .T. ) ;
#32262 = DIRECTION ( 'NONE',  ( 0.000000000000000000, 0.8090169943749487835, -0.5877852522924713607 ) ) ;
#32263 = CARTESIAN_POINT ( 'NONE',  ( 5.000000000000000000, -31.52238457039619490, 27.75498641678731104 ) ) ;
#32264 = LINE ( 'NONE', #35698, #21019 ) ;
#32265 = LINE ( 'NONE', #27631, #38856 ) ;
#32267 = ORIENTED_EDGE ( 'NONE', *, *, #8962, .F. ) ;
#32266 = VECTOR ( 'NONE', #37722, 1000.000000000000000 ) ;
#32268 = EDGE_CURVE ( 'NONE', #35892, #40544, #5106, .T. ) ;
#32269 = DIRECTION ( 'NONE',  ( 0.000000000000000000, 0.7431448254773862505, 0.6691306063588671194 ) ) ;
#32270 = DIRECTION ( 'NONE',  ( 0.000000000000000000, -1.156482317317870936E-15, -1.000000000000000000 ) ) ;
#32271 = DIRECTION ( 'NONE',  ( 0.000000000000000000, 0.9510565162951523099, 0.3090169943749514481 ) ) ;
#32272 = ADVANCED_FACE ( 'NONE', ( #5515 ), #45918, .T. ) ;
#32273 = AXIS2_PLACEMENT_3D ( 'NONE', #1428, #12684, #1663 ) ;
#32274 = FACE_OUTER_BOUND ( 'NONE', #26334, .T. ) ;
#32275 = ADVANCED_FACE ( 'NONE', ( #30493 ), #45416, .T. ) ;
#32276 = CIRCLE ( 'NONE', #8047, 31.99999999999998579 ) ;
#32277 = ORIENTED_EDGE ( 'NONE', *, *, #42893, .F. ) ;
#32278 = VERTEX_POINT ( 'NONE', #21649 ) ;
#32279 = AXIS2_PLACEMENT_3D ( 'NONE', #37846, #1612, #16538 ) ;
#32280 = VECTOR ( 'NONE', #27050, 1000.000000000000000 ) ;
#32281 = CARTESIAN_POINT ( 'NONE',  ( 10.00000000000000000, 6.736453364084091788, -36.88895765772625879 ) ) ;
#32282 = DIRECTION ( 'NONE',  ( -1.000000000000000000, -0.000000000000000000, -0.000000000000000000 ) ) ;
#32283 = EDGE_LOOP ( 'NONE', ( #15449, #48353, #18159, #29042 ) ) ;
#32284 = EDGE_CURVE ( 'NONE', #7344, #7731, #31709, .T. ) ;
#32285 = EDGE_CURVE ( 'NONE', #17381, #19503, #14060, .T. ) ;
#32286 = ADVANCED_FACE ( 'NONE', ( #36570, #28982 ), #39549, .F. ) ;
#32287 = CARTESIAN_POINT ( 'NONE',  ( 5.000000000000000000, 51.29473840253223926, 63.97538442413444670 ) ) ;
#32288 = ORIENTED_EDGE ( 'NONE', *, *, #11066, .T. ) ;
#32289 = ORIENTED_EDGE ( 'NONE', *, *, #31126, .F. ) ;
#32290 = VERTEX_POINT ( 'NONE', #10145 ) ;
#32291 = VECTOR ( 'NONE', #13027, 1000.000000000000000 ) ;
#32292 = AXIS2_PLACEMENT_3D ( 'NONE', #20328, #15709, #35028 ) ;
#32293 = EDGE_CURVE ( 'NONE', #5676, #293, #40016, .T. ) ;
#32294 = DIRECTION ( 'NONE',  ( 0.000000000000000000, 0.000000000000000000, -1.000000000000000000 ) ) ;
#32295 = EDGE_LOOP ( 'NONE', ( #29424, #41568, #45450, #2170 ) ) ;
#32296 = CARTESIAN_POINT ( 'NONE',  ( 10.00000000000000000, 0.6853352020795618893, -37.58145647212453611 ) ) ;
#32297 = ORIENTED_EDGE ( 'NONE', *, *, #21833, .T. ) ;
#32298 = CARTESIAN_POINT ( 'NONE',  ( 15.00000000000000000, 24.81905959214275370, 9.408202855044498492 ) ) ;
#32299 = AXIS2_PLACEMENT_3D ( 'NONE', #22047, #36978, #3450 ) ;
#32300 = AXIS2_PLACEMENT_3D ( 'NONE', #18263, #10448, #21466 ) ;
#32301 = DIRECTION ( 'NONE',  ( -1.000000000000000000, 0.000000000000000000, 0.000000000000000000 ) ) ;
#32302 = CYLINDRICAL_SURFACE ( 'NONE', #46310, 32.00000000000000000 ) ;
#32303 = VECTOR ( 'NONE', #40863, 1000.000000000000000 ) ;
#32304 = ORIENTED_EDGE ( 'NONE', *, *, #30655, .F. ) ;
#32305 = DIRECTION ( 'NONE',  ( -1.000000000000000000, -0.000000000000000000, 0.000000000000000000 ) ) ;
#32306 = VERTEX_POINT ( 'NONE', #36335 ) ;
#32307 = DIRECTION ( 'NONE',  ( 0.000000000000000000, -0.4067366430757887730, 0.9135454576426059736 ) ) ;
#32308 = CARTESIAN_POINT ( 'NONE',  ( 10.00000000000000000, 70.52718814184260054, 26.02418014898334420 ) ) ;
#32309 = AXIS2_PLACEMENT_3D ( 'NONE', #45872, #42426, #23338 ) ;
#32310 = ORIENTED_EDGE ( 'NONE', *, *, #24289, .F. ) ;
#32311 = ORIENTED_EDGE ( 'NONE', *, *, #5083, .F. ) ;
#32312 = CARTESIAN_POINT ( 'NONE',  ( 10.00000000000000000, 0.000000000000000000, 0.000000000000000000 ) ) ;
#32313 = DIRECTION ( 'NONE',  ( -1.000000000000000000, 0.000000000000000000, -0.000000000000000000 ) ) ;
#32314 = ORIENTED_EDGE ( 'NONE', *, *, #12058, .T. ) ;
#32315 = ORIENTED_EDGE ( 'NONE', *, *, #2477, .T. ) ;
#32316 = AXIS2_PLACEMENT_3D ( 'NONE', #23306, #11578, #26502 ) ;
#32317 = CARTESIAN_POINT ( 'NONE',  ( 11.99999999999999822, -46.21855187248585395, -62.20884554314068993 ) ) ;
#32318 = DIRECTION ( 'NONE',  ( 0.000000000000000000, -0.7071067811865536790, 0.7071067811865413555 ) ) ;
#32319 = DIRECTION ( 'NONE',  ( 1.000000000000000000, 0.000000000000000000, 0.000000000000000000 ) ) ;
#32320 = CARTESIAN_POINT ( 'NONE',  ( 12.00000000000000000, -26.23277895567245466, 4.042438405570107918 ) ) ;
#32321 = AXIS2_PLACEMENT_3D ( 'NONE', #46625, #5999, #12604 ) ;
#32322 = DIRECTION ( 'NONE',  ( -1.000000000000000000, -0.000000000000000000, 0.000000000000000000 ) ) ;
#32323 = DIRECTION ( 'NONE',  ( 0.000000000000000000, 0.4539904997395477482, -0.8910065241883673437 ) ) ;
#32324 = CARTESIAN_POINT ( 'NONE',  ( 10.00000000000000000, 70.52718814184294160, -26.02418014898236720 ) ) ;
#32325 = EDGE_CURVE ( 'NONE', #42578, #15938, #46642, .T. ) ;
#32326 = LINE ( 'NONE', #36471, #24456 ) ;
#32327 = DIRECTION ( 'NONE',  ( -1.000000000000000000, -0.000000000000000000, -0.000000000000000000 ) ) ;
#32328 = CARTESIAN_POINT ( 'NONE',  ( -3.000000000000000000, -20.55727247249726020, -16.78983467731313084 ) ) ;
#32329 = EDGE_CURVE ( 'NONE', #12921, #31098, #22331, .T. ) ;
#32330 = FACE_OUTER_BOUND ( 'NONE', #22768, .T. ) ;
#32331 = FACE_OUTER_BOUND ( 'NONE', #3629, .T. ) ;
#32332 = EDGE_CURVE ( 'NONE', #23927, #5207, #30121, .T. ) ;
#32333 = EDGE_LOOP ( 'NONE', ( #32655, #4432, #10480, #9413 ) ) ;
#32334 = AXIS2_PLACEMENT_3D ( 'NONE', #34972, #26670, #41598 ) ;
#32335 = ORIENTED_EDGE ( 'NONE', *, *, #33559, .F. ) ;
#32336 = ORIENTED_EDGE ( 'NONE', *, *, #31918, .F. ) ;
#32337 = EDGE_CURVE ( 'NONE', #40687, #23501, #43434, .T. ) ;
#32338 = ADVANCED_FACE ( 'NONE', ( #43917 ), #38730, .T. ) ;
#32339 = CARTESIAN_POINT ( 'NONE',  ( 10.00000000000000000, 68.26794271651307611, -31.47745569255064169 ) ) ;
#32340 = CIRCLE ( 'NONE', #36236, 31.99999999999999645 ) ;
#32341 = AXIS2_PLACEMENT_3D ( 'NONE', #18518, #7012, #32719 ) ;
#32342 = AXIS2_PLACEMENT_3D ( 'NONE', #16438, #23534, #38473 ) ;
#32343 = CONTEXT_DEPENDENT_SHAPE_REPRESENTATION ( #44165, #29261 ) ;
#32344 = DIRECTION ( 'NONE',  ( 0.000000000000000000, 0.000000000000000000, -1.000000000000000000 ) ) ;
#32345 = ORIENTED_EDGE ( 'NONE', *, *, #16680, .F. ) ;
#32346 = EDGE_CURVE ( 'NONE', #42296, #20697, #16780, .T. ) ;
#32347 = CIRCLE ( 'NONE', #46429, 15.77977592589476608 ) ;
#32348 = ADVANCED_FACE ( 'NONE', ( #17007, #47581, #6015, #2094, #35620, #36092, #31730, #13107, #28040, #9659, #35849, #28756, #24606, #13837, #42966, #9417, #31963 ), #5764, .F. ) ;
#32349 = AXIS2_PLACEMENT_3D ( 'NONE', #1498, #30885, #24243 ) ;
#32350 = DIRECTION ( 'NONE',  ( -1.000000000000000000, -0.000000000000000000, -0.000000000000000000 ) ) ;
#32351 = VECTOR ( 'NONE', #6872, 1000.000000000000000 ) ;
#32352 = EDGE_LOOP ( 'NONE', ( #27867, #30854, #8198, #3329 ) ) ;
#32353 = CARTESIAN_POINT ( 'NONE',  ( -5.250000000000000888, -13.95926121303099343, 0.000000000000000000 ) ) ;
#32354 = VERTEX_POINT ( 'NONE', #2549 ) ;
#32355 = VECTOR ( 'NONE', #36784, 1000.000000000000114 ) ;
#32356 = EDGE_CURVE ( 'NONE', #9579, #36733, #28520, .T. ) ;
#32357 = ORIENTED_EDGE ( 'NONE', *, *, #42942, .T. ) ;
#32358 = DIRECTION ( 'NONE',  ( 0.000000000000000000, -1.000000000000000000, -1.040834085586084414E-14 ) ) ;
#32359 = DIRECTION ( 'NONE',  ( 0.9135454576426004225, 0.4067366430758009854, 0.000000000000000000 ) ) ;
#32360 = LINE ( 'NONE', #40651, #44674 ) ;
#32361 = VERTEX_POINT ( 'NONE', #32434 ) ;
#32362 = VERTEX_POINT ( 'NONE', #30213 ) ;
#32363 = DIRECTION ( 'NONE',  ( 0.000000000000000000, 0.000000000000000000, 1.000000000000000000 ) ) ;
#32364 = DIRECTION ( 'NONE',  ( -0.8774505977381983346, -0.4796670183876294291, 0.000000000000000000 ) ) ;
#32365 = CARTESIAN_POINT ( 'NONE',  ( 0.000000000000000000, 0.000000000000000000, 42.00000000000001421 ) ) ;
#32366 = AXIS2_PLACEMENT_3D ( 'NONE', #25393, #40351, #6809 ) ;
#32367 = EDGE_CURVE ( 'NONE', #6884, #7063, #332, .T. ) ;
#32368 = LINE ( 'NONE', #13516, #14846 ) ;
#32369 = CIRCLE ( 'NONE', #37033, 82.00000000000000000 ) ;
#32370 = CARTESIAN_POINT ( 'NONE',  ( 10.00000000000000000, -21.60688246758641995, 79.10210256391358996 ) ) ;
#32371 = ORIENTED_EDGE ( 'NONE', *, *, #28127, .F. ) ;
#32372 = FACE_OUTER_BOUND ( 'NONE', #24163, .T. ) ;
#32373 = EDGE_LOOP ( 'NONE', ( #35036, #31640, #6711, #21963 ) ) ;
#32374 = ORIENTED_EDGE ( 'NONE', *, *, #31922, .F. ) ;
#32375 = AXIS2_PLACEMENT_3D ( 'NONE', #37916, #8294, #26420 ) ;
#32376 = DIRECTION ( 'NONE',  ( -1.000000000000000000, 0.000000000000000000, -0.000000000000000000 ) ) ;
#32377 = ORIENTED_EDGE ( 'NONE', *, *, #13830, .F. ) ;
#32378 = AXIS2_PLACEMENT_3D ( 'NONE', #25091, #14081, #21421 ) ;
#32379 = DIRECTION ( 'NONE',  ( 0.000000000000000000, 0.3090169943749482839, -0.9510565162951533091 ) ) ;
#32380 = CARTESIAN_POINT ( 'NONE',  ( 11.99999999999999822, -8.830959090342926032, 74.65491531819115778 ) ) ;
#32381 = DIRECTION ( 'NONE',  ( 0.000000000000000000, 0.8910065241883656784, 0.4539904997395511344 ) ) ;
#32382 = ORIENTED_EDGE ( 'NONE', *, *, #37750, .T. ) ;
#32383 = CARTESIAN_POINT ( 'NONE',  ( -22.53294031248082163, -134.0273518838794757, 5.500000000000000000 ) ) ;
#32384 = PRODUCT_DEFINITION_SHAPE ( 'NONE', 'NONE',  #28304 ) ;
#32385 = CARTESIAN_POINT ( 'NONE',  ( 11.99999999999999822, -2.543863470247810010, -81.96053171279903893 ) ) ;
#32386 = CARTESIAN_POINT ( 'NONE',  ( 0.000000000000000000, 44.99326035066149387, -68.55367621811095091 ) ) ;
#32387 = CARTESIAN_POINT ( 'NONE',  ( 20.10151712711562766, -102.7321394148470830, 2.500000000000000000 ) ) ;
#32388 = AXIS2_PLACEMENT_3D ( 'NONE', #1808, #2281, #9871 ) ;
#32389 = CARTESIAN_POINT ( 'NONE',  ( 0.000000000000000000, -71.91182617369167929, -28.89263327155821059 ) ) ;
#32390 = DIRECTION ( 'NONE',  ( -1.000000000000000000, 0.000000000000000000, -0.000000000000000000 ) ) ;
#32391 = DIRECTION ( 'NONE',  ( 0.000000000000000000, 0.000000000000000000, -1.000000000000000000 ) ) ;
#32393 = AXIS2_PLACEMENT_3D ( 'NONE', #34464, #23961, #12697 ) ;
#32392 = CARTESIAN_POINT ( 'NONE',  ( -34.02017708624681092, -130.1428571428571388, 102.9091629284897493 ) ) ;
#32394 = ADVANCED_FACE ( 'NONE', ( #48074 ), #40498, .T. ) ;
#32395 = CIRCLE ( 'NONE', #21436, 31.99999999999998934 ) ;
#32396 = DIRECTION ( 'NONE',  ( -1.000000000000000000, -0.000000000000000000, -0.000000000000000000 ) ) ;
#32397 = CARTESIAN_POINT ( 'NONE',  ( 10.00000000000000178, 0.000000000000000000, 0.000000000000000000 ) ) ;
#32398 = AXIS2_PLACEMENT_3D ( 'NONE', #28048, #1614, #8468 ) ;
#32399 = EDGE_CURVE ( 'NONE', #32891, #2211, #11601, .T. ) ;
#32400 = EDGE_LOOP ( 'NONE', ( #32792, #46044, #7446, #9746 ) ) ;
#32401 = CARTESIAN_POINT ( 'NONE',  ( 12.00000000000000000, 20.85821328998741109, -10.92862929874522671 ) ) ;
#32402 = ORIENTED_EDGE ( 'NONE', *, *, #20960, .F. ) ;
#32403 = EDGE_CURVE ( 'NONE', #39728, #46150, #39524, .T. ) ;
#32404 = CARTESIAN_POINT ( 'NONE',  ( 0.000000000000000000, -22.64427369931148348, -30.00120703465229965 ) ) ;
#32405 = CIRCLE ( 'NONE', #11295, 77.49899999999999523 ) ;
#32406 = DIRECTION ( 'NONE',  ( -1.000000000000000000, 0.000000000000000000, 0.000000000000000000 ) ) ;
#32407 = ORIENTED_EDGE ( 'NONE', *, *, #31414, .T. ) ;
#32408 = VECTOR ( 'NONE', #39427, 1000.000000000000000 ) ;
#32409 = AXIS2_PLACEMENT_3D ( 'NONE', #14829, #9515, #37095 ) ;
#32410 = CIRCLE ( 'NONE', #10531, 16.00000000000000000 ) ;
#32411 = CARTESIAN_POINT ( 'NONE',  ( 0.000000000000000000, 0.000000000000000000, 0.000000000000000000 ) ) ;
#32412 = ORIENTED_EDGE ( 'NONE', *, *, #37693, .F. ) ;
#32413 = VECTOR ( 'NONE', #34094, 1000.000000000000114 ) ;
#32414 = ORIENTED_EDGE ( 'NONE', *, *, #37524, .T. ) ;
#32415 = EDGE_LOOP ( 'NONE', ( #9406, #6226, #28546, #27923 ) ) ;
#32416 = AXIS2_PLACEMENT_3D ( 'NONE', #124, #44933, #29026 ) ;
#32417 = CIRCLE ( 'NONE', #22243, 37.49900000000000944 ) ;
#32418 = DIRECTION ( 'NONE',  ( 0.000000000000000000, -0.07845909572785224328, 0.9969173337331274087 ) ) ;
#32419 = CIRCLE ( 'NONE', #28503, 82.00000000000000000 ) ;
#32420 = CARTESIAN_POINT ( 'NONE',  ( 5.822613034544236399, -142.8165987265839760, -5.500000000000000000 ) ) ;
#32421 = DIRECTION ( 'NONE',  ( 0.6516173805718078471, -0.7585478161175706058, 0.000000000000000000 ) ) ;
#32422 = VERTEX_POINT ( 'NONE', #26528 ) ;
#32423 = LINE ( 'NONE', #47352, #35593 ) ;
#32424 = AXIS2_PLACEMENT_3D ( 'NONE', #45541, #1492, #41639 ) ;
#32425 = VERTEX_POINT ( 'NONE', #41457 ) ;
#32426 = AXIS2_PLACEMENT_3D ( 'NONE', #21657, #21165, #40024 ) ;
#32427 = CARTESIAN_POINT ( 'NONE',  ( 10.00000000000000000, -6.736453364083817341, 36.88895765772630142 ) ) ;
#32428 = CARTESIAN_POINT ( 'NONE',  ( 12.49999999999999645, 1.530808498934191127E-15, 125.0000000000000000 ) ) ;
#32429 = CARTESIAN_POINT ( 'NONE',  ( 5.000000000000000000, 26.79245525562714292, 32.34446384429980981 ) ) ;
#32430 = ORIENTED_EDGE ( 'NONE', *, *, #33289, .T. ) ;
#32431 = CARTESIAN_POINT ( 'NONE',  ( 0.000000000000000000, -89.50000000000000000, 5.500000000000000000 ) ) ;
#32432 = ORIENTED_EDGE ( 'NONE', *, *, #23446, .F. ) ;
#32433 = ORIENTED_EDGE ( 'NONE', *, *, #34114, .T. ) ;
#32434 = CARTESIAN_POINT ( 'NONE',  ( 15.00000000000000000, 26.50000000000000355, -1.500000000000000000 ) ) ;
#32435 = CARTESIAN_POINT ( 'NONE',  ( -11.59999999999999787, 0.000000000000000000, -54.99999999999998579 ) ) ;
#32436 = DIRECTION ( 'NONE',  ( -1.000000000000000000, -0.000000000000000000, -0.000000000000000000 ) ) ;
#32437 = DIRECTION ( 'NONE',  ( -2.889240119132116694E-16, 1.000000000000000000, 0.000000000000000000 ) ) ;
#32438 = CARTESIAN_POINT ( 'NONE',  ( 10.00000000000000000, 0.000000000000000000, 0.000000000000000000 ) ) ;
#32439 = DIRECTION ( 'NONE',  ( 0.000000000000000000, 0.000000000000000000, -1.000000000000000000 ) ) ;
#32440 = CARTESIAN_POINT ( 'NONE',  ( 11.99999999999999822, 76.66974797899852945, -11.30684508768257679 ) ) ;
#32441 = CARTESIAN_POINT ( 'NONE',  ( 10.00000000000000000, -2.956366410621191765, 75.11725578898467859 ) ) ;
#32442 = DIRECTION ( 'NONE',  ( 0.000000000000000000, -0.8910065241883722287, 0.4539904997395383113 ) ) ;
#32443 = EDGE_CURVE ( 'NONE', #36248, #46672, #41070, .T. ) ;
#32444 = CARTESIAN_POINT ( 'NONE',  ( 11.99999999999999822, 18.89407956138362010, -75.16055320797013906 ) ) ;
#32445 = VERTEX_POINT ( 'NONE', #33856 ) ;
#32446 = ORIENTED_EDGE ( 'NONE', *, *, #42437, .F. ) ;
#32447 = FACE_OUTER_BOUND ( 'NONE', #7765, .T. ) ;
#32448 = EDGE_CURVE ( 'NONE', #38691, #10422, #21514, .T. ) ;
#32449 = AXIS2_PLACEMENT_3D ( 'NONE', #36571, #40499, #44644 ) ;
#32450 = CARTESIAN_POINT ( 'NONE',  ( 0.000000000000000000, 76.41127070299273782, 12.93880638057342836 ) ) ;
#32451 = CARTESIAN_POINT ( 'NONE',  ( 4.999999999999999112, -41.81611651403864727, 3.925862922256025289 ) ) ;
#32452 = EDGE_CURVE ( 'NONE', #9566, #37777, #34012, .T. ) ;
#32453 = FACE_OUTER_BOUND ( 'NONE', #38638, .T. ) ;
#32454 = VECTOR ( 'NONE', #15498, 1000.000000000000000 ) ;
#32455 = VECTOR ( 'NONE', #31757, 1000.000000000000000 ) ;
#32456 = CARTESIAN_POINT ( 'NONE',  ( 10.00000000000000000, 58.39081064771751528, 50.95692526931350841 ) ) ;
#32457 = CARTESIAN_POINT ( 'NONE',  ( 10.00000000000000000, 0.000000000000000000, 0.000000000000000000 ) ) ;
#32458 = ORIENTED_EDGE ( 'NONE', *, *, #506, .F. ) ;
#32459 = EDGE_CURVE ( 'NONE', #13395, #7073, #19164, .T. ) ;
#32460 = CARTESIAN_POINT ( 'NONE',  ( 10.00000000000000000, 12.42422080174688404, -35.38097989696498047 ) ) ;
#32461 = CIRCLE ( 'NONE', #12174, 42.00000000000000000 ) ;
#32462 = EDGE_CURVE ( 'NONE', #15896, #35257, #18200, .T. ) ;
#32463 = LINE ( 'NONE', #28780, #19711 ) ;
#32464 = ORIENTED_EDGE ( 'NONE', *, *, #25216, .T. ) ;
#32465 = ORIENTED_EDGE ( 'NONE', *, *, #8180, .T. ) ;
#32466 = EDGE_CURVE ( 'NONE', #22705, #13922, #44191, .T. ) ;
#32467 = AXIS2_PLACEMENT_3D ( 'NONE', #22271, #36935, #37194 ) ;
#32468 = CARTESIAN_POINT ( 'NONE',  ( 11.99999999999999822, 0.000000000000000000, 0.000000000000000000 ) ) ;
#32469 = ORIENTED_EDGE ( 'NONE', *, *, #98, .F. ) ;
#32470 = ORIENTED_EDGE ( 'NONE', *, *, #24318, .F. ) ;
#32471 = CIRCLE ( 'NONE', #16862, 42.00000000000000000 ) ;
#32472 = PLANE ( 'NONE',  #44519 ) ;
#32473 = FACE_OUTER_BOUND ( 'NONE', #20959, .T. ) ;
#32474 = ORIENTED_EDGE ( 'NONE', *, *, #45236, .T. ) ;
#32475 = ORIENTED_EDGE ( 'NONE', *, *, #13480, .F. ) ;
#32476 = CARTESIAN_POINT ( 'NONE',  ( 10.00000000000000000, 46.53671651293948486, 59.03961581697416250 ) ) ;
#32477 = DIRECTION ( 'NONE',  ( -1.000000000000000000, 0.000000000000000000, -0.000000000000000000 ) ) ;
#32478 = DIRECTION ( 'NONE',  ( -0.3853207896976523772, 0.9227826878668550226, 0.000000000000000000 ) ) ;
#32479 = ADVANCED_FACE ( 'NONE', ( #33145 ), #22122, .T. ) ;
#32480 = VERTEX_POINT ( 'NONE', #32893 ) ;
#32481 = CIRCLE ( 'NONE', #24654, 77.49899999999999523 ) ;
#32482 = AXIS2_PLACEMENT_3D ( 'NONE', #47053, #13517, #2971 ) ;
#32483 = ORIENTED_EDGE ( 'NONE', *, *, #33533, .F. ) ;
#32484 = ORIENTED_EDGE ( 'NONE', *, *, #21163, .F. ) ;
#32485 = DIRECTION ( 'NONE',  ( 1.000000000000000000, 0.000000000000000000, 0.000000000000000000 ) ) ;
#32486 = ORIENTED_EDGE ( 'NONE', *, *, #42777, .T. ) ;
#32487 = DIRECTION ( 'NONE',  ( -1.000000000000000000, -0.000000000000000000, -0.000000000000000000 ) ) ;
#32488 = EDGE_CURVE ( 'NONE', #9223, #26325, #13765, .T. ) ;
#32489 = AXIS2_PLACEMENT_3D ( 'NONE', #8416, #19906, #4986 ) ;
#32490 = DIRECTION ( 'NONE',  ( 1.000000000000000000, 0.000000000000000000, -0.000000000000000000 ) ) ;
#32491 = CARTESIAN_POINT ( 'NONE',  ( 12.00000000000000000, 20.85821328998756385, 10.92862929874494249 ) ) ;
#32492 = FACE_OUTER_BOUND ( 'NONE', #8629, .T. ) ;
#32493 = EDGE_CURVE ( 'NONE', #43938, #21525, #45813, .T. ) ;
#32494 = AXIS2_PLACEMENT_3D ( 'NONE', #45865, #30940, #30677 ) ;
#32495 = CIRCLE ( 'NONE', #23084, 77.49899999999999523 ) ;
#32496 = FILL_AREA_STYLE ('',( #21470 ) ) ;
#32497 = CARTESIAN_POINT ( 'NONE',  ( 11.99999999999999822, 75.11725578898472122, -2.956366410619845730 ) ) ;
#32498 = ORIENTED_EDGE ( 'NONE', *, *, #21260, .F. ) ;
#32499 = DIRECTION ( 'NONE',  ( 1.000000000000000000, -0.000000000000000000, 0.000000000000000000 ) ) ;
#32500 = ORIENTED_EDGE ( 'NONE', *, *, #8189, .T. ) ;
#32501 = FACE_OUTER_BOUND ( 'NONE', #38849, .T. ) ;
#32502 = DIRECTION ( 'NONE',  ( -0.000000000000000000, 0.000000000000000000, 1.000000000000000000 ) ) ;
#32503 = AXIS2_PLACEMENT_3D ( 'NONE', #9749, #24687, #28606 ) ;
#32504 = CARTESIAN_POINT ( 'NONE',  ( 10.00000000000000000, 8.830959090343430518, -74.65491531819107252 ) ) ;
#32505 = CARTESIAN_POINT ( 'NONE',  ( 5.250000000000000000, -13.95926121303099343, -1.199999999999999956 ) ) ;
#32506 = EDGE_CURVE ( 'NONE', #7163, #43544, #7514, .T. ) ;
#32507 = CIRCLE ( 'NONE', #47354, 42.00000000000000000 ) ;
#32508 = EDGE_CURVE ( 'NONE', #2713, #4855, #44232, .T. ) ;
#32509 = EDGE_CURVE ( 'NONE', #30519, #17771, #35637, .T. ) ;
#32510 = CARTESIAN_POINT ( 'NONE',  ( 11.99999999999999822, -76.41127070299262414, -12.93880638057396304 ) ) ;
#32511 = LINE ( 'NONE', #39372, #11497 ) ;
#32512 = AXIS2_PLACEMENT_3D ( 'NONE', #29905, #48023, #40456 ) ;
#32513 = VERTEX_POINT ( 'NONE', #44405 ) ;
#32514 = CARTESIAN_POINT ( 'NONE',  ( 5.999999999999999112, -77.16300072079681627, 27.74655509720641433 ) ) ;
#32515 = CARTESIAN_POINT ( 'NONE',  ( 0.000000000000000000, 58.39081064771822582, -50.95692526931267707 ) ) ;
#32516 = CARTESIAN_POINT ( 'NONE',  ( 0.000000000000000000, 27.74655509720669500, 77.16300072079670258 ) ) ;
#32517 = VERTEX_POINT ( 'NONE', #10874 ) ;
#32518 = DIRECTION ( 'NONE',  ( -1.000000000000000000, -0.000000000000000000, -0.000000000000000000 ) ) ;
#32519 = EDGE_LOOP ( 'NONE', ( #34925, #31227, #24235, #22959 ) ) ;
#32520 = ORIENTED_EDGE ( 'NONE', *, *, #14863, .T. ) ;
#32521 = CIRCLE ( 'NONE', #30189, 31.99999999999998224 ) ;
#32522 = CARTESIAN_POINT ( 'NONE',  ( 10.00000000000000000, 23.16143007188426850, 73.95703589263983702 ) ) ;
#32523 = DIRECTION ( 'NONE',  ( 0.000000000000000000, 0.000000000000000000, 1.000000000000000000 ) ) ;
#32524 = ORIENTED_EDGE ( 'NONE', *, *, #12594, .F. ) ;
#32525 = AXIS2_PLACEMENT_3D ( 'NONE', #26315, #26787, #11396 ) ;
#32526 = CARTESIAN_POINT ( 'NONE',  ( 11.99999999999999822, 0.000000000000000000, 0.000000000000000000 ) ) ;
#32527 = VERTEX_POINT ( 'NONE', #26036 ) ;
#32528 = ORIENTED_EDGE ( 'NONE', *, *, #32184, .T. ) ;
#32529 = AXIS2_PLACEMENT_3D ( 'NONE', #14994, #30638, #12048 ) ;
#32530 = VERTEX_POINT ( 'NONE', #18919 ) ;
#32531 = CIRCLE ( 'NONE', #33339, 16.00000000000000355 ) ;
#32532 = AXIS2_PLACEMENT_3D ( 'NONE', #21287, #32783, #37193 ) ;
#32533 = DIRECTION ( 'NONE',  ( -1.000000000000000000, 0.000000000000000000, 0.000000000000000000 ) ) ;
#32534 = ADVANCED_FACE ( 'NONE', ( #40985 ), #7680, .T. ) ;
#32535 = ORIENTED_EDGE ( 'NONE', *, *, #45625, .F. ) ;
#32536 = CARTESIAN_POINT ( 'NONE',  ( 0.000000000000000000, 0.000000000000000000, 42.00000000000001421 ) ) ;
#32537 = ORIENTED_EDGE ( 'NONE', *, *, #24502, .F. ) ;
#32538 = FACE_OUTER_BOUND ( 'NONE', #20529, .T. ) ;
#32539 = EDGE_CURVE ( 'NONE', #46550, #20736, #41902, .T. ) ;
#32540 = PLANE ( 'NONE',  #12939 ) ;
#32541 = LINE ( 'NONE', #6357, #18934 ) ;
#32542 = EDGE_CURVE ( 'NONE', #29567, #22296, #4373, .T. ) ;
#32543 = EDGE_LOOP ( 'NONE', ( #22972, #38617, #4435, #7121 ) ) ;
#32544 = CARTESIAN_POINT ( 'NONE',  ( 5.000000000000002665, -80.28980883073747066, -16.65972982745018172 ) ) ;
#32545 = EDGE_LOOP ( 'NONE', ( #8023, #43623, #9743, #13142 ) ) ;
#32546 = DIRECTION ( 'NONE',  ( -1.000000000000000000, 0.000000000000000000, 0.000000000000000000 ) ) ;
#32547 = CARTESIAN_POINT ( 'NONE',  ( 10.00000000000000000, -15.48615015657610883, 39.04073710021339139 ) ) ;
#32548 = VECTOR ( 'NONE', #30801, 1000.000000000000000 ) ;
#32549 = ORIENTED_EDGE ( 'NONE', *, *, #40656, .F. ) ;
#32550 = ORIENTED_EDGE ( 'NONE', *, *, #34864, .T. ) ;
#32551 = DIRECTION ( 'NONE',  ( -1.000000000000000000, -0.000000000000000000, -0.000000000000000000 ) ) ;
#32552 = DIRECTION ( 'NONE',  ( 0.000000000000000000, -0.8660254037844363761, -0.5000000000000039968 ) ) ;
#32553 = ORIENTED_EDGE ( 'NONE', *, *, #10263, .F. ) ;
#32554 = VERTEX_POINT ( 'NONE', #27258 ) ;
#32555 = LINE ( 'NONE', #25669, #12077 ) ;
#32556 = CIRCLE ( 'NONE', #11467, 77.49900000000002365 ) ;
#32557 = DIRECTION ( 'NONE',  ( -1.000000000000000000, 0.000000000000000000, -0.000000000000000000 ) ) ;
#32558 = FACE_OUTER_BOUND ( 'NONE', #25121, .T. ) ;
#32559 = DIRECTION ( 'NONE',  ( 0.000000000000000000, 0.000000000000000000, -1.000000000000000000 ) ) ;
#32560 = ADVANCED_FACE ( 'NONE', ( #23332 ), #34329, .T. ) ;
#32561 = EDGE_CURVE ( 'NONE', #6408, #48250, #38767, .T. ) ;
#32562 = PLANE ( 'NONE',  #16936 ) ;
#32563 = ORIENTED_EDGE ( 'NONE', *, *, #15106, .T. ) ;
#32564 = LINE ( 'NONE', #47485, #22371 ) ;
#32565 = CARTESIAN_POINT ( 'NONE',  ( 0.000000000000000000, 21.60688246758586928, 79.10210256391376049 ) ) ;
#32566 = CARTESIAN_POINT ( 'NONE',  ( 11.99999999999999822, -75.11764819372149304, 2.946379043146075905 ) ) ;
#32567 = LINE ( 'NONE', #13958, #48022 ) ;
#32568 = SURFACE_SIDE_STYLE ('',( #35517 ) ) ;
#32569 = AXIS2_PLACEMENT_3D ( 'NONE', #46413, #19977, #27829 ) ;
#32570 = DIRECTION ( 'NONE',  ( -1.000000000000000000, -0.000000000000000000, -0.000000000000000000 ) ) ;
#32571 = ADVANCED_FACE ( 'NONE', ( #581 ), #8630, .T. ) ;
#32572 = VECTOR ( 'NONE', #47655, 1000.000000000000000 ) ;
#32573 = CARTESIAN_POINT ( 'NONE',  ( 0.000000000000000000, -39.78640506895559525, -66.50666863322042843 ) ) ;
#32574 = CARTESIAN_POINT ( 'NONE',  ( 10.00000000000000000, 67.80270845531956070, -46.11716303203112943 ) ) ;
#32575 = VERTEX_POINT ( 'NONE', #42419 ) ;
#32576 = CIRCLE ( 'NONE', #22416, 16.00000000000000000 ) ;
#32577 = APPLICATION_CONTEXT ( 'automotive_design' ) ;
#32578 = DIRECTION ( 'NONE',  ( 0.000000000000000000, 0.000000000000000000, 1.000000000000000000 ) ) ;
#32579 = DIRECTION ( 'NONE',  ( 1.000000000000000000, -0.000000000000000000, -0.000000000000000000 ) ) ;
#32580 = CIRCLE ( 'NONE', #15410, 31.99999999999998579 ) ;
#32581 = VERTEX_POINT ( 'NONE', #27021 ) ;
#32582 = ORIENTED_EDGE ( 'NONE', *, *, #25627, .F. ) ;
#32583 = CARTESIAN_POINT ( 'NONE',  ( 15.00000000000000000, -3.948201729842355068, -23.21447184625292692 ) ) ;
#32584 = CARTESIAN_POINT ( 'NONE',  ( 10.00000000000000000, 70.53064760720316428, -26.01480285779861035 ) ) ;
#32585 = DIRECTION ( 'NONE',  ( -1.000000000000000000, -0.000000000000000000, -0.000000000000000000 ) ) ;
#32586 = ORIENTED_EDGE ( 'NONE', *, *, #21558, .T. ) ;
#32587 = ADVANCED_FACE ( 'NONE', ( #23096 ), #4500, .T. ) ;
#32588 = CARTESIAN_POINT ( 'NONE',  ( 11.99999999999999822, 0.000000000000000000, 0.000000000000000000 ) ) ;
#32589 = ORIENTED_EDGE ( 'NONE', *, *, #47155, .T. ) ;
#32590 = AXIS2_PLACEMENT_3D ( 'NONE', #5532, #13126, #20454 ) ;
#32591 = LINE ( 'NONE', #21581, #36862 ) ;
#32592 = EDGE_CURVE ( 'NONE', #26338, #11209, #17628, .T. ) ;
#32593 = DIRECTION ( 'NONE',  ( 0.000000000000000000, -0.9135454576426056406, 0.4067366430757897722 ) ) ;
#32594 = PLANE ( 'NONE',  #34093 ) ;
#32595 = VECTOR ( 'NONE', #6498, 1000.000000000000114 ) ;
#32597 = VERTEX_POINT ( 'NONE', #38506 ) ;
#32596 = CARTESIAN_POINT ( 'NONE',  ( -7.893099573151324044, -11.68370571044642503, -1.199999999999999956 ) ) ;
#32598 = CARTESIAN_POINT ( 'NONE',  ( -10.00000000000000000, 0.000000000000000000, 0.000000000000000000 ) ) ;
#32599 = EDGE_LOOP ( 'NONE', ( #14533, #9218, #4273, #45821 ) ) ;
#32600 = DIRECTION ( 'NONE',  ( 0.000000000000000000, 0.000000000000000000, 1.000000000000000000 ) ) ;
#32601 = ORIENTED_EDGE ( 'NONE', *, *, #37761, .F. ) ;
#32602 = EDGE_LOOP ( 'NONE', ( #12, #26207, #10929, #5165 ) ) ;
#32603 = EDGE_CURVE ( 'NONE', #33968, #22554, #48136, .T. ) ;
#32604 = CARTESIAN_POINT ( 'NONE',  ( 10.00000000000000000, 18.89407956138256139, 75.16055320797038064 ) ) ;
#32605 = DIRECTION ( 'NONE',  ( 0.000000000000000000, 0.000000000000000000, 1.000000000000000000 ) ) ;
#32606 = CARTESIAN_POINT ( 'NONE',  ( 10.00000000000000000, 79.10210256391397365, -21.60688246758502373 ) ) ;
#32607 = CARTESIAN_POINT ( 'NONE',  ( 0.000000000000000000, 51.29473840253223926, 63.97538442413444670 ) ) ;
#32608 = DIRECTION ( 'NONE',  ( -1.000000000000000000, -0.000000000000000000, -0.000000000000000000 ) ) ;
#32609 = ORIENTED_EDGE ( 'NONE', *, *, #21916, .F. ) ;
#32610 = LINE ( 'NONE', #21098, #27697 ) ;
#32611 = LINE ( 'NONE', #47536, #18697 ) ;
#32612 = AXIS2_PLACEMENT_3D ( 'NONE', #29249, #21413, #32671 ) ;
#32613 = LINE ( 'NONE', #32838, #29803 ) ;
#32614 = EDGE_CURVE ( 'NONE', #29381, #45887, #25448, .T. ) ;
#32615 = FACE_OUTER_BOUND ( 'NONE', #40383, .T. ) ;
#32616 = AXIS2_PLACEMENT_3D ( 'NONE', #802, #23092, #7677 ) ;
#32617 = ORIENTED_EDGE ( 'NONE', *, *, #4919, .F. ) ;
#32618 = DIRECTION ( 'NONE',  ( -1.000000000000000000, -0.000000000000000000, -0.000000000000000000 ) ) ;
#32619 = EDGE_CURVE ( 'NONE', #8511, #39399, #5947, .T. ) ;
#32620 = DIRECTION ( 'NONE',  ( -1.000000000000000000, 0.000000000000000000, -0.000000000000000000 ) ) ;
#32621 = DIRECTION ( 'NONE',  ( -1.000000000000000000, 0.000000000000000000, 0.000000000000000000 ) ) ;
#32622 = AXIS2_PLACEMENT_3D ( 'NONE', #22209, #18285, #7028 ) ;
#32623 = DIRECTION ( 'NONE',  ( -1.000000000000000000, 0.000000000000000000, 0.000000000000000000 ) ) ;
#32624 = CARTESIAN_POINT ( 'NONE',  ( 10.00000000000000000, 36.88895765772633695, 6.736453364083687667 ) ) ;
#32625 = ORIENTED_EDGE ( 'NONE', *, *, #22763, .F. ) ;
#32626 = ADVANCED_FACE ( 'NONE', ( #31425 ), #46332, .T. ) ;
#32627 = ORIENTED_EDGE ( 'NONE', *, *, #14550, .T. ) ;
#32628 = CYLINDRICAL_SURFACE ( 'NONE', #45682, 31.99999999999998579 ) ;
#32629 = VECTOR ( 'NONE', #16319, 1000.000000000000000 ) ;
#32630 = EDGE_LOOP ( 'NONE', ( #40539, #8428, #46019, #13209 ) ) ;
#32631 = CARTESIAN_POINT ( 'NONE',  ( 10.00000000000000000, 0.000000000000000000, 0.000000000000000000 ) ) ;
#32632 = FACE_OUTER_BOUND ( 'NONE', #43230, .T. ) ;
#32633 = EDGE_LOOP ( 'NONE', ( #31898, #24684, #13814, #45112 ) ) ;
#32634 = EDGE_CURVE ( 'NONE', #44307, #45913, #5231, .T. ) ;
#32635 = LINE ( 'NONE', #24580, #25382 ) ;
#32636 = ORIENTED_EDGE ( 'NONE', *, *, #25228, .T. ) ;
#32637 = VECTOR ( 'NONE', #9359, 1000.000000000000000 ) ;
#32638 = DIRECTION ( 'NONE',  ( 0.000000000000000000, 0.000000000000000000, -1.000000000000000000 ) ) ;
#32639 = EDGE_CURVE ( 'NONE', #20444, #32581, #23898, .T. ) ;
#32640 = DIRECTION ( 'NONE',  ( 0.000000000000000000, 0.000000000000000000, 1.000000000000000000 ) ) ;
#32641 = FACE_OUTER_BOUND ( 'NONE', #28509, .T. ) ;
#32642 = ORIENTED_EDGE ( 'NONE', *, *, #32509, .F. ) ;
#32644 = EDGE_CURVE ( 'NONE', #19539, #26327, #1049, .T. ) ;
#32643 = AXIS2_PLACEMENT_3D ( 'NONE', #16801, #35141, #1624 ) ;
#32645 = CARTESIAN_POINT ( 'NONE',  ( 10.00000000000000000, 46.54456581323805153, 59.03342792756280488 ) ) ;
#32646 = ORIENTED_EDGE ( 'NONE', *, *, #4342, .T. ) ;
#32647 = EDGE_CURVE ( 'NONE', #44807, #28358, #37779, .T. ) ;
#32648 = FACE_OUTER_BOUND ( 'NONE', #35848, .T. ) ;
#32649 = PLANE ( 'NONE',  #30424 ) ;
#32650 = DIRECTION ( 'NONE',  ( -0.1276937514489679404, -0.9918136447140103451, 0.000000000000000000 ) ) ;
#32651 = VERTEX_POINT ( 'NONE', #1312 ) ;
#32652 = ADVANCED_FACE ( 'NONE', ( #31178 ), #46098, .F. ) ;
#32653 = DIRECTION ( 'NONE',  ( -1.000000000000000000, -0.000000000000000000, -0.000000000000000000 ) ) ;
#32654 = VERTEX_POINT ( 'NONE', #31670 ) ;
#32655 = ORIENTED_EDGE ( 'NONE', *, *, #22465, .T. ) ;
#32656 = EDGE_CURVE ( 'NONE', #8515, #1874, #24543, .T. ) ;
#32657 = DIRECTION ( 'NONE',  ( -1.000000000000000000, 0.000000000000000000, 0.000000000000000000 ) ) ;
#32658 = CARTESIAN_POINT ( 'NONE',  ( 10.00000000000000000, 37.01155633439059756, 6.555932627142549762 ) ) ;
#32659 = FACE_OUTER_BOUND ( 'NONE', #26689, .T. ) ;
#32660 = DIRECTION ( 'NONE',  ( -1.000000000000000000, -0.000000000000000000, -0.000000000000000000 ) ) ;
#32661 = ORIENTED_EDGE ( 'NONE', *, *, #27119, .F. ) ;
#32662 = DIRECTION ( 'NONE',  ( -1.000000000000000000, -0.000000000000000000, -0.000000000000000000 ) ) ;
#32663 = CARTESIAN_POINT ( 'NONE',  ( 10.00000000000000000, -33.17418723428319538, 17.67226234102814431 ) ) ;
#32664 = DIRECTION ( 'NONE',  ( -1.000000000000000000, 0.000000000000000000, -0.000000000000000000 ) ) ;
#32665 = CARTESIAN_POINT ( 'NONE',  ( 5.250000000000000000, -13.95926121303099343, -1.199999999999999956 ) ) ;
#32666 = VECTOR ( 'NONE', #26435, 1000.000000000000000 ) ;
#32667 = PLANE ( 'NONE',  #7972 ) ;
#32668 = CARTESIAN_POINT ( 'NONE',  ( 10.00000000000000000, -59.03961581697432592, 46.53671651293927880 ) ) ;
#32669 = ORIENTED_EDGE ( 'NONE', *, *, #37699, .F. ) ;
#32670 = VERTEX_POINT ( 'NONE', #31910 ) ;
#32671 = DIRECTION ( 'NONE',  ( 0.000000000000000000, 0.000000000000000000, 1.000000000000000000 ) ) ;
#32672 = CARTESIAN_POINT ( 'NONE',  ( -2.977765906491215642, 15.77977592589476608, 0.000000000000000000 ) ) ;
#32673 = FACE_OUTER_BOUND ( 'NONE', #1859, .T. ) ;
#32674 = FACE_OUTER_BOUND ( 'NONE', #37174, .T. ) ;
#32675 = CIRCLE ( 'NONE', #48291, 31.99999999999999289 ) ;
#32676 = ADVANCED_FACE ( 'NONE', ( #39960 ), #43148, .T. ) ;
#32677 = CARTESIAN_POINT ( 'NONE',  ( -19.27444613274700913, -101.8135840178490668, -2.500000000000000000 ) ) ;
#32678 = CARTESIAN_POINT ( 'NONE',  ( 12.00000000000000000, -1.278221433540507768, -26.51162292216071492 ) ) ;
#32679 = ORIENTED_EDGE ( 'NONE', *, *, #41673, .F. ) ;
#32680 = CYLINDRICAL_SURFACE ( 'NONE', #38721, 12.49999999999999645 ) ;
#32681 = VECTOR ( 'NONE', #5913, 999.9999999999998863 ) ;
#32682 = EDGE_CURVE ( 'NONE', #4718, #28097, #35796, .T. ) ;
#32683 = VECTOR ( 'NONE', #5816, 1000.000000000000000 ) ;
#32684 = CARTESIAN_POINT ( 'NONE',  ( 10.00000000000000000, 60.67117009219136037, 55.16347631943062879 ) ) ;
#32685 = EDGE_LOOP ( 'NONE', ( #6772, #40413, #31395, #26948 ) ) ;
#32686 = ORIENTED_EDGE ( 'NONE', *, *, #4429, .F. ) ;
#32687 = ADVANCED_FACE ( 'NONE', ( #20621 ), #28704, .T. ) ;
#32688 = EDGE_LOOP ( 'NONE', ( #46711, #39200, #14724, #14558 ) ) ;
#32689 = CARTESIAN_POINT ( 'NONE',  ( 10.00000000000000000, 77.16300072079661732, 27.74655509720697921 ) ) ;
#32690 = PRODUCT_DEFINITION_FORMATION_WITH_SPECIFIED_SOURCE ( 'ANY', '', #6195, .NOT_KNOWN. ) ;
#32691 = VERTEX_POINT ( 'NONE', #5457 ) ;
#32692 = AXIS2_PLACEMENT_3D ( 'NONE', #27552, #1369, #45667 ) ;
#32693 = ORIENTED_EDGE ( 'NONE', *, *, #40511, .T. ) ;
#32694 = CARTESIAN_POINT ( 'NONE',  ( 15.00000000000000000, -4.261787119644963262, 26.19803753235780164 ) ) ;
#32695 = EDGE_CURVE ( 'NONE', #39278, #34677, #25010, .T. ) ;
#32696 = CARTESIAN_POINT ( 'NONE',  ( -10.00000000000000000, 0.000000000000000000, 0.000000000000000000 ) ) ;
#32697 = DIRECTION ( 'NONE',  ( -1.000000000000000000, 0.000000000000000000, 0.000000000000000000 ) ) ;
#32698 = ORIENTED_EDGE ( 'NONE', *, *, #27583, .F. ) ;
#32699 = DIRECTION ( 'NONE',  ( 0.000000000000000000, 0.000000000000000000, 1.000000000000000000 ) ) ;
#32700 = ORIENTED_EDGE ( 'NONE', *, *, #24660, .F. ) ;
#32701 = EDGE_CURVE ( 'NONE', #25362, #45891, #443, .T. ) ;
#32702 = ORIENTED_EDGE ( 'NONE', *, *, #9445, .F. ) ;
#32703 = VERTEX_POINT ( 'NONE', #17419 ) ;
#32704 = LINE ( 'NONE', #39827, #45981 ) ;
#32705 = CARTESIAN_POINT ( 'NONE',  ( 0.000000000000000000, 1.530808498934191521E-15, -12.50000000000000000 ) ) ;
#32706 = CARTESIAN_POINT ( 'NONE',  ( 0.000000000000000000, 0.000000000000000000, 0.000000000000000000 ) ) ;
#32707 = ORIENTED_EDGE ( 'NONE', *, *, #17886, .F. ) ;
#32708 = ORIENTED_EDGE ( 'NONE', *, *, #43988, .T. ) ;
#32709 = DIRECTION ( 'NONE',  ( 0.000000000000000000, 0.000000000000000000, -1.000000000000000000 ) ) ;
#32710 = EDGE_LOOP ( 'NONE', ( #7550, #26712, #36186, #37243 ) ) ;
#32711 = ADVANCED_FACE ( 'NONE', ( #21092 ), #20876, .T. ) ;
#32712 = CARTESIAN_POINT ( 'NONE',  ( 0.000000000000000000, 76.69515212746016175, 29.01471420065590578 ) ) ;
#32713 = VECTOR ( 'NONE', #24696, 1000.000000000000000 ) ;
#32714 = CARTESIAN_POINT ( 'NONE',  ( 11.99999999999999822, 20.41045688087824317, 72.35160999960824313 ) ) ;
#32715 = EDGE_CURVE ( 'NONE', #39388, #24628, #12972, .T. ) ;
#32717 = DIRECTION ( 'NONE',  ( -1.000000000000000000, -0.000000000000000000, 0.000000000000000000 ) ) ;
#32716 = VECTOR ( 'NONE', #27889, 1000.000000000000114 ) ;
#32718 = EDGE_LOOP ( 'NONE', ( #27361, #43960, #33327, #30152 ) ) ;
#32719 = DIRECTION ( 'NONE',  ( 0.000000000000000000, 0.9969173337331276308, 0.07845909572784874608 ) ) ;
#32720 = DIRECTION ( 'NONE',  ( 0.000000000000000000, -0.9510565162951565288, 0.3090169943749382364 ) ) ;
#32721 = VECTOR ( 'NONE', #2789, 1000.000000000000114 ) ;
#32722 = CARTESIAN_POINT ( 'NONE',  ( -19.90058851926621131, -132.5883508287165853, 5.500000000000000000 ) ) ;
#32723 = PLANE ( 'NONE',  #47662 ) ;
#32724 = CARTESIAN_POINT ( 'NONE',  ( 0.000000000000000000, 0.000000000000000000, 0.000000000000000000 ) ) ;
#32725 = VERTEX_POINT ( 'NONE', #1787 ) ;
#32726 = CARTESIAN_POINT ( 'NONE',  ( 11.99999999999999822, 73.72996012237440766, 14.67089635893739619 ) ) ;
#32727 = DIRECTION ( 'NONE',  ( -1.000000000000000000, 0.000000000000000000, 0.000000000000000000 ) ) ;
#32728 = LINE ( 'NONE', #17803, #28273 ) ;
#32729 = FACE_OUTER_BOUND ( 'NONE', #37813, .T. ) ;
#32730 = DIRECTION ( 'NONE',  ( 1.000000000000000000, 0.000000000000000000, 0.000000000000000000 ) ) ;
#32731 = AXIS2_PLACEMENT_3D ( 'NONE', #28169, #24748, #6386 ) ;
#32732 = FACE_OUTER_BOUND ( 'NONE', #35998, .T. ) ;
#32733 = LINE ( 'NONE', #9984, #39616 ) ;
#32734 = CARTESIAN_POINT ( 'NONE',  ( -3.000000000000000000, -18.13022148937243472, -15.02647892043568767 ) ) ;
#32735 = DIRECTION ( 'NONE',  ( -1.000000000000000000, -0.000000000000000000, 0.000000000000000000 ) ) ;
#32736 = DIRECTION ( 'NONE',  ( 1.000000000000000000, -0.000000000000000000, -0.000000000000000000 ) ) ;
#32737 = ORIENTED_EDGE ( 'NONE', *, *, #37861, .T. ) ;
#32738 = ORIENTED_EDGE ( 'NONE', *, *, #38689, .F. ) ;
#32739 = EDGE_LOOP ( 'NONE', ( #43132, #4552, #694, #38813 ) ) ;
#32740 = AXIS2_PLACEMENT_3D ( 'NONE', #3123, #10485, #36434 ) ;
#32741 = ADVANCED_FACE ( 'NONE', ( #27988 ), #17672, .T. ) ;
#32742 = AXIS2_PLACEMENT_3D ( 'NONE', #33950, #11468, #19266 ) ;
#32743 = CIRCLE ( 'NONE', #11658, 31.99999999999999645 ) ;
#32744 = CYLINDRICAL_SURFACE ( 'NONE', #9271, 42.00000000000000000 ) ;
#32745 = CARTESIAN_POINT ( 'NONE',  ( -8.826826895187510402, -94.96827758698185562, -5.500000000000000000 ) ) ;
#32746 = AXIS2_PLACEMENT_3D ( 'NONE', #11365, #795, #29467 ) ;
#32747 = VERTEX_POINT ( 'NONE', #21339 ) ;
#32748 = CYLINDRICAL_SURFACE ( 'NONE', #6215, 77.49899999999999523 ) ;
#32749 = VERTEX_POINT ( 'NONE', #38997 ) ;
#32750 = EDGE_LOOP ( 'NONE', ( #43329, #23872, #37228, #3449 ) ) ;
#32751 = EDGE_CURVE ( 'NONE', #40605, #43691, #30971, .T. ) ;
#32752 = EDGE_CURVE ( 'NONE', #28743, #38129, #41131, .T. ) ;
#32753 = EDGE_CURVE ( 'NONE', #23167, #19565, #9851, .T. ) ;
#32754 = FACE_OUTER_BOUND ( 'NONE', #42701, .T. ) ;
#32755 = ORIENTED_EDGE ( 'NONE', *, *, #27705, .T. ) ;
#32756 = CARTESIAN_POINT ( 'NONE',  ( 10.00000000000000000, 0.000000000000000000, 0.000000000000000000 ) ) ;
#32757 = ORIENTED_EDGE ( 'NONE', *, *, #9703, .F. ) ;
#32758 = EDGE_CURVE ( 'NONE', #22722, #4498, #26240, .T. ) ;
#32759 = DIRECTION ( 'NONE',  ( 0.000000000000000000, 0.000000000000000000, 1.000000000000000000 ) ) ;
#32760 = EDGE_CURVE ( 'NONE', #44059, #29462, #9594, .T. ) ;
#32761 = LINE ( 'NONE', #36675, #417 ) ;
#32762 = CARTESIAN_POINT ( 'NONE',  ( 5.000000000000002665, -81.96053171279903893, 2.543863470248101333 ) ) ;
#32763 = ORIENTED_EDGE ( 'NONE', *, *, #25130, .T. ) ;
#32764 = ORIENTED_EDGE ( 'NONE', *, *, #28082, .T. ) ;
#32765 = CARTESIAN_POINT ( 'NONE',  ( 11.99999999999999822, -75.11725578898466438, -2.956366410621452001 ) ) ;
#32766 = CIRCLE ( 'NONE', #29630, 82.00000000000000000 ) ;
#32767 = CARTESIAN_POINT ( 'NONE',  ( 10.00000000000000000, -55.19960302592029677, -51.03279382321147750 ) ) ;
#32768 = ORIENTED_EDGE ( 'NONE', *, *, #47188, .T. ) ;
#32769 = AXIS2_PLACEMENT_3D ( 'NONE', #3069, #29517, #36606 ) ;
#32770 = EDGE_LOOP ( 'NONE', ( #3187, #1231, #5453, #33328 ) ) ;
#32771 = CARTESIAN_POINT ( 'NONE',  ( 10.00000000000000000, 0.000000000000000000, 37.49900000000000233 ) ) ;
#32772 = CARTESIAN_POINT ( 'NONE',  ( 0.000000000000000000, 74.18225833017937987, -34.94270380257559339 ) ) ;
#32773 = VERTEX_POINT ( 'NONE', #6186 ) ;
#32774 = ORIENTED_EDGE ( 'NONE', *, *, #25734, .F. ) ;
#32775 = AXIS2_PLACEMENT_3D ( 'NONE', #39209, #843, #20348 ) ;
#32777 = EDGE_CURVE ( 'NONE', #15686, #34754, #15349, .T. ) ;
#32776 = DIRECTION ( 'NONE',  ( -0.6516173805718067369, 0.7585478161175716050, 0.000000000000000000 ) ) ;
#32778 = FACE_OUTER_BOUND ( 'NONE', #16639, .T. ) ;
#32779 = DIRECTION ( 'NONE',  ( 0.000000000000000000, 0.000000000000000000, 1.000000000000000000 ) ) ;
#32780 = DIRECTION ( 'NONE',  ( -1.000000000000000000, -0.000000000000000000, 0.000000000000000000 ) ) ;
#32781 = CARTESIAN_POINT ( 'NONE',  ( 11.99999999999999822, -67.80270845531921964, 46.11716303203162681 ) ) ;
#32782 = EDGE_LOOP ( 'NONE', ( #45572, #19574, #25869, #34744 ) ) ;
#32783 = DIRECTION ( 'NONE',  ( -1.000000000000000000, -0.000000000000000000, -0.000000000000000000 ) ) ;
#32784 = AXIS2_PLACEMENT_3D ( 'NONE', #18681, #36800, #37530 ) ;
#32785 = FACE_OUTER_BOUND ( 'NONE', #42042, .T. ) ;
#32786 = DIRECTION ( 'NONE',  ( 0.9227826878668540234, 0.3853207896976547087, 0.000000000000000000 ) ) ;
#32787 = DIRECTION ( 'NONE',  ( 0.000000000000000000, 0.000000000000000000, 1.000000000000000000 ) ) ;
#32788 = CYLINDRICAL_SURFACE ( 'NONE', #2933, 42.00000000000000000 ) ;
#32789 = ORIENTED_EDGE ( 'NONE', *, *, #6311, .T. ) ;
#32790 = ORIENTED_EDGE ( 'NONE', *, *, #44960, .F. ) ;
#32791 = EDGE_LOOP ( 'NONE', ( #45588, #14761, #35967, #28020 ) ) ;
#32792 = ORIENTED_EDGE ( 'NONE', *, *, #9770, .T. ) ;
#32793 = EDGE_CURVE ( 'NONE', #30536, #24231, #47529, .T. ) ;
#32794 = PLANE ( 'NONE',  #39347 ) ;
#32795 = ADVANCED_FACE ( 'NONE', ( #36513 ), #268, .T. ) ;
#32796 = DIRECTION ( 'NONE',  ( -1.000000000000000000, 0.000000000000000000, -0.000000000000000000 ) ) ;
#32797 = EDGE_CURVE ( 'NONE', #40433, #2363, #2818, .T. ) ;
#32798 = VERTEX_POINT ( 'NONE', #21596 ) ;
#32799 = AXIS2_PLACEMENT_3D ( 'NONE', #45491, #11977, #26908 ) ;
#32800 = AXIS2_PLACEMENT_3D ( 'NONE', #35836, #2301, #17218 ) ;
#32801 = CARTESIAN_POINT ( 'NONE',  ( 0.000000000000000000, 0.000000000000000000, 0.000000000000000000 ) ) ;
#32802 = ORIENTED_EDGE ( 'NONE', *, *, #4762, .F. ) ;
#32803 = CARTESIAN_POINT ( 'NONE',  ( 10.00000000000000000, -41.76106447765443619, -62.50884508063471401 ) ) ;
#32804 = AXIS2_PLACEMENT_3D ( 'NONE', #26936, #38185, #19798 ) ;
#32805 = ORIENTED_EDGE ( 'NONE', *, *, #37402, .F. ) ;
#32806 = AXIS2_PLACEMENT_3D ( 'NONE', #47174, #47885, #40558 ) ;
#32807 = EDGE_CURVE ( 'NONE', #35473, #40588, #21821, .T. ) ;
#32808 = EDGE_CURVE ( 'NONE', #10070, #39605, #6668, .T. ) ;
#32809 = DIRECTION ( 'NONE',  ( -1.000000000000000000, -0.000000000000000000, 0.000000000000000000 ) ) ;
#32810 = ORIENTED_EDGE ( 'NONE', *, *, #4775, .F. ) ;
#32811 = CIRCLE ( 'NONE', #20310, 12.50000000000000000 ) ;
#32812 = LINE ( 'NONE', #2956, #47678 ) ;
#32813 = ORIENTED_EDGE ( 'NONE', *, *, #28792, .F. ) ;
#32814 = DIRECTION ( 'NONE',  ( 1.000000000000000000, 0.000000000000000000, 0.000000000000000000 ) ) ;
#32815 = ORIENTED_EDGE ( 'NONE', *, *, #45259, .T. ) ;
#32816 = DIRECTION ( 'NONE',  ( 0.000000000000000000, 0.000000000000000000, 1.000000000000000000 ) ) ;
#32817 = ORIENTED_EDGE ( 'NONE', *, *, #39654, .T. ) ;
#32818 = CARTESIAN_POINT ( 'NONE',  ( 0.000000000000000000, 23.50000000000000000, 1.499999999999997780 ) ) ;
#32819 = ORIENTED_EDGE ( 'NONE', *, *, #6299, .F. ) ;
#32820 = CARTESIAN_POINT ( 'NONE',  ( 10.00000000000000000, 0.000000000000000000, 0.000000000000000000 ) ) ;
#32821 = CARTESIAN_POINT ( 'NONE',  ( 0.000000000000000000, -120.0000000000000000, -2.500000000000000000 ) ) ;
#32822 = EDGE_CURVE ( 'NONE', #34540, #32940, #36325, .T. ) ;
#32824 = ORIENTED_EDGE ( 'NONE', *, *, #40304, .T. ) ;
#32823 = DIRECTION ( 'NONE',  ( -0.000000000000000000, -0.000000000000000000, -1.000000000000000000 ) ) ;
#32825 = DIRECTION ( 'NONE',  ( 0.000000000000000000, 0.000000000000000000, 1.000000000000000000 ) ) ;
#32826 = ORIENTED_EDGE ( 'NONE', *, *, #36080, .T. ) ;
#32827 = CYLINDRICAL_SURFACE ( 'NONE', #47494, 31.99999999999998579 ) ;
#32828 = ORIENTED_EDGE ( 'NONE', *, *, #32682, .T. ) ;
#32829 = ORIENTED_EDGE ( 'NONE', *, *, #13169, .T. ) ;
#32830 = FACE_OUTER_BOUND ( 'NONE', #9256, .T. ) ;
#32831 = DIRECTION ( 'NONE',  ( -1.000000000000000000, 0.000000000000000000, -0.000000000000000000 ) ) ;
#32832 = ORIENTED_EDGE ( 'NONE', *, *, #15862, .T. ) ;
#32833 = CARTESIAN_POINT ( 'NONE',  ( 10.00000000000000000, -26.01480285779785362, -70.53064760720343429 ) ) ;
#32834 = CARTESIAN_POINT ( 'NONE',  ( 6.000000000000000000, -34.94270380257692921, 74.18225833017875459 ) ) ;
#32835 = DIRECTION ( 'NONE',  ( 0.000000000000000000, 0.9969173337331281859, -0.07845909572784168229 ) ) ;
#32836 = VERTEX_POINT ( 'NONE', #14974 ) ;
#32837 = CARTESIAN_POINT ( 'NONE',  ( 10.00000000000000000, 37.22597642581158084, 10.79786254984347593 ) ) ;
#32838 = CARTESIAN_POINT ( 'NONE',  ( 12.00000000000000000, -3.948201729842032215, 23.21447184625297666 ) ) ;
#32840 = AXIS2_PLACEMENT_3D ( 'NONE', #21690, #47862, #32699 ) ;
#32839 = DIRECTION ( 'NONE',  ( 0.000000000000000000, 0.000000000000000000, 1.000000000000000000 ) ) ;
#32841 = VECTOR ( 'NONE', #46804, 1000.000000000000000 ) ;
#32842 = LINE ( 'NONE', #28933, #19947 ) ;
#32843 = CARTESIAN_POINT ( 'NONE',  ( 10.00000000000000178, 0.000000000000000000, 0.000000000000000000 ) ) ;
#32844 = CARTESIAN_POINT ( 'NONE',  ( 0.000000000000000000, -68.26794271651239399, -31.47745569255214093 ) ) ;
#32845 = CYLINDRICAL_SURFACE ( 'NONE', #15360, 77.49899999999999523 ) ;
#32846 = VECTOR ( 'NONE', #29955, 1000.000000000000000 ) ;
#32847 = AXIS2_PLACEMENT_3D ( 'NONE', #26944, #8327, #40900 ) ;
#32848 = CARTESIAN_POINT ( 'NONE',  ( 0.000000000000000000, 55.20638768913831029, -51.02545421589267960 ) ) ;
#32849 = CARTESIAN_POINT ( 'NONE',  ( 0.000000000000000000, 0.000000000000000000, 0.000000000000000000 ) ) ;
#32850 = CARTESIAN_POINT ( 'NONE',  ( 11.99999999999999822, 68.26794271651262136, 31.47745569255165066 ) ) ;
#32851 = CARTESIAN_POINT ( 'NONE',  ( 5.999999999999999112, -50.23322058963393744, 64.81221759200325039 ) ) ;
#32852 = AXIS2_PLACEMENT_3D ( 'NONE', #43463, #9668, #21407 ) ;
#32853 = VERTEX_POINT ( 'NONE', #33567 ) ;
#32854 = EDGE_CURVE ( 'NONE', #38423, #842, #41822, .T. ) ;
#32855 = ORIENTED_EDGE ( 'NONE', *, *, #3967, .F. ) ;
#32856 = ADVANCED_FACE ( 'NONE', ( #44827 ), #44103, .T. ) ;
#32857 = DIRECTION ( 'NONE',  ( 0.000000000000000000, 0.000000000000000000, 1.000000000000000000 ) ) ;
#32858 = CIRCLE ( 'NONE', #16448, 77.49899999999999523 ) ;
#32859 = ORIENTED_EDGE ( 'NONE', *, *, #44100, .F. ) ;
#32860 = CARTESIAN_POINT ( 'NONE',  ( 5.000000000000000000, 31.52238457039599595, 27.75498641678753842 ) ) ;
#32861 = EDGE_CURVE ( 'NONE', #30212, #16459, #18136, .T. ) ;
#32862 = DIRECTION ( 'NONE',  ( -1.000000000000000000, 0.000000000000000000, 0.000000000000000000 ) ) ;
#32863 = EDGE_CURVE ( 'NONE', #4472, #45870, #2978, .T. ) ;
#32864 = VERTEX_POINT ( 'NONE', #25975 ) ;
#32865 = CARTESIAN_POINT ( 'NONE',  ( 11.99999999999999822, 72.35160999960817207, 20.41045688087850607 ) ) ;
#32866 = ORIENTED_EDGE ( 'NONE', *, *, #10310, .T. ) ;
#32867 = ORIENTED_EDGE ( 'NONE', *, *, #45483, .F. ) ;
#32868 = EDGE_CURVE ( 'NONE', #9900, #22230, #33078, .T. ) ;
#32869 = ADVANCED_FACE ( 'NONE', ( #48259 ), #29894, .F. ) ;
#32870 = AXIS2_PLACEMENT_3D ( 'NONE', #22616, #18210, #92 ) ;
#32871 = CARTESIAN_POINT ( 'NONE',  ( 10.00000000000000000, -5.202137450156655518, 37.22597642581156663 ) ) ;
#32872 = ORIENTED_EDGE ( 'NONE', *, *, #44203, .F. ) ;
#32873 = AXIS2_PLACEMENT_3D ( 'NONE', #3873, #4120, #1166 ) ;
#32874 = EDGE_CURVE ( 'NONE', #46628, #40605, #29312, .T. ) ;
#32875 = FACE_OUTER_BOUND ( 'NONE', #27727, .T. ) ;
#32876 = FACE_OUTER_BOUND ( 'NONE', #23349, .T. ) ;
#32877 = AXIS2_PLACEMENT_3D ( 'NONE', #48011, #36517, #14502 ) ;
#32878 = AXIS2_PLACEMENT_3D ( 'NONE', #33723, #41097, #41331 ) ;
#32879 = ORIENTED_EDGE ( 'NONE', *, *, #15832, .T. ) ;
#32880 = CARTESIAN_POINT ( 'NONE',  ( 0.000000000000000000, 37.58145647212455032, -0.6853352020786441789 ) ) ;
#32881 = ORIENTED_EDGE ( 'NONE', *, *, #12291, .F. ) ;
#32882 = CIRCLE ( 'NONE', #21954, 37.49900000000000233 ) ;
#32883 = CARTESIAN_POINT ( 'NONE',  ( 10.00000000000000000, -74.65491531819111515, -8.830959090343204920 ) ) ;
#32884 = DIRECTION ( 'NONE',  ( 0.000000000000000000, -0.8090169943749503378, -0.5877852522924690293 ) ) ;
#32885 = CIRCLE ( 'NONE', #28220, 16.00000000000000000 ) ;
#32886 = CARTESIAN_POINT ( 'NONE',  ( 10.00000000000000000, 17.28742895386191236, -75.54627589209927407 ) ) ;
#32887 = EDGE_CURVE ( 'NONE', #18371, #7999, #11330, .T. ) ;
#32888 = EDGE_LOOP ( 'NONE', ( #34760, #3944, #16101, #7612 ) ) ;
#32889 = AXIS2_PLACEMENT_3D ( 'NONE', #5111, #20023, #16594 ) ;
#32890 = DIRECTION ( 'NONE',  ( -1.000000000000000000, -0.000000000000000000, 0.000000000000000000 ) ) ;
#32891 = VERTEX_POINT ( 'NONE', #40922 ) ;
#32892 = ORIENTED_EDGE ( 'NONE', *, *, #16625, .T. ) ;
#32893 = CARTESIAN_POINT ( 'NONE',  ( 0.000000000000000000, -25.88420570971381807, -27.13269053701123212 ) ) ;
#32894 = DIRECTION ( 'NONE',  ( -1.000000000000000000, 0.000000000000000000, 0.000000000000000000 ) ) ;
#32895 = DIRECTION ( 'NONE',  ( 0.000000000000000000, 0.000000000000000000, 1.000000000000000000 ) ) ;
#32896 = FACE_OUTER_BOUND ( 'NONE', #2182, .T. ) ;
#32897 = ORIENTED_EDGE ( 'NONE', *, *, #15003, .F. ) ;
#32898 = FACE_OUTER_BOUND ( 'NONE', #46064, .T. ) ;
#32899 = CARTESIAN_POINT ( 'NONE',  ( -15.44521549751111422, -137.7748507232956001, 5.500000000000000000 ) ) ;
#32900 = CARTESIAN_POINT ( 'NONE',  ( 10.00000000000000000, -26.08949754953044220, 27.05870788708222818 ) ) ;
#32901 = CARTESIAN_POINT ( 'NONE',  ( 10.00000000000000000, -10.96151621346514382, 35.95386929396252640 ) ) ;
#32902 = LINE ( 'NONE', #31974, #14532 ) ;
#32903 = ORIENTED_EDGE ( 'NONE', *, *, #16929, .T. ) ;
#32904 = ORIENTED_EDGE ( 'NONE', *, *, #16601, .T. ) ;
#32905 = LINE ( 'NONE', #10159, #6826 ) ;
#32906 = DIRECTION ( 'NONE',  ( -1.000000000000000000, -0.000000000000000000, 0.000000000000000000 ) ) ;
#32907 = CARTESIAN_POINT ( 'NONE',  ( 10.00000000000000000, 0.000000000000000000, 0.000000000000000000 ) ) ;
#32908 = DIRECTION ( 'NONE',  ( 0.000000000000000000, 0.8090169943749486725, -0.5877852522924713607 ) ) ;
#32909 = AXIS2_PLACEMENT_3D ( 'NONE', #26722, #23045, #26971 ) ;
#32910 = ORIENTED_EDGE ( 'NONE', *, *, #13381, .F. ) ;
#32911 = CARTESIAN_POINT ( 'NONE',  ( 11.99999999999999822, 0.000000000000000000, 0.000000000000000000 ) ) ;
#32912 = CARTESIAN_POINT ( 'NONE',  ( 11.99999999999999822, 14.66109333815564852, -73.73191006444555740 ) ) ;
#32913 = AXIS2_PLACEMENT_3D ( 'NONE', #45409, #7729, #4786 ) ;
#32914 = ORIENTED_EDGE ( 'NONE', *, *, #4585, .F. ) ;
#32915 = CARTESIAN_POINT ( 'NONE',  ( 5.000000000000002665, 78.73519480814955784, 22.90783923731657268 ) ) ;
#32916 = AXIS2_PLACEMENT_3D ( 'NONE', #15093, #19700, #19241 ) ;
#32917 = ADVANCED_FACE ( 'NONE', ( #33794 ), #41175, .F. ) ;
#32918 = ADVANCED_FACE ( 'NONE', ( #18864 ), #25241, .T. ) ;
#32919 = CARTESIAN_POINT ( 'NONE',  ( 11.99999999999999822, 20.40083707022987625, -72.35432306680462489 ) ) ;
#32920 = EDGE_CURVE ( 'NONE', #46892, #12455, #40204, .T. ) ;
#32921 = AXIS2_PLACEMENT_3D ( 'NONE', #6364, #28860, #44036 ) ;
#32922 = ORIENTED_EDGE ( 'NONE', *, *, #8156, .T. ) ;
#32923 = VERTEX_POINT ( 'NONE', #34047 ) ;
#32924 = VECTOR ( 'NONE', #37429, 1000.000000000000000 ) ;
#32925 = EDGE_CURVE ( 'NONE', #26652, #15212, #12901, .T. ) ;
#32926 = EDGE_CURVE ( 'NONE', #5723, #6467, #26982, .T. ) ;
#32927 = EDGE_CURVE ( 'NONE', #28709, #10878, #15243, .T. ) ;
#32928 = AXIS2_PLACEMENT_3D ( 'NONE', #46265, #19814, #24224 ) ;
#32929 = CARTESIAN_POINT ( 'NONE',  ( 10.00000000000000000, 0.000000000000000000, 0.000000000000000000 ) ) ;
#32930 = ORIENTED_EDGE ( 'NONE', *, *, #9427, .F. ) ;
#32931 = ORIENTED_EDGE ( 'NONE', *, *, #10395, .T. ) ;
#32932 = CYLINDRICAL_SURFACE ( 'NONE', #5862, 32.00000000000000000 ) ;
#32933 = ADVANCED_FACE ( 'NONE', ( #16190 ), #4914, .T. ) ;
#32934 = FACE_OUTER_BOUND ( 'NONE', #21729, .T. ) ;
#32935 = CARTESIAN_POINT ( 'NONE',  ( 10.00000000000000000, 0.000000000000000000, 0.000000000000000000 ) ) ;
#32936 = ORIENTED_EDGE ( 'NONE', *, *, #25086, .T. ) ;
#32937 = DIRECTION ( 'NONE',  ( -1.000000000000000000, 0.000000000000000000, -0.000000000000000000 ) ) ;
#32938 = ORIENTED_EDGE ( 'NONE', *, *, #11337, .T. ) ;
#32939 = ORIENTED_EDGE ( 'NONE', *, *, #7229, .T. ) ;
#32940 = VERTEX_POINT ( 'NONE', #5174 ) ;
#32941 = DIRECTION ( 'NONE',  ( 0.6064928550163524168, 0.7950889364178788110, -0.000000000000000000 ) ) ;
#32942 = DIRECTION ( 'NONE',  ( 0.000000000000000000, 0.000000000000000000, 1.000000000000000000 ) ) ;
#32943 = CIRCLE ( 'NONE', #22008, 32.50000000000000000 ) ;
#32944 = EDGE_CURVE ( 'NONE', #16462, #40697, #751, .T. ) ;
#32945 = DIRECTION ( 'NONE',  ( -1.000000000000000000, 0.000000000000000000, 0.000000000000000000 ) ) ;
#32947 = ORIENTED_EDGE ( 'NONE', *, *, #21841, .T. ) ;
#32946 = CIRCLE ( 'NONE', #47039, 16.00000000000000000 ) ;
#32948 = ORIENTED_EDGE ( 'NONE', *, *, #12885, .T. ) ;
#32949 = CARTESIAN_POINT ( 'NONE',  ( 10.00000000000000000, 0.000000000000000000, 0.000000000000000000 ) ) ;
#32950 = ORIENTED_EDGE ( 'NONE', *, *, #45035, .T. ) ;
#32951 = VECTOR ( 'NONE', #10309, 999.9999999999998863 ) ;
#32952 = DIRECTION ( 'NONE',  ( 0.000000000000000000, -0.3090169943749548898, 0.9510565162951511997 ) ) ;
#32953 = CARTESIAN_POINT ( 'NONE',  ( 10.00000000000000000, -54.21277698773715059, 55.38113227695762930 ) ) ;
#32954 = LINE ( 'NONE', #47880, #24467 ) ;
#32955 = ORIENTED_EDGE ( 'NONE', *, *, #5265, .F. ) ;
#32956 = DIRECTION ( 'NONE',  ( 1.000000000000000000, 0.000000000000000000, 0.000000000000000000 ) ) ;
#32957 = CYLINDRICAL_SURFACE ( 'NONE', #5675, 11.59999999999999787 ) ;
#32958 = AXIS2_PLACEMENT_3D ( 'NONE', #42925, #46838, #16970 ) ;
#32959 = AXIS2_PLACEMENT_3D ( 'NONE', #31799, #9484, #46942 ) ;
#32960 = FACE_OUTER_BOUND ( 'NONE', #28802, .T. ) ;
#32961 = DIRECTION ( 'NONE',  ( -1.000000000000000000, 0.000000000000000000, -0.000000000000000000 ) ) ;
#32962 = ADVANCED_FACE ( 'NONE', ( #34279 ), #37972, .F. ) ;
#32963 = DIRECTION ( 'NONE',  ( 0.000000000000000000, 0.000000000000000000, 1.000000000000000000 ) ) ;
#32964 = VERTEX_POINT ( 'NONE', #30881 ) ;
#32965 = DIRECTION ( 'NONE',  ( 0.000000000000000000, 1.000000000000000000, 3.491481338843133750E-15 ) ) ;
#32966 = ORIENTED_EDGE ( 'NONE', *, *, #15138, .T. ) ;
#32967 = AXIS2_PLACEMENT_3D ( 'NONE', #29349, #21985, #36445 ) ;
#32968 = CARTESIAN_POINT ( 'NONE',  ( 0.000000000000000000, 16.65560815589464028, -38.55633173626993226 ) ) ;
#32969 = ORIENTED_EDGE ( 'NONE', *, *, #9286, .T. ) ;
#32970 = CARTESIAN_POINT ( 'NONE',  ( 0.000000000000000000, -120.0000000000000000, 2.500000000000000000 ) ) ;
#32971 = FACE_OUTER_BOUND ( 'NONE', #19104, .T. ) ;
#32972 = CARTESIAN_POINT ( 'NONE',  ( 10.00000000000000000, 0.000000000000000000, 0.000000000000000000 ) ) ;
#32973 = CARTESIAN_POINT ( 'NONE',  ( 10.00000000000000000, 12.42422080174639021, 35.38097989696516521 ) ) ;
#32974 = ADVANCED_FACE ( 'NONE', ( #30624 ), #4677, .T. ) ;
#32975 = EDGE_LOOP ( 'NONE', ( #35232, #21577, #11205, #18299 ) ) ;
#32976 = CARTESIAN_POINT ( 'NONE',  ( -119.3426274441927433, -132.5434155921188619, 5.500000000000000000 ) ) ;
#32977 = DIRECTION ( 'NONE',  ( -1.000000000000000000, -0.000000000000000000, -0.000000000000000000 ) ) ;
#32978 = EDGE_CURVE ( 'NONE', #5424, #17233, #529, .T. ) ;
#32979 = PLANE ( 'NONE',  #38515 ) ;
#32980 = EDGE_CURVE ( 'NONE', #42340, #8001, #23054, .T. ) ;
#32981 = CARTESIAN_POINT ( 'NONE',  ( -3.000000000000000000, -22.67460108101783334, 6.353146135317912169 ) ) ;
#32982 = EDGE_CURVE ( 'NONE', #12875, #28552, #23928, .T. ) ;
#32983 = ORIENTED_EDGE ( 'NONE', *, *, #5599, .T. ) ;
#32984 = ORIENTED_EDGE ( 'NONE', *, *, #41255, .T. ) ;
#32985 = AXIS2_PLACEMENT_3D ( 'NONE', #29970, #348, #7464 ) ;
#32986 = EDGE_CURVE ( 'NONE', #13936, #5271, #15460, .T. ) ;
#32987 = ORIENTED_EDGE ( 'NONE', *, *, #31805, .F. ) ;
#32988 = CIRCLE ( 'NONE', #26779, 31.99999999999998579 ) ;
#32989 = DIRECTION ( 'NONE',  ( -1.000000000000000000, -0.000000000000000000, -0.000000000000000000 ) ) ;
#32990 = LINE ( 'NONE', #9999, #34711 ) ;
#32991 = VERTEX_POINT ( 'NONE', #26714 ) ;
#32992 = VECTOR ( 'NONE', #29484, 1000.000000000000000 ) ;
#32993 = FACE_OUTER_BOUND ( 'NONE', #30371, .T. ) ;
#32994 = CIRCLE ( 'NONE', #11914, 31.99999999999999289 ) ;
#32995 = ORIENTED_EDGE ( 'NONE', *, *, #8553, .T. ) ;
#32996 = ORIENTED_EDGE ( 'NONE', *, *, #3986, .F. ) ;
#32997 = PLANE ( 'NONE',  #26642 ) ;
#32998 = ORIENTED_EDGE ( 'NONE', *, *, #7083, .T. ) ;
#32999 = CARTESIAN_POINT ( 'NONE',  ( 11.99999999999999822, 75.54627589209944460, 17.28742895386110945 ) ) ;
#33000 = ORIENTED_EDGE ( 'NONE', *, *, #37682, .F. ) ;
#33001 = ORIENTED_EDGE ( 'NONE', *, *, #30368, .F. ) ;
#33002 = DIRECTION ( 'NONE',  ( -1.000000000000000000, 0.000000000000000000, -0.000000000000000000 ) ) ;
#33003 = CARTESIAN_POINT ( 'NONE',  ( 10.00000000000000000, -12.42422080174663712, 35.38097989696507994 ) ) ;
#33004 = DIRECTION ( 'NONE',  ( -1.000000000000000000, 0.000000000000000000, -0.000000000000000000 ) ) ;
#33005 = ORIENTED_EDGE ( 'NONE', *, *, #28283, .T. ) ;
#33006 = VERTEX_POINT ( 'NONE', #4452 ) ;
#33007 = AXIS2_PLACEMENT_3D ( 'NONE', #24316, #1569, #1807 ) ;
#33008 = DIRECTION ( 'NONE',  ( 0.000000000000000000, 0.000000000000000000, -1.000000000000000000 ) ) ;
#33009 = CARTESIAN_POINT ( 'NONE',  ( 10.00000000000000000, 0.000000000000000000, 0.000000000000000000 ) ) ;
#33010 = AXIS2_PLACEMENT_3D ( 'NONE', #7383, #48004, #10818 ) ;
#33011 = ORIENTED_EDGE ( 'NONE', *, *, #46306, .F. ) ;
#33012 = VERTEX_POINT ( 'NONE', #35014 ) ;
#33013 = CYLINDRICAL_SURFACE ( 'NONE', #22848, 77.49899999999999523 ) ;
#33014 = DIRECTION ( 'NONE',  ( 0.000000000000000000, 0.000000000000000000, 1.000000000000000000 ) ) ;
#33015 = ORIENTED_EDGE ( 'NONE', *, *, #16396, .F. ) ;
#33016 = VECTOR ( 'NONE', #34449, 1000.000000000000000 ) ;
#33017 = ORIENTED_EDGE ( 'NONE', *, *, #6802, .F. ) ;
#33018 = FACE_OUTER_BOUND ( 'NONE', #37717, .T. ) ;
#33019 = CARTESIAN_POINT ( 'NONE',  ( 10.00000000000000000, -68.55367621811173251, 44.99326035066030016 ) ) ;
#33020 = DIRECTION ( 'NONE',  ( -1.000000000000000000, 0.000000000000000000, -0.000000000000000000 ) ) ;
#33021 = DIRECTION ( 'NONE',  ( 2.889240119132116694E-16, -1.000000000000000000, 0.000000000000000000 ) ) ;
#33022 = CARTESIAN_POINT ( 'NONE',  ( -23.97194136764370498, -131.3950000906648938, 5.500000000000000000 ) ) ;
#33023 = AXIS2_PLACEMENT_3D ( 'NONE', #30221, #19905, #15293 ) ;
#33024 = DIRECTION ( 'NONE',  ( 0.000000000000000000, 0.000000000000000000, 1.000000000000000000 ) ) ;
#33025 = EDGE_CURVE ( 'NONE', #10422, #40361, #30193, .T. ) ;
#33026 = VECTOR ( 'NONE', #20937, 1000.000000000000000 ) ;
#33027 = CYLINDRICAL_SURFACE ( 'NONE', #20796, 31.99999999999998579 ) ;
#33028 = DIRECTION ( 'NONE',  ( -1.000000000000000000, -0.000000000000000000, -0.000000000000000000 ) ) ;
#33029 = EDGE_CURVE ( 'NONE', #7137, #33736, #16418, .T. ) ;
#33030 = CIRCLE ( 'NONE', #36937, 77.49900000000000944 ) ;
#33031 = DIRECTION ( 'NONE',  ( 0.000000000000000000, 0.7604059656000322631, -0.6494480483301821039 ) ) ;
#33032 = CARTESIAN_POINT ( 'NONE',  ( -22.17439115976385366, -112.2188447712574799, 2.500000000000000000 ) ) ;
#33033 = EDGE_CURVE ( 'NONE', #13922, #38765, #26964, .T. ) ;
#33034 = FILL_AREA_STYLE_COLOUR ( '', #1472 ) ;
#33035 = CARTESIAN_POINT ( 'NONE',  ( -3.000000000000000000, -0.9646360437375307573, 23.52805723605590060 ) ) ;
#33036 = ORIENTED_EDGE ( 'NONE', *, *, #39300, .F. ) ;
#33037 = ORIENTED_EDGE ( 'NONE', *, *, #9495, .T. ) ;
#33038 = ORIENTED_EDGE ( 'NONE', *, *, #10061, .F. ) ;
#33039 = EDGE_CURVE ( 'NONE', #1298, #22174, #21582, .T. ) ;
#33040 = ORIENTED_EDGE ( 'NONE', *, *, #957, .T. ) ;
#33041 = PRODUCT_DEFINITION_CONTEXT ( 'detailed design', #23220, 'design' ) ;
#33042 = DIRECTION ( 'NONE',  ( 0.000000000000000000, 0.3090169943749411785, 0.9510565162951556406 ) ) ;
#33043 = ADVANCED_FACE ( 'NONE', ( #27443 ), #11550, .T. ) ;
#33044 = EDGE_CURVE ( 'NONE', #23927, #8722, #41895, .T. ) ;
#33045 = CIRCLE ( 'NONE', #36160, 16.00000000000000000 ) ;
#33046 = CARTESIAN_POINT ( 'NONE',  ( -30.50000000000000000, -120.0000000000000000, 2.500000000000000000 ) ) ;
#33047 = VERTEX_POINT ( 'NONE', #6129 ) ;
#33048 = AXIS2_PLACEMENT_3D ( 'NONE', #22274, #14925, #44779 ) ;
#33049 = VECTOR ( 'NONE', #5644, 1000.000000000000000 ) ;
#33050 = CARTESIAN_POINT ( 'NONE',  ( 11.99999999999999822, -49.70050353004846500, -59.46389618802017907 ) ) ;
#33051 = CIRCLE ( 'NONE', #26806, 77.49900000000002365 ) ;
#33052 = ORIENTED_EDGE ( 'NONE', *, *, #10176, .T. ) ;
#33053 = CARTESIAN_POINT ( 'NONE',  ( 10.00000000000000000, 0.000000000000000000, 0.000000000000000000 ) ) ;
#33054 = AXIS2_PLACEMENT_3D ( 'NONE', #26643, #38146, #37655 ) ;
#33055 = ORIENTED_EDGE ( 'NONE', *, *, #41029, .F. ) ;
#33056 = CARTESIAN_POINT ( 'NONE',  ( -10.00000000000000000, 0.000000000000000000, 0.000000000000000000 ) ) ;
#33057 = AXIS2_PLACEMENT_3D ( 'NONE', #16368, #937, #23457 ) ;
#33058 = EDGE_CURVE ( 'NONE', #3151, #46329, #34083, .T. ) ;
#33059 = DIRECTION ( 'NONE',  ( -0.000000000000000000, -0.000000000000000000, -1.000000000000000000 ) ) ;
#33060 = CIRCLE ( 'NONE', #1813, 82.00000000000000000 ) ;
#33061 = VERTEX_POINT ( 'NONE', #35251 ) ;
#33062 = CARTESIAN_POINT ( 'NONE',  ( 10.00000000000000000, -35.91791733033426226, -68.67312586195033930 ) ) ;
#33063 = AXIS2_PLACEMENT_3D ( 'NONE', #28728, #43174, #9388 ) ;
#33064 = ORIENTED_EDGE ( 'NONE', *, *, #32854, .T. ) ;
#33065 = CARTESIAN_POINT ( 'NONE',  ( 10.00000000000000000, 0.000000000000000000, 0.000000000000000000 ) ) ;
#33066 = DIRECTION ( 'NONE',  ( -1.000000000000000000, 0.000000000000000000, 0.000000000000000000 ) ) ;
#33067 = EDGE_LOOP ( 'NONE', ( #9296, #15747, #44927, #11886 ) ) ;
#33068 = CYLINDRICAL_SURFACE ( 'NONE', #33095, 42.00000000000000000 ) ;
#33069 = FACE_OUTER_BOUND ( 'NONE', #2246, .T. ) ;
#33070 = DIRECTION ( 'NONE',  ( 0.000000000000000000, 0.000000000000000000, -1.000000000000000000 ) ) ;
#33071 = ADVANCED_FACE ( 'NONE', ( #16658 ), #35501, .T. ) ;
#33072 = DIRECTION ( 'NONE',  ( -1.000000000000000000, -0.000000000000000000, -0.000000000000000000 ) ) ;
#33073 = ORIENTED_EDGE ( 'NONE', *, *, #14432, .F. ) ;
#33074 = FACE_OUTER_BOUND ( 'NONE', #27391, .T. ) ;
#33075 = VERTEX_POINT ( 'NONE', #38948 ) ;
#33076 = ORIENTED_EDGE ( 'NONE', *, *, #9448, .T. ) ;
#33077 = FACE_OUTER_BOUND ( 'NONE', #10585, .T. ) ;
#33078 = LINE ( 'NONE', #22323, #20713 ) ;
#33079 = EDGE_CURVE ( 'NONE', #43138, #9412, #10030, .T. ) ;
#33080 = DIRECTION ( 'NONE',  ( 0.000000000000000000, 0.000000000000000000, 1.000000000000000000 ) ) ;
#33081 = CYLINDRICAL_SURFACE ( 'NONE', #17231, 32.00000000000000000 ) ;
#33082 = FACE_OUTER_BOUND ( 'NONE', #23254, .T. ) ;
#33083 = VERTEX_POINT ( 'NONE', #42855 ) ;
#33084 = CIRCLE ( 'NONE', #47919, 16.00000000000000000 ) ;
#33085 = EDGE_CURVE ( 'NONE', #35643, #46491, #24954, .T. ) ;
#33086 = CARTESIAN_POINT ( 'NONE',  ( 5.999999999999999112, -27.74655509720726698, 77.16300072079651784 ) ) ;
#33087 = DIRECTION ( 'NONE',  ( 0.000000000000000000, 0.9969173337331282969, -0.07845909572784179331 ) ) ;
#33088 = AXIS2_PLACEMENT_3D ( 'NONE', #31322, #34472, #20041 ) ;
#33089 = CARTESIAN_POINT ( 'NONE',  ( 0.000000000000000000, -36.72794159290288718, 65.59268652807197952 ) ) ;
#33090 = ORIENTED_EDGE ( 'NONE', *, *, #38451, .F. ) ;
#33091 = DIRECTION ( 'NONE',  ( -1.000000000000000000, 0.000000000000000000, 0.000000000000000000 ) ) ;
#33092 = DIRECTION ( 'NONE',  ( -1.000000000000000000, 0.000000000000000000, 0.000000000000000000 ) ) ;
#33093 = DIRECTION ( 'NONE',  ( -1.000000000000000000, -0.000000000000000000, 0.000000000000000000 ) ) ;
#33094 = AXIS2_PLACEMENT_3D ( 'NONE', #6728, #10392, #21404 ) ;
#33095 = AXIS2_PLACEMENT_3D ( 'NONE', #10808, #14483, #25715 ) ;
#33096 = AXIS2_PLACEMENT_3D ( 'NONE', #1516, #28415, #43360 ) ;
#33097 = VECTOR ( 'NONE', #42008, 1000.000000000000000 ) ;
#33098 = ORIENTED_EDGE ( 'NONE', *, *, #7656, .F. ) ;
#33099 = DIRECTION ( 'NONE',  ( -0.000000000000000000, -0.000000000000000000, -1.000000000000000000 ) ) ;
#33100 = DIRECTION ( 'NONE',  ( 1.000000000000000000, 0.000000000000000000, -0.000000000000000000 ) ) ;
#33101 = CARTESIAN_POINT ( 'NONE',  ( 0.000000000000000000, -20.40083707022829174, -72.35432306680507963 ) ) ;
#33102 = EDGE_CURVE ( 'NONE', #21677, #26799, #23824, .T. ) ;
#33103 = CARTESIAN_POINT ( 'NONE',  ( 10.00000000000000000, -12.26510123303234501, -35.53030884539098366 ) ) ;
#33104 = AXIS2_PLACEMENT_3D ( 'NONE', #15362, #30036, #18282 ) ;
#33105 = EDGE_CURVE ( 'NONE', #12571, #38965, #27940, .T. ) ;
#33106 = ADVANCED_FACE ( 'NONE', ( #24482 ), #36214, .T. ) ;
#33107 = ORIENTED_EDGE ( 'NONE', *, *, #23640, .F. ) ;
#33109 = CARTESIAN_POINT ( 'NONE',  ( 6.000000000000000000, -3.894527615418457600, 81.90746397400387480 ) ) ;
#33108 = VECTOR ( 'NONE', #22030, 1000.000000000000000 ) ;
#33110 = AXIS2_PLACEMENT_3D ( 'NONE', #27516, #42440, #26781 ) ;
#33111 = VERTEX_POINT ( 'NONE', #13466 ) ;
#33112 = DIRECTION ( 'NONE',  ( -1.000000000000000000, -0.000000000000000000, 0.000000000000000000 ) ) ;
#33113 = VECTOR ( 'NONE', #28180, 1000.000000000000000 ) ;
#33114 = APPLICATION_PROTOCOL_DEFINITION ( 'draft international standard', 'automotive_design', 1998, #23220 ) ;
#33115 = CARTESIAN_POINT ( 'NONE',  ( 15.00000000000000000, 0.000000000000000000, 0.000000000000000000 ) ) ;
#33116 = VECTOR ( 'NONE', #4416, 1000.000000000000114 ) ;
#33117 = ORIENTED_EDGE ( 'NONE', *, *, #24203, .F. ) ;
#33118 = ADVANCED_FACE ( 'NONE', ( #2210 ), #9538, .T. ) ;
#33119 = CARTESIAN_POINT ( 'NONE',  ( 11.99999999999999822, 34.44570377933598593, 69.42325613327452061 ) ) ;
#33120 = ORIENTED_EDGE ( 'NONE', *, *, #30890, .T. ) ;
#33121 = VECTOR ( 'NONE', #28236, 1000.000000000000000 ) ;
#33122 = CIRCLE ( 'NONE', #4244, 31.99999999999998224 ) ;
#33123 = DIRECTION ( 'NONE',  ( 0.000000000000000000, -0.1045284632676449221, 0.9945218953682741780 ) ) ;
#33124 = VERTEX_POINT ( 'NONE', #17133 ) ;
#33125 = CARTESIAN_POINT ( 'NONE',  ( 10.00000000000000000, 12.42422080174639021, 35.38097989696516521 ) ) ;
#33126 = VECTOR ( 'NONE', #40991, 1000.000000000000000 ) ;
#33127 = VECTOR ( 'NONE', #5039, 1000.000000000000000 ) ;
#33128 = DIRECTION ( 'NONE',  ( 0.000000000000000000, 0.5877852522924744694, -0.8090169943749465631 ) ) ;
#33129 = VECTOR ( 'NONE', #44186, 1000.000000000000000 ) ;
#33130 = ORIENTED_EDGE ( 'NONE', *, *, #13550, .F. ) ;
#33131 = DIRECTION ( 'NONE',  ( 0.000000000000000000, 0.000000000000000000, 1.000000000000000000 ) ) ;
#33132 = ORIENTED_EDGE ( 'NONE', *, *, #24768, .F. ) ;
#33133 = CARTESIAN_POINT ( 'NONE',  ( 0.000000000000000000, 9.615535125378775305, 24.73947219025917121 ) ) ;
#33134 = PLANE ( 'NONE',  #11663 ) ;
#33135 = DIRECTION ( 'NONE',  ( -1.000000000000000000, -0.000000000000000000, 0.000000000000000000 ) ) ;
#33136 = DIRECTION ( 'NONE',  ( -1.000000000000000000, 0.000000000000000000, -0.000000000000000000 ) ) ;
#33137 = EDGE_CURVE ( 'NONE', #29574, #12245, #23852, .T. ) ;
#33138 = VECTOR ( 'NONE', #36882, 1000.000000000000114 ) ;
#33139 = CIRCLE ( 'NONE', #39404, 1.000000000000000000 ) ;
#33140 = ORIENTED_EDGE ( 'NONE', *, *, #1047, .T. ) ;
#33141 = CARTESIAN_POINT ( 'NONE',  ( 10.00000000000000000, -37.22597642581153821, -5.202137450156795850 ) ) ;
#33142 = EDGE_LOOP ( 'NONE', ( #4214, #41816, #10537, #18274 ) ) ;
#33143 = ORIENTED_EDGE ( 'NONE', *, *, #29244, .F. ) ;
#33144 = CIRCLE ( 'NONE', #22974, 16.00000000000000000 ) ;
#33145 = FACE_OUTER_BOUND ( 'NONE', #1342, .T. ) ;
#33146 = AXIS2_PLACEMENT_3D ( 'NONE', #18605, #15188, #19322 ) ;
#33147 = AXIS2_PLACEMENT_3D ( 'NONE', #27814, #21161, #16786 ) ;
#33148 = ADVANCED_FACE ( 'NONE', ( #2673 ), #13001, .T. ) ;
#33149 = LINE ( 'NONE', #29953, #22273 ) ;
#33150 = CARTESIAN_POINT ( 'NONE',  ( 11.99999999999999822, -65.59268652807183742, -36.72794159290312166 ) ) ;
#33151 = DIRECTION ( 'NONE',  ( -1.000000000000000000, 0.000000000000000000, -0.000000000000000000 ) ) ;
#33152 = ORIENTED_EDGE ( 'NONE', *, *, #37382, .F. ) ;
#33153 = CARTESIAN_POINT ( 'NONE',  ( 11.99999999999999822, -59.03342792756297541, 46.54456581323783126 ) ) ;
#33154 = EDGE_CURVE ( 'NONE', #32480, #42780, #45734, .T. ) ;
#33155 = CARTESIAN_POINT ( 'NONE',  ( -3.000000000000000000, 6.762365576493310826, 25.66652317338401090 ) ) ;
#33156 = DIRECTION ( 'NONE',  ( 0.000000000000000000, 0.000000000000000000, 1.000000000000000000 ) ) ;
#33157 = DIRECTION ( 'NONE',  ( 0.000000000000000000, 0.4999999999999929501, 0.8660254037844427044 ) ) ;
#33158 = DIRECTION ( 'NONE',  ( -1.000000000000000000, -0.000000000000000000, -0.000000000000000000 ) ) ;
#33159 = VERTEX_POINT ( 'NONE', #20815 ) ;
#33160 = ORIENTED_EDGE ( 'NONE', *, *, #7285, .F. ) ;
#33161 = CYLINDRICAL_SURFACE ( 'NONE', #19325, 1.000000000000000888 ) ;
#33162 = CYLINDRICAL_SURFACE ( 'NONE', #43504, 31.99999999999998579 ) ;
#33163 = LINE ( 'NONE', #48091, #34546 ) ;
#33164 = CARTESIAN_POINT ( 'NONE',  ( -3.000000000000000000, 20.85821328998741109, 10.92862929874522315 ) ) ;
#33165 = ADVANCED_FACE ( 'NONE', ( #24730 ), #31856, .T. ) ;
#33166 = EDGE_CURVE ( 'NONE', #41935, #17996, #47000, .T. ) ;
#33167 = DIRECTION ( 'NONE',  ( 0.6064928550163524168, 0.7950889364178788110, -0.000000000000000000 ) ) ;
#33168 = DIRECTION ( 'NONE',  ( 0.000000000000000000, 0.8910065241883688980, -0.4539904997395447506 ) ) ;
#33169 = DIRECTION ( 'NONE',  ( -1.000000000000000000, 0.000000000000000000, -0.000000000000000000 ) ) ;
#33170 = ORIENTED_EDGE ( 'NONE', *, *, #3300, .F. ) ;
#33171 = CIRCLE ( 'NONE', #12080, 77.49899999999999523 ) ;
#33172 = DIRECTION ( 'NONE',  ( -1.000000000000000000, 0.000000000000000000, -0.000000000000000000 ) ) ;
#33173 = VECTOR ( 'NONE', #11082, 1000.000000000000114 ) ;
#33174 = VECTOR ( 'NONE', #39719, 1000.000000000000000 ) ;
#33175 = CARTESIAN_POINT ( 'NONE',  ( 0.000000000000000000, 21.60688246758697062, -79.10210256391344785 ) ) ;
#33176 = VERTEX_POINT ( 'NONE', #39675 ) ;
#33177 = EDGE_CURVE ( 'NONE', #37777, #36444, #5402, .T. ) ;
#33178 = VECTOR ( 'NONE', #43724, 1000.000000000000000 ) ;
#33179 = AXIS2_PLACEMENT_3D ( 'NONE', #21951, #7022, #41299 ) ;
#33180 = EDGE_LOOP ( 'NONE', ( #33410, #1045, #46426, #4156 ) ) ;
#33181 = AXIS2_PLACEMENT_3D ( 'NONE', #43542, #32282, #32523 ) ;
#33182 = CYLINDRICAL_SURFACE ( 'NONE', #21848, 31.99999999999999289 ) ;
#33183 = ORIENTED_EDGE ( 'NONE', *, *, #29787, .T. ) ;
#33184 = VECTOR ( 'NONE', #404, 1000.000000000000000 ) ;
#33185 = ORIENTED_EDGE ( 'NONE', *, *, #29185, .T. ) ;
#33186 = CARTESIAN_POINT ( 'NONE',  ( 10.00000000000000000, -27.13269053701078448, -25.88420570971428702 ) ) ;
#33187 = DIRECTION ( 'NONE',  ( 0.000000000000000000, 0.000000000000000000, 1.000000000000000000 ) ) ;
#33188 = DIRECTION ( 'NONE',  ( 0.000000000000000000, 0.000000000000000000, 1.000000000000000000 ) ) ;
#33189 = VERTEX_POINT ( 'NONE', #46775 ) ;
#33190 = DIRECTION ( 'NONE',  ( 0.000000000000000000, 0.000000000000000000, 1.000000000000000000 ) ) ;
#33191 = ORIENTED_EDGE ( 'NONE', *, *, #18313, .T. ) ;
#33192 = ORIENTED_EDGE ( 'NONE', *, *, #8657, .F. ) ;
#33193 = ORIENTED_EDGE ( 'NONE', *, *, #32399, .F. ) ;
#33194 = ORIENTED_EDGE ( 'NONE', *, *, #29966, .T. ) ;
#33195 = LINE ( 'NONE', #6773, #11590 ) ;
#33196 = FACE_OUTER_BOUND ( 'NONE', #36053, .T. ) ;
#33198 = FACE_OUTER_BOUND ( 'NONE', #16455, .T. ) ;
#33197 = CIRCLE ( 'NONE', #3502, 21.00000000000000000 ) ;
#33199 = VERTEX_POINT ( 'NONE', #13233 ) ;
#33200 = EDGE_LOOP ( 'NONE', ( #6955, #18224, #25112, #15124 ) ) ;
#33201 = FACE_OUTER_BOUND ( 'NONE', #3784, .T. ) ;
#33202 = ORIENTED_EDGE ( 'NONE', *, *, #13878, .T. ) ;
#33203 = CARTESIAN_POINT ( 'NONE',  ( 0.000000000000000000, 55.20638768913831029, -51.02545421589267960 ) ) ;
#33204 = AXIS2_PLACEMENT_3D ( 'NONE', #45325, #22577, #4698 ) ;
#33205 = ADVANCED_FACE ( 'NONE', ( #28156 ), #15576, .T. ) ;
#33206 = CARTESIAN_POINT ( 'NONE',  ( 11.99999999999999822, 78.73519480814985627, -22.90783923731548199 ) ) ;
#33207 = CARTESIAN_POINT ( 'NONE',  ( 0.000000000000000000, -10.74501242461307982, 35.92658777277507198 ) ) ;
#33208 = CARTESIAN_POINT ( 'NONE',  ( -18.12185313557660038, -104.9634299478706794, 5.500000000000000000 ) ) ;
#33209 = CARTESIAN_POINT ( 'NONE',  ( -3.000000000000000000, 20.85821328998756385, -10.92862929874494959 ) ) ;
#33210 = EDGE_CURVE ( 'NONE', #9886, #37732, #40608, .T. ) ;
#33211 = DIRECTION ( 'NONE',  ( -1.000000000000000000, 0.000000000000000000, 0.000000000000000000 ) ) ;
#33212 = CARTESIAN_POINT ( 'NONE',  ( 0.000000000000000000, -16.45098606841102651, -33.79645857604531045 ) ) ;
#33213 = DIRECTION ( 'NONE',  ( -1.000000000000000000, 0.000000000000000000, 0.000000000000000000 ) ) ;
#33214 = DIRECTION ( 'NONE',  ( -1.000000000000000000, 0.000000000000000000, -0.000000000000000000 ) ) ;
#33215 = AXIS2_PLACEMENT_3D ( 'NONE', #25050, #40002, #3257 ) ;
#33216 = VECTOR ( 'NONE', #46673, 999.9999999999998863 ) ;
#33217 = EDGE_LOOP ( 'NONE', ( #4228, #42275, #37213, #24572 ) ) ;
#33218 = EDGE_CURVE ( 'NONE', #30063, #6579, #10998, .T. ) ;
#33219 = DIRECTION ( 'NONE',  ( 0.9997280174009349762, -0.02332147558787674158, 0.000000000000000000 ) ) ;
#33220 = AXIS2_PLACEMENT_3D ( 'NONE', #12278, #23511, #38713 ) ;
#33221 = DIRECTION ( 'NONE',  ( 1.000000000000000000, 5.778480238264233142E-17, -0.000000000000000000 ) ) ;
#33222 = CARTESIAN_POINT ( 'NONE',  ( 0.000000000000000000, 73.95703589264006439, -23.16143007188350822 ) ) ;
#33223 = CARTESIAN_POINT ( 'NONE',  ( 24.95699195200416654, -110.9640411295978595, -5.500000000000000000 ) ) ;
#33224 = AXIS2_PLACEMENT_3D ( 'NONE', #10651, #25558, #31972 ) ;
#33225 = EDGE_CURVE ( 'NONE', #17540, #32047, #42633, .T. ) ;
#33226 = DIRECTION ( 'NONE',  ( -1.000000000000000000, -0.000000000000000000, -0.000000000000000000 ) ) ;
#33227 = LINE ( 'NONE', #37137, #43594 ) ;
#33228 = LINE ( 'NONE', #14639, #12250 ) ;
#33229 = DIRECTION ( 'NONE',  ( 0.000000000000000000, 1.000000000000000000, 7.228014483236689653E-16 ) ) ;
#33230 = EDGE_CURVE ( 'NONE', #46424, #37720, #6670, .T. ) ;
#33231 =( REPRESENTATION_RELATIONSHIP ('NONE','NONE', #5957, #21223 ) REPRESENTATION_RELATIONSHIP_WITH_TRANSFORMATION ( #28668 )SHAPE_REPRESENTATION_RELATIONSHIP( ) );
#33232 = AXIS2_PLACEMENT_3D ( 'NONE', #45030, #44777, #26668 ) ;
#33233 = CARTESIAN_POINT ( 'NONE',  ( 10.00000000000000000, 16.45098606841126454, 33.79645857604518966 ) ) ;
#33234 = FILL_AREA_STYLE_COLOUR ( '', #34230 ) ;
#33235 = CARTESIAN_POINT ( 'NONE',  ( 10.00000000000000000, -81.96053171279902472, 2.543863470248087566 ) ) ;
#33236 = VERTEX_POINT ( 'NONE', #44044 ) ;
#33237 = EDGE_CURVE ( 'NONE', #37785, #44445, #10587, .T. ) ;
#33238 = VECTOR ( 'NONE', #1564, 1000.000000000000000 ) ;
#33239 = EDGE_LOOP ( 'NONE', ( #46693, #10961, #38284, #45001 ) ) ;
#33240 = CARTESIAN_POINT ( 'NONE',  ( 11.99999999999999822, 73.72996012237460661, -14.67089635893632504 ) ) ;
#33241 = CARTESIAN_POINT ( 'NONE',  ( -35.37301231164799731, -123.0000000000000142, 2.500000000000000000 ) ) ;
#33242 = ORIENTED_EDGE ( 'NONE', *, *, #24833, .F. ) ;
#33243 = EDGE_CURVE ( 'NONE', #27962, #33538, #37938, .T. ) ;
#33244 = AXIS2_PLACEMENT_3D ( 'NONE', #39469, #46081, #46320 ) ;
#33245 = DIRECTION ( 'NONE',  ( -0.9227826878668540234, -0.3853207896976547642, 0.000000000000000000 ) ) ;
#33246 = ORIENTED_EDGE ( 'NONE', *, *, #35460, .F. ) ;
#33247 = AXIS2_PLACEMENT_3D ( 'NONE', #17610, #32552, #47475 ) ;
#33248 = ORIENTED_EDGE ( 'NONE', *, *, #36639, .T. ) ;
#33249 = VECTOR ( 'NONE', #32657, 1000.000000000000000 ) ;
#33250 = CIRCLE ( 'NONE', #7476, 82.00000000000000000 ) ;
#33251 = CARTESIAN_POINT ( 'NONE',  ( 0.000000000000000000, 0.000000000000000000, 0.000000000000000000 ) ) ;
#33252 = EDGE_LOOP ( 'NONE', ( #47342, #21648 ) ) ;
#33253 = CARTESIAN_POINT ( 'NONE',  ( -10.00000000000000000, 0.000000000000000000, 0.000000000000000000 ) ) ;
#33254 = ORIENTED_EDGE ( 'NONE', *, *, #45088, .T. ) ;
#33255 = EDGE_CURVE ( 'NONE', #9753, #24727, #41065, .T. ) ;
#33256 = DIRECTION ( 'NONE',  ( -1.000000000000000000, 0.000000000000000000, 0.000000000000000000 ) ) ;
#33257 = EDGE_CURVE ( 'NONE', #8722, #33303, #30117, .T. ) ;
#33258 = CIRCLE ( 'NONE', #30171, 31.99999999999999645 ) ;
#33259 = FACE_OUTER_BOUND ( 'NONE', #25879, .T. ) ;
#33260 = LINE ( 'NONE', #43562, #31475 ) ;
#33261 = EDGE_LOOP ( 'NONE', ( #40674, #11284, #8735, #12698 ) ) ;
#33262 = EDGE_CURVE ( 'NONE', #45718, #6408, #27007, .T. ) ;
#33263 = EDGE_LOOP ( 'NONE', ( #9755, #9814, #27519, #29640 ) ) ;
#33264 = CARTESIAN_POINT ( 'NONE',  ( 11.99999999999999822, 76.66974797899837313, 11.30684508768366747 ) ) ;
#33265 = VECTOR ( 'NONE', #38957, 1000.000000000000000 ) ;
#33266 = CARTESIAN_POINT ( 'NONE',  ( 10.00000000000000000, -22.90783923731575911, -78.73519480814978522 ) ) ;
#33267 = ORIENTED_EDGE ( 'NONE', *, *, #20166, .F. ) ;
#33268 = ORIENTED_EDGE ( 'NONE', *, *, #1830, .T. ) ;
#33269 = EDGE_CURVE ( 'NONE', #5219, #7382, #3511, .T. ) ;
#33270 = LINE ( 'NONE', #44286, #17384 ) ;
#33271 = DIRECTION ( 'NONE',  ( -1.000000000000000000, 0.000000000000000000, 0.000000000000000000 ) ) ;
#33272 = VERTEX_POINT ( 'NONE', #21534 ) ;
#33273 = FACE_OUTER_BOUND ( 'NONE', #13654, .T. ) ;
#33274 = FACE_OUTER_BOUND ( 'NONE', #3395, .T. ) ;
#33275 = CARTESIAN_POINT ( 'NONE',  ( 0.000000000000000000, -26.01480285779785362, -70.53064760720343429 ) ) ;
#33276 = CARTESIAN_POINT ( 'NONE',  ( -12.50000000000000000, -107.5000000000000000, -40.00000000000000000 ) ) ;
#33277 = PLANE ( 'NONE',  #5468 ) ;
#33278 = CARTESIAN_POINT ( 'NONE',  ( 10.00000000000000000, 30.84782396557248418, -21.32104025579081252 ) ) ;
#33279 = CIRCLE ( 'NONE', #3617, 82.00000000000000000 ) ;
#33280 = DIRECTION ( 'NONE',  ( -1.000000000000000000, 0.000000000000000000, -0.000000000000000000 ) ) ;
#33281 = CARTESIAN_POINT ( 'NONE',  ( 0.000000000000000000, -40.98264845739755202, 9.188173127307159405 ) ) ;
#33282 = AXIS2_PLACEMENT_3D ( 'NONE', #47826, #39295, #35860 ) ;
#33283 = FACE_OUTER_BOUND ( 'NONE', #14904, .T. ) ;
#33284 = CARTESIAN_POINT ( 'NONE',  ( 5.000000000000000000, -64.81221759200306565, -50.23322058963418613 ) ) ;
#33285 = AXIS2_PLACEMENT_3D ( 'NONE', #47302, #14003, #2043 ) ;
#33286 = CARTESIAN_POINT ( 'NONE',  ( 15.00000000000000000, 24.81905959214260804, -9.408202855044828894 ) ) ;
#33287 = EDGE_LOOP ( 'NONE', ( #12609, #31207, #22513, #2258 ) ) ;
#33288 = VERTEX_POINT ( 'NONE', #37183 ) ;
#33289 = EDGE_CURVE ( 'NONE', #30039, #44237, #3652, .T. ) ;
#33290 = CIRCLE ( 'NONE', #21591, 77.49899999999999523 ) ;
#33291 = CYLINDRICAL_SURFACE ( 'NONE', #13558, 77.49899999999999523 ) ;
#33292 = CIRCLE ( 'NONE', #12211, 77.49899999999999523 ) ;
#33293 = AXIS2_PLACEMENT_3D ( 'NONE', #36589, #6265, #44661 ) ;
#33294 = CARTESIAN_POINT ( 'NONE',  ( 11.99999999999999822, 76.66974797899852945, -11.30684508768257679 ) ) ;
#33295 = ORIENTED_EDGE ( 'NONE', *, *, #36616, .F. ) ;
#33296 = VECTOR ( 'NONE', #28344, 1000.000000000000000 ) ;
#33297 = ORIENTED_EDGE ( 'NONE', *, *, #1238, .T. ) ;
#33298 = EDGE_CURVE ( 'NONE', #45931, #17130, #6604, .T. ) ;
#33299 = CYLINDRICAL_SURFACE ( 'NONE', #6169, 31.99999999999998579 ) ;
#33300 = EDGE_LOOP ( 'NONE', ( #8666, #8865, #27313, #33731 ) ) ;
#33301 = CARTESIAN_POINT ( 'NONE',  ( 11.99999999999999822, -76.41127070299262414, -12.93880638057396304 ) ) ;
#33302 = VERTEX_POINT ( 'NONE', #33503 ) ;
#33303 = VERTEX_POINT ( 'NONE', #21762 ) ;
#33304 = ORIENTED_EDGE ( 'NONE', *, *, #5255, .T. ) ;
#33305 = ORIENTED_EDGE ( 'NONE', *, *, #36306, .F. ) ;
#33306 = CYLINDRICAL_SURFACE ( 'NONE', #34378, 82.00000000000000000 ) ;
#33307 = CIRCLE ( 'NONE', #20107, 16.00000000000000000 ) ;
#33308 = AXIS2_PLACEMENT_3D ( 'NONE', #19748, #31288, #42289 ) ;
#33309 = PLANE ( 'NONE',  #32847 ) ;
#33310 = ORIENTED_EDGE ( 'NONE', *, *, #41503, .T. ) ;
#33311 = ORIENTED_EDGE ( 'NONE', *, *, #20374, .T. ) ;
#33312 = EDGE_CURVE ( 'NONE', #47328, #41024, #35596, .T. ) ;
#33313 = CYLINDRICAL_SURFACE ( 'NONE', #37654, 31.99999999999999289 ) ;
#33314 = EDGE_LOOP ( 'NONE', ( #14059, #25363, #41602, #25619 ) ) ;
#33315 = CIRCLE ( 'NONE', #44258, 37.49900000000000233 ) ;
#33316 = DIRECTION ( 'NONE',  ( 0.000000000000000000, 0.000000000000000000, 1.000000000000000000 ) ) ;
#33317 = ADVANCED_FACE ( 'NONE', ( #40386 ), #38102, .F. ) ;
#33318 = CARTESIAN_POINT ( 'NONE',  ( 11.99999999999999822, -14.67089635893764665, 73.72996012237435082 ) ) ;
#33319 = ORIENTED_EDGE ( 'NONE', *, *, #45581, .T. ) ;
#33320 = DIRECTION ( 'NONE',  ( 0.000000000000000000, 0.7071067811865486830, -0.7071067811865463515 ) ) ;
#33321 = DIRECTION ( 'NONE',  ( 0.000000000000000000, 0.000000000000000000, 1.000000000000000000 ) ) ;
#33322 = CARTESIAN_POINT ( 'NONE',  ( 10.00000000000000000, 0.000000000000000000, 0.000000000000000000 ) ) ;
#33323 = FACE_BOUND ( 'NONE', #15353, .T. ) ;
#33324 = ORIENTED_EDGE ( 'NONE', *, *, #28242, .T. ) ;
#33325 = CIRCLE ( 'NONE', #2853, 42.00000000000000000 ) ;
#33326 = CARTESIAN_POINT ( 'NONE',  ( 2.874421927457452952, -143.3717286177755739, 5.500000000000000000 ) ) ;
#33327 = ORIENTED_EDGE ( 'NONE', *, *, #42174, .T. ) ;
#33328 = ORIENTED_EDGE ( 'NONE', *, *, #18616, .T. ) ;
#33329 = EDGE_CURVE ( 'NONE', #9618, #11259, #3153, .T. ) ;
#33330 = CARTESIAN_POINT ( 'NONE',  ( 0.000000000000000000, 81.96053171279902472, 2.543863470248677316 ) ) ;
#33331 = CARTESIAN_POINT ( 'NONE',  ( 6.000000000000000000, -80.55351364060599906, 15.33399622253457295 ) ) ;
#33332 = VERTEX_POINT ( 'NONE', #43801 ) ;
#33333 = CARTESIAN_POINT ( 'NONE',  ( 0.000000000000000000, 0.000000000000000000, 53.20000000000001705 ) ) ;
#33334 = AXIS2_PLACEMENT_3D ( 'NONE', #34531, #31379, #42868 ) ;
#33335 = EDGE_CURVE ( 'NONE', #23424, #19153, #10265, .T. ) ;
#33336 = FACE_OUTER_BOUND ( 'NONE', #47789, .T. ) ;
#33337 = CARTESIAN_POINT ( 'NONE',  ( -14.25258209288423750, -138.6845900058201551, -2.500000000000000000 ) ) ;
#33338 = ORIENTED_EDGE ( 'NONE', *, *, #32285, .F. ) ;
#33339 = AXIS2_PLACEMENT_3D ( 'NONE', #37712, #37230, #45296 ) ;
#33340 = LINE ( 'NONE', #14743, #17155 ) ;
#33341 = CYLINDRICAL_SURFACE ( 'NONE', #47745, 77.49899999999999523 ) ;
#33342 = CARTESIAN_POINT ( 'NONE',  ( -12.50000000000000000, -132.5000000000000000, -40.00000000000000000 ) ) ;
#33343 = CARTESIAN_POINT ( 'NONE',  ( 10.00000000000000000, -8.830959090342926032, 74.65491531819115778 ) ) ;
#33344 = LINE ( 'NONE', #35447, #5602 ) ;
#33345 = DIRECTION ( 'NONE',  ( -1.000000000000000000, 0.000000000000000000, 0.000000000000000000 ) ) ;
#33346 = CARTESIAN_POINT ( 'NONE',  ( 0.000000000000000000, 35.53030884539102630, -12.26510123303222599 ) ) ;
#33347 = CARTESIAN_POINT ( 'NONE',  ( 11.99999999999999822, -51.29473840253177741, -63.97538442413483750 ) ) ;
#33348 = CYLINDRICAL_SURFACE ( 'NONE', #42516, 82.00000000000000000 ) ;
#33349 = CARTESIAN_POINT ( 'NONE',  ( 14.59956846177685996, -138.4757300459248484, -2.500000000000000000 ) ) ;
#33350 = DIRECTION ( 'NONE',  ( 0.6575728627325955200, -0.7533909544171997208, 0.000000000000000000 ) ) ;
#33351 = ORIENTED_EDGE ( 'NONE', *, *, #4825, .T. ) ;
#33352 = ORIENTED_EDGE ( 'NONE', *, *, #11516, .F. ) ;
#33353 = AXIS2_PLACEMENT_3D ( 'NONE', #40785, #47875, #18259 ) ;
#33354 = CARTESIAN_POINT ( 'NONE',  ( 12.00000000000000000, -13.04903810567675393, -19.60159698893424718 ) ) ;
#33355 = VERTEX_POINT ( 'NONE', #32772 ) ;
#33356 = DIRECTION ( 'NONE',  ( 0.000000000000000000, 0.9723699203976756689, 0.2334453638559095268 ) ) ;
#33357 = CARTESIAN_POINT ( 'NONE',  ( 0.09268126076924407264, 0.8248091802970087816, 42.00000000000001421 ) ) ;
#33358 = AXIS2_PLACEMENT_3D ( 'NONE', #8827, #20097, #16198 ) ;
#33359 = CARTESIAN_POINT ( 'NONE',  ( 10.00000000000000000, 0.000000000000000000, 0.000000000000000000 ) ) ;
#33360 = EDGE_LOOP ( 'NONE', ( #18841, #35667, #47204, #12115 ) ) ;
#33361 = EDGE_CURVE ( 'NONE', #11716, #22548, #32461, .T. ) ;
#33362 = AXIS2_PLACEMENT_3D ( 'NONE', #10833, #6438, #47070 ) ;
#33363 = ORIENTED_EDGE ( 'NONE', *, *, #13836, .T. ) ;
#33364 = EDGE_CURVE ( 'NONE', #30385, #37478, #39519, .T. ) ;
#33365 = CYLINDRICAL_SURFACE ( 'NONE', #22249, 77.49899999999999523 ) ;
#33366 = EDGE_LOOP ( 'NONE', ( #14272, #32866, #12712, #38669 ) ) ;
#33367 = VECTOR ( 'NONE', #47651, 1000.000000000000000 ) ;
#33368 = EDGE_CURVE ( 'NONE', #11531, #48354, #872, .T. ) ;
#33369 = AXIS2_PLACEMENT_3D ( 'NONE', #44425, #4035, #18941 ) ;
#33370 = FACE_OUTER_BOUND ( 'NONE', #32543, .T. ) ;
#33371 = VERTEX_POINT ( 'NONE', #35132 ) ;
#33372 = PLANE ( 'NONE',  #8598 ) ;
#33373 = CARTESIAN_POINT ( 'NONE',  ( 5.999999999999999112, 81.96053171279902472, 2.543863470248677316 ) ) ;
#33374 = EDGE_LOOP ( 'NONE', ( #4141, #5097, #28459, #34710 ) ) ;
#33375 = DIRECTION ( 'NONE',  ( 1.000000000000000000, -0.000000000000000000, -0.000000000000000000 ) ) ;
#33376 = EDGE_CURVE ( 'NONE', #7935, #5492, #45930, .T. ) ;
#33377 = ORIENTED_EDGE ( 'NONE', *, *, #45379, .T. ) ;
#33378 = EDGE_CURVE ( 'NONE', #47615, #14593, #15821, .T. ) ;
#33379 = EDGE_CURVE ( 'NONE', #23020, #35449, #8955, .T. ) ;
#33380 = AXIS2_PLACEMENT_3D ( 'NONE', #15298, #7926, #26304 ) ;
#33381 = CARTESIAN_POINT ( 'NONE',  ( 0.000000000000000000, 6.736453364084091788, -36.88895765772625879 ) ) ;
#33382 = DIRECTION ( 'NONE',  ( 1.000000000000000000, 0.000000000000000000, 0.000000000000000000 ) ) ;
#33383 = DIRECTION ( 'NONE',  ( -1.000000000000000000, 0.000000000000000000, 0.000000000000000000 ) ) ;
#33385 = DIRECTION ( 'NONE',  ( 0.000000000000000000, 0.000000000000000000, 1.000000000000000000 ) ) ;
#33384 = CIRCLE ( 'NONE', #22462, 42.00000000000000000 ) ;
#33386 = ORIENTED_EDGE ( 'NONE', *, *, #8668, .F. ) ;
#33387 = CARTESIAN_POINT ( 'NONE',  ( 0.000000000000000000, -22.67460108101783334, 6.353146135317912169 ) ) ;
#33388 = VERTEX_POINT ( 'NONE', #12397 ) ;
#33389 = EDGE_LOOP ( 'NONE', ( #1592, #17760, #13518, #32966 ) ) ;
#33390 = CARTESIAN_POINT ( 'NONE',  ( 0.000000000000000000, 6.555932627142952995, -37.01155633439051940 ) ) ;
#33391 = CYLINDRICAL_SURFACE ( 'NONE', #20732, 16.00000000000000000 ) ;
#33392 = ADVANCED_FACE ( 'NONE', ( #45677 ), #16543, .T. ) ;
#33393 = LINE ( 'NONE', #44645, #27501 ) ;
#33394 = CARTESIAN_POINT ( 'NONE',  ( 10.00000000000000000, -6.555932627142676772, 37.01155633439056203 ) ) ;
#33395 = ORIENTED_EDGE ( 'NONE', *, *, #40882, .T. ) ;
#33396 = DIRECTION ( 'NONE',  ( 0.1276937514489679404, 0.9918136447140103451, 0.000000000000000000 ) ) ;
#33397 = CARTESIAN_POINT ( 'NONE',  ( 0.000000000000000000, -0.8299999999999999600, -1.199999999999999956 ) ) ;
#33398 = DIRECTION ( 'NONE',  ( 0.9580045777625458836, 0.2867529058022011412, -0.000000000000000000 ) ) ;
#33399 = DIRECTION ( 'NONE',  ( 0.000000000000000000, -0.7071067811865389130, -0.7071067811865563435 ) ) ;
#33400 = DIRECTION ( 'NONE',  ( 0.000000000000000000, -0.6494480483301904306, 0.7604059656000252687 ) ) ;
#33401 = AXIS2_PLACEMENT_3D ( 'NONE', #26847, #11683, #34187 ) ;
#33402 = DIRECTION ( 'NONE',  ( -1.000000000000000000, 0.000000000000000000, 0.000000000000000000 ) ) ;
#33403 = ORIENTED_EDGE ( 'NONE', *, *, #34271, .F. ) ;
#33404 = DIRECTION ( 'NONE',  ( 0.000000000000000000, 0.000000000000000000, -1.000000000000000000 ) ) ;
#33405 = DIRECTION ( 'NONE',  ( -1.000000000000000000, -0.000000000000000000, -0.000000000000000000 ) ) ;
#33406 = DIRECTION ( 'NONE',  ( 0.000000000000000000, 0.000000000000000000, 1.000000000000000000 ) ) ;
#33407 = CARTESIAN_POINT ( 'NONE',  ( -17.26469406256017791, -140.1601175325492648, -2.500000000000000444 ) ) ;
#33408 = CARTESIAN_POINT ( 'NONE',  ( 0.000000000000000000, 0.000000000000000000, 0.000000000000000000 ) ) ;
#33409 = VECTOR ( 'NONE', #11138, 1000.000000000000114 ) ;
#33410 = ORIENTED_EDGE ( 'NONE', *, *, #13818, .T. ) ;
#33411 = CARTESIAN_POINT ( 'NONE',  ( 0.000000000000000000, 0.000000000000000000, 0.000000000000000000 ) ) ;
#33412 = CARTESIAN_POINT ( 'NONE',  ( 10.00000000000000000, 0.000000000000000000, 0.000000000000000000 ) ) ;
#33413 = DIRECTION ( 'NONE',  ( 0.000000000000000000, 0.000000000000000000, 1.000000000000000000 ) ) ;
#33414 = DIRECTION ( 'NONE',  ( -0.000000000000000000, -0.000000000000000000, -1.000000000000000000 ) ) ;
#33415 = DIRECTION ( 'NONE',  ( 0.000000000000000000, 0.000000000000000000, 1.000000000000000000 ) ) ;
#33416 = ORIENTED_EDGE ( 'NONE', *, *, #43215, .T. ) ;
#33417 = EDGE_CURVE ( 'NONE', #28552, #18377, #19162, .T. ) ;
#33418 = CIRCLE ( 'NONE', #44386, 77.49899999999999523 ) ;
#33419 = EDGE_CURVE ( 'NONE', #34570, #12619, #42744, .T. ) ;
#33420 = ORIENTED_EDGE ( 'NONE', *, *, #34778, .T. ) ;
#33421 = ADVANCED_FACE ( 'NONE', ( #31489 ), #9199, .F. ) ;
#33422 = AXIS2_PLACEMENT_3D ( 'NONE', #23405, #40225, #25261 ) ;
#33423 = DIRECTION ( 'NONE',  ( 0.000000000000000000, -0.1564344650402170744, -0.9876883405951399908 ) ) ;
#33424 = EDGE_LOOP ( 'NONE', ( #18549, #44045, #24187, #4117 ) ) ;
#33425 = ADVANCED_FACE ( 'NONE', ( #20442 ), #23635, .T. ) ;
#33426 = VECTOR ( 'NONE', #8251, 1000.000000000000000 ) ;
#33427 = DIRECTION ( 'NONE',  ( 0.000000000000000000, -0.5877852522924797984, 0.8090169943749426773 ) ) ;
#33428 = CARTESIAN_POINT ( 'NONE',  ( 10.00000000000000000, -17.28742895386031719, -75.54627589209962935 ) ) ;
#33429 = PLANE ( 'NONE',  #28499 ) ;
#33430 = VERTEX_POINT ( 'NONE', #1125 ) ;
#33431 = CARTESIAN_POINT ( 'NONE',  ( 50.00005079999999680, 0.000000000000000000, 0.000000000000000000 ) ) ;
#33432 = ORIENTED_EDGE ( 'NONE', *, *, #47922, .F. ) ;
#33433 = ORIENTED_EDGE ( 'NONE', *, *, #3912, .T. ) ;
#33434 = ORIENTED_EDGE ( 'NONE', *, *, #38478, .T. ) ;
#33435 = EDGE_CURVE ( 'NONE', #41033, #23667, #27819, .T. ) ;
#33436 = EDGE_CURVE ( 'NONE', #648, #27310, #44964, .T. ) ;
#33437 = CARTESIAN_POINT ( 'NONE',  ( 0.000000000000000000, 0.000000000000000000, 0.000000000000000000 ) ) ;
#33438 = DIRECTION ( 'NONE',  ( -1.000000000000000000, 0.000000000000000000, 0.000000000000000000 ) ) ;
#33439 = FACE_OUTER_BOUND ( 'NONE', #19828, .T. ) ;
#33440 = ORIENTED_EDGE ( 'NONE', *, *, #4538, .F. ) ;
#33441 = VERTEX_POINT ( 'NONE', #34395 ) ;
#33442 = DIRECTION ( 'NONE',  ( -1.000000000000000000, -0.000000000000000000, -0.000000000000000000 ) ) ;
#33443 = ORIENTED_EDGE ( 'NONE', *, *, #43976, .T. ) ;
#33444 = CYLINDRICAL_SURFACE ( 'NONE', #21483, 16.00000000000000000 ) ;
#33445 = DIRECTION ( 'NONE',  ( 0.000000000000000000, 0.000000000000000000, 1.000000000000000000 ) ) ;
#33446 = CARTESIAN_POINT ( 'NONE',  ( -24.94940289813038703, -237.3777120880567963, 5.500000000000000000 ) ) ;
#33447 = DIRECTION ( 'NONE',  ( 0.000000000000000000, -0.1564344650402382242, 0.9876883405951366601 ) ) ;
#33448 = CARTESIAN_POINT ( 'NONE',  ( 12.00000000000000000, -11.95096189432345746, -23.69967320028757030 ) ) ;
#33449 = DIRECTION ( 'NONE',  ( 0.000000000000000000, 0.000000000000000000, 1.000000000000000000 ) ) ;
#33450 = LINE ( 'NONE', #148, #20172 ) ;
#33451 = FILL_AREA_STYLE_COLOUR ( '', #24229 ) ;
#33453 = EDGE_CURVE ( 'NONE', #9220, #24955, #9006, .T. ) ;
#33452 = LINE ( 'NONE', #14625, #33184 ) ;
#33454 = EDGE_LOOP ( 'NONE', ( #41062, #43082, #28381, #21242 ) ) ;
#33455 = CYLINDRICAL_SURFACE ( 'NONE', #14985, 16.00000000000000000 ) ;
#33456 = VECTOR ( 'NONE', #18987, 1000.000000000000227 ) ;
#33457 = ORIENTED_EDGE ( 'NONE', *, *, #4690, .F. ) ;
#33458 = CARTESIAN_POINT ( 'NONE',  ( -3.000000000000000000, -10.45096189432344147, 21.10159698893426494 ) ) ;
#33459 = VECTOR ( 'NONE', #43880, 1000.000000000000000 ) ;
#33460 = DIRECTION ( 'NONE',  ( 1.000000000000000000, -0.000000000000000000, 0.000000000000000000 ) ) ;
#33461 = CARTESIAN_POINT ( 'NONE',  ( 4.999999999999999112, 21.40280677340371795, 36.13751322684426270 ) ) ;
#33462 = CARTESIAN_POINT ( 'NONE',  ( 0.000000000000000000, -0.6853352020793173072, 37.58145647212453611 ) ) ;
#33463 = DIRECTION ( 'NONE',  ( -1.000000000000000000, 0.000000000000000000, -0.000000000000000000 ) ) ;
#33464 = CARTESIAN_POINT ( 'NONE',  ( 10.00000000000000000, 37.48860685352291000, 0.8828120875901893649 ) ) ;
#33465 = DIRECTION ( 'NONE',  ( -1.000000000000000000, 0.000000000000000000, 0.000000000000000000 ) ) ;
#33466 = DIRECTION ( 'NONE',  ( 0.000000000000000000, 0.000000000000000000, 1.000000000000000000 ) ) ;
#33467 = DIRECTION ( 'NONE',  ( -0.000000000000000000, -0.000000000000000000, -1.000000000000000000 ) ) ;
#33468 = DIRECTION ( 'NONE',  ( 0.000000000000000000, 0.000000000000000000, 1.000000000000000000 ) ) ;
#33469 = ORIENTED_EDGE ( 'NONE', *, *, #1799, .T. ) ;
#33470 = VERTEX_POINT ( 'NONE', #1380 ) ;
#33471 = AXIS2_PLACEMENT_3D ( 'NONE', #29045, #22437, #10447 ) ;
#33472 = ADVANCED_FACE ( 'NONE', ( #16307 ), #31246, .F. ) ;
#33473 = ORIENTED_EDGE ( 'NONE', *, *, #44642, .F. ) ;
#33474 = CARTESIAN_POINT ( 'NONE',  ( 0.000000000000000000, -72.35432306680469594, -20.40083707022958848 ) ) ;
#33475 = DIRECTION ( 'NONE',  ( -1.000000000000000000, 0.000000000000000000, 0.000000000000000000 ) ) ;
#33476 = VERTEX_POINT ( 'NONE', #39060 ) ;
#33477 = EDGE_CURVE ( 'NONE', #20327, #23602, #13121, .T. ) ;
#33478 = LINE ( 'NONE', #34430, #43692 ) ;
#33479 = COLOUR_RGB ( '', 0.72549020, 0.75294118, 0.79215686) ;
#33480 = ORIENTED_EDGE ( 'NONE', *, *, #32822, .F. ) ;
#33481 = EDGE_LOOP ( 'NONE', ( #21738, #19685, #6857, #47078 ) ) ;
#33482 = AXIS2_PLACEMENT_3D ( 'NONE', #27305, #5753, #5027 ) ;
#33483 = EDGE_CURVE ( 'NONE', #46110, #22787, #31741, .T. ) ;
#33484 = ADVANCED_FACE ( 'NONE', ( #9426 ), #24360, .F. ) ;
#33485 = ORIENTED_EDGE ( 'NONE', *, *, #4958, .F. ) ;
#33486 = CARTESIAN_POINT ( 'NONE',  ( 0.000000000000000000, -33.80338159004273280, -16.23288003029533044 ) ) ;
#33487 = ORIENTED_EDGE ( 'NONE', *, *, #24309, .T. ) ;
#33488 = CARTESIAN_POINT ( 'NONE',  ( 0.000000000000000000, 0.000000000000000000, 0.000000000000000000 ) ) ;
#33489 = EDGE_CURVE ( 'NONE', #6565, #21764, #29374, .T. ) ;
#33490 = ORIENTED_EDGE ( 'NONE', *, *, #26072, .F. ) ;
#33491 = FACE_OUTER_BOUND ( 'NONE', #30394, .T. ) ;
#33492 = DIRECTION ( 'NONE',  ( 0.000000000000000000, -0.9510565162951500895, -0.3090169943749583314 ) ) ;
#33493 = CARTESIAN_POINT ( 'NONE',  ( 0.000000000000000000, -70.53064760720297954, -26.01480285779911839 ) ) ;
#33494 = ORIENTED_EDGE ( 'NONE', *, *, #39115, .F. ) ;
#33495 = ORIENTED_EDGE ( 'NONE', *, *, #34557, .F. ) ;
#33496 = CIRCLE ( 'NONE', #42884, 15.99999999999999822 ) ;
#33497 = CARTESIAN_POINT ( 'NONE',  ( 11.99999999999999822, 0.000000000000000000, 0.000000000000000000 ) ) ;
#33498 = EDGE_CURVE ( 'NONE', #7846, #29919, #12197, .T. ) ;
#33499 = DIRECTION ( 'NONE',  ( -1.000000000000000000, 0.000000000000000000, 0.000000000000000000 ) ) ;
#33500 = EDGE_LOOP ( 'NONE', ( #26609, #24576, #24785, #28088 ) ) ;
#33501 = ORIENTED_EDGE ( 'NONE', *, *, #16521, .F. ) ;
#33502 = CYLINDRICAL_SURFACE ( 'NONE', #18952, 82.00000000000000000 ) ;
#33503 = CARTESIAN_POINT ( 'NONE',  ( 0.000000000000000000, 63.97538442413426907, 51.29473840253247374 ) ) ;
#33504 = ORIENTED_EDGE ( 'NONE', *, *, #15539, .T. ) ;
#33505 = DIRECTION ( 'NONE',  ( -1.000000000000000000, 0.000000000000000000, -0.000000000000000000 ) ) ;
#33506 = LINE ( 'NONE', #37186, #37925 ) ;
#33507 = CARTESIAN_POINT ( 'NONE',  ( -10.00000000000000000, 0.000000000000000000, 0.000000000000000000 ) ) ;
#33508 = PLANE ( 'NONE',  #3429 ) ;
#33509 = CARTESIAN_POINT ( 'NONE',  ( 10.00000000000000000, -37.01155633439063308, 6.555932627142289526 ) ) ;
#33510 = DIRECTION ( 'NONE',  ( 0.1276937514489679404, 0.9918136447140103451, -0.000000000000000000 ) ) ;
#33511 = CARTESIAN_POINT ( 'NONE',  ( 0.000000000000000000, 74.65374052328660071, -8.840884882374309583 ) ) ;
#33512 = LINE ( 'NONE', #15891, #31798 ) ;
#33513 = VECTOR ( 'NONE', #14465, 1000.000000000000000 ) ;
#33514 = PLANE ( 'NONE',  #38738 ) ;
#33515 = CIRCLE ( 'NONE', #35096, 11.59999999999999787 ) ;
#33516 = CARTESIAN_POINT ( 'NONE',  ( 5.999999999999999112, 40.65526001592713357, -71.21200624218752750 ) ) ;
#33517 = CYLINDRICAL_SURFACE ( 'NONE', #26933, 42.00000000000000000 ) ;
#33519 = CIRCLE ( 'NONE', #43697, 32.50000000000000000 ) ;
#33518 =( LENGTH_UNIT ( ) NAMED_UNIT ( * ) SI_UNIT ( .MILLI., .METRE. ) );
#33520 = FACE_OUTER_BOUND ( 'NONE', #42093, .T. ) ;
#33521 = ORIENTED_EDGE ( 'NONE', *, *, #8913, .T. ) ;
#33522 = VERTEX_POINT ( 'NONE', #43929 ) ;
#33523 = UNCERTAINTY_MEASURE_WITH_UNIT (LENGTH_MEASURE( 1.000000000000000082E-05 ), #40232, 'distance_accuracy_value', 'NONE');
#33524 = EDGE_CURVE ( 'NONE', #24727, #36078, #9923, .T. ) ;
#33525 = CARTESIAN_POINT ( 'NONE',  ( 11.99999999999999822, 0.000000000000000000, 0.000000000000000000 ) ) ;
#33526 = EDGE_CURVE ( 'NONE', #24182, #20061, #18433, .T. ) ;
#33527 = DIRECTION ( 'NONE',  ( -0.000000000000000000, -0.000000000000000000, 1.000000000000000000 ) ) ;
#33528 = DIRECTION ( 'NONE',  ( -1.000000000000000000, 0.000000000000000000, 0.000000000000000000 ) ) ;
#33529 = ADVANCED_FACE ( 'NONE', ( #28766 ), #14314, .T. ) ;
#33530 = EDGE_LOOP ( 'NONE', ( #18846, #11054, #35409, #13052 ) ) ;
#33531 = EDGE_CURVE ( 'NONE', #25033, #7137, #24848, .T. ) ;
#33532 = MECHANICAL_DESIGN_GEOMETRIC_PRESENTATION_REPRESENTATION (  '', ( #42921 ), #35881 ) ;
#33533 = EDGE_CURVE ( 'NONE', #15851, #8001, #10617, .T. ) ;
#33534 = EDGE_CURVE ( 'NONE', #17233, #19561, #2809, .T. ) ;
#33535 = EDGE_CURVE ( 'NONE', #34289, #11599, #440, .T. ) ;
#33536 = CARTESIAN_POINT ( 'NONE',  ( 0.000000000000000000, 0.000000000000000000, 0.000000000000000000 ) ) ;
#33537 = ORIENTED_EDGE ( 'NONE', *, *, #27129, .F. ) ;
#33538 = VERTEX_POINT ( 'NONE', #10653 ) ;
#33539 = VERTEX_POINT ( 'NONE', #25316 ) ;
#33540 = ORIENTED_EDGE ( 'NONE', *, *, #11724, .T. ) ;
#33541 = CYLINDRICAL_SURFACE ( 'NONE', #23008, 82.00000000000000000 ) ;
#33542 = CIRCLE ( 'NONE', #8529, 20.64000000000000057 ) ;
#33543 = CARTESIAN_POINT ( 'NONE',  ( 4.999999999999999112, 10.41901085202078292, 40.68715046381932865 ) ) ;
#33545 = ORIENTED_EDGE ( 'NONE', *, *, #24819, .F. ) ;
#33544 = AXIS2_PLACEMENT_3D ( 'NONE', #17107, #16388, #9049 ) ;
#33546 = EDGE_CURVE ( 'NONE', #4028, #14988, #3551, .T. ) ;
#33547 = VERTEX_POINT ( 'NONE', #36583 ) ;
#33548 = CARTESIAN_POINT ( 'NONE',  ( 11.99999999999999822, 14.67089635893819377, -73.72996012237423713 ) ) ;
#33549 = ORIENTED_EDGE ( 'NONE', *, *, #7008, .F. ) ;
#33550 = AXIS2_PLACEMENT_3D ( 'NONE', #47913, #44259, #25640 ) ;
#33551 = DIRECTION ( 'NONE',  ( 1.000000000000000000, 0.000000000000000000, 0.000000000000000000 ) ) ;
#33552 = DIRECTION ( 'NONE',  ( -0.000000000000000000, -0.000000000000000000, -1.000000000000000000 ) ) ;
#33553 = ORIENTED_EDGE ( 'NONE', *, *, #43894, .T. ) ;
#33554 = DIRECTION ( 'NONE',  ( 0.000000000000000000, 0.000000000000000000, 1.000000000000000000 ) ) ;
#33555 = DIRECTION ( 'NONE',  ( -1.000000000000000000, -0.000000000000000000, -0.000000000000000000 ) ) ;
#33556 = ORIENTED_EDGE ( 'NONE', *, *, #23832, .T. ) ;
#33558 = VERTEX_POINT ( 'NONE', #40275 ) ;
#33557 = DIRECTION ( 'NONE',  ( 0.000000000000000000, -0.8526401643540860720, -0.5224985647159590130 ) ) ;
#33559 = EDGE_CURVE ( 'NONE', #32964, #11808, #44226, .T. ) ;
#33560 = PLANE ( 'NONE',  #30555 ) ;
#33561 = ORIENTED_EDGE ( 'NONE', *, *, #9033, .T. ) ;
#33562 = DIRECTION ( 'NONE',  ( 0.000000000000000000, 0.3090169943749482839, -0.9510565162951533091 ) ) ;
#33563 = EDGE_LOOP ( 'NONE', ( #40276, #13739, #5139, #2940 ) ) ;
#33564 = CIRCLE ( 'NONE', #1532, 31.99999999999998224 ) ;
#33565 = ORIENTED_EDGE ( 'NONE', *, *, #20177, .T. ) ;
#33566 = CARTESIAN_POINT ( 'NONE',  ( 10.00000000000000000, 25.88420570971438650, -27.13269053701069566 ) ) ;
#33567 = CARTESIAN_POINT ( 'NONE',  ( 0.000000000000000000, 6.762365576493310826, 25.66652317338401090 ) ) ;
#33568 = DIRECTION ( 'NONE',  ( 0.000000000000000000, 0.000000000000000000, 1.000000000000000000 ) ) ;
#33569 = PLANE ( 'NONE',  #24271 ) ;
#33570 = CARTESIAN_POINT ( 'NONE',  ( 0.000000000000000000, 0.000000000000000000, 0.000000000000000000 ) ) ;
#33571 = EDGE_CURVE ( 'NONE', #20008, #28171, #32902, .T. ) ;
#33572 = CARTESIAN_POINT ( 'NONE',  ( 10.00000000000000000, 0.000000000000000000, 0.000000000000000000 ) ) ;
#33573 = DIRECTION ( 'NONE',  ( 0.000000000000000000, -0.7431448254773954654, -0.6691306063588569053 ) ) ;
#33574 = DIRECTION ( 'NONE',  ( 0.000000000000000000, 0.000000000000000000, 1.000000000000000000 ) ) ;
#33575 = EDGE_CURVE ( 'NONE', #17439, #14824, #5945, .T. ) ;
#33576 = CARTESIAN_POINT ( 'NONE',  ( 0.000000000000000000, -14.54903810567645372, -22.19967320028775504 ) ) ;
#33577 = DIRECTION ( 'NONE',  ( -1.000000000000000000, 0.000000000000000000, 0.000000000000000000 ) ) ;
#33578 = LINE ( 'NONE', #4217, #13103 ) ;
#33579 = DIRECTION ( 'NONE',  ( -1.000000000000000000, -0.000000000000000000, -0.000000000000000000 ) ) ;
#33580 = CARTESIAN_POINT ( 'NONE',  ( -10.00000000000000000, 0.000000000000000000, 0.000000000000000000 ) ) ;
#33581 = FACE_OUTER_BOUND ( 'NONE', #13962, .T. ) ;
#33582 = DIRECTION ( 'NONE',  ( -1.000000000000000000, 0.000000000000000000, 0.000000000000000000 ) ) ;
#33583 = LINE ( 'NONE', #6689, #24115 ) ;
#33584 = ORIENTED_EDGE ( 'NONE', *, *, #18765, .F. ) ;
#33585 = EDGE_CURVE ( 'NONE', #6004, #1147, #17247, .T. ) ;
#33586 = VECTOR ( 'NONE', #43343, 1000.000000000000000 ) ;
#33587 = CARTESIAN_POINT ( 'NONE',  ( 10.00000000000000000, -76.66974797899830207, -11.30684508768422170 ) ) ;
#33588 = CIRCLE ( 'NONE', #32042, 15.99999999999999645 ) ;
#33589 = ORIENTED_EDGE ( 'NONE', *, *, #3709, .F. ) ;
#33590 = EDGE_CURVE ( 'NONE', #36506, #20061, #45810, .T. ) ;
#33591 = DIRECTION ( 'NONE',  ( -1.000000000000000000, 0.000000000000000000, -0.000000000000000000 ) ) ;
#33592 = VECTOR ( 'NONE', #31644, 1000.000000000000000 ) ;
#33593 = DIRECTION ( 'NONE',  ( 0.000000000000000000, 0.000000000000000000, 0.9999999999999998890 ) ) ;
#33594 = ADVANCED_FACE ( 'NONE', ( #35630 ), #46891, .T. ) ;
#33595 = FACE_OUTER_BOUND ( 'NONE', #21282, .T. ) ;
#33596 = VERTEX_POINT ( 'NONE', #28530 ) ;
#33597 = CIRCLE ( 'NONE', #20303, 16.00000000000000000 ) ;
#33598 = EDGE_CURVE ( 'NONE', #20241, #21733, #43466, .T. ) ;
#33599 = CARTESIAN_POINT ( 'NONE',  ( 11.99999999999999822, -79.10210256391381733, 21.60688246758557796 ) ) ;
#33600 = ORIENTED_EDGE ( 'NONE', *, *, #3472, .T. ) ;
#33601 = FACE_OUTER_BOUND ( 'NONE', #11526, .T. ) ;
#33602 = DIRECTION ( 'NONE',  ( 1.000000000000000000, 0.000000000000000000, -0.000000000000000000 ) ) ;
#33604 = ORIENTED_EDGE ( 'NONE', *, *, #5996, .F. ) ;
#33603 = DIRECTION ( 'NONE',  ( 1.000000000000000000, -0.000000000000000000, -0.000000000000000000 ) ) ;
#33605 = ORIENTED_EDGE ( 'NONE', *, *, #12412, .F. ) ;
#33606 = ORIENTED_EDGE ( 'NONE', *, *, #16700, .T. ) ;
#33607 = CYLINDRICAL_SURFACE ( 'NONE', #26926, 77.49899999999999523 ) ;
#33608 = CARTESIAN_POINT ( 'NONE',  ( 0.000000000000000000, 55.19960302592141232, -51.03279382321027668 ) ) ;
#33609 = CARTESIAN_POINT ( 'NONE',  ( 0.000000000000000000, 0.000000000000000000, 0.000000000000000000 ) ) ;
#33610 = CIRCLE ( 'NONE', #12531, 82.00000000000000000 ) ;
#33611 = FACE_OUTER_BOUND ( 'NONE', #43651, .T. ) ;
#33612 = ORIENTED_EDGE ( 'NONE', *, *, #12044, .T. ) ;
#33613 = FACE_OUTER_BOUND ( 'NONE', #5078, .T. ) ;
#33614 = VERTEX_POINT ( 'NONE', #36817 ) ;
#33615 = EDGE_LOOP ( 'NONE', ( #29892, #31645, #13464, #7573 ) ) ;
#33616 = DIRECTION ( 'NONE',  ( 1.000000000000000000, -0.000000000000000000, -0.000000000000000000 ) ) ;
#33617 = CIRCLE ( 'NONE', #23353, 31.99999999999999645 ) ;
#33618 = CARTESIAN_POINT ( 'NONE',  ( -21.67772167707813935, -110.8034581014852762, 5.500000000000000000 ) ) ;
#33619 = DIRECTION ( 'NONE',  ( -1.000000000000000000, -0.000000000000000000, -0.000000000000000000 ) ) ;
#33620 = CARTESIAN_POINT ( 'NONE',  ( 10.00000000000000000, 75.11725578898467859, 2.956366410620910656 ) ) ;
#33621 = ORIENTED_EDGE ( 'NONE', *, *, #21441, .F. ) ;
#33622 = CARTESIAN_POINT ( 'NONE',  ( 10.00000000000000000, 30.84782396557218931, 21.32104025579126017 ) ) ;
#33623 = DIRECTION ( 'NONE',  ( -0.000000000000000000, -0.000000000000000000, -1.000000000000000000 ) ) ;
#33624 = MECHANICAL_DESIGN_GEOMETRIC_PRESENTATION_REPRESENTATION (  '', ( #5505 ), #6282 ) ;
#33625 = LINE ( 'NONE', #10881, #25851 ) ;
#33626 = CIRCLE ( 'NONE', #17305, 11.59999999999999787 ) ;
#33627 = DIRECTION ( 'NONE',  ( 1.000000000000000000, 0.000000000000000000, 0.000000000000000000 ) ) ;
#33628 = CARTESIAN_POINT ( 'NONE',  ( 11.99999999999999822, 0.000000000000000000, 0.000000000000000000 ) ) ;
#33629 = CIRCLE ( 'NONE', #29720, 77.49899999999999523 ) ;
#33630 = LINE ( 'NONE', #2383, #17576 ) ;
#33631 = CARTESIAN_POINT ( 'NONE',  ( -20.30386590532155111, -102.9045904027214959, -2.500000000000000000 ) ) ;
#33632 = CARTESIAN_POINT ( 'NONE',  ( -3.000000000000000000, -3.948201729842348850, 23.21447184625293048 ) ) ;
#33633 = DIRECTION ( 'NONE',  ( 0.000000000000000000, 0.000000000000000000, 1.000000000000000000 ) ) ;
#33634 = CARTESIAN_POINT ( 'NONE',  ( -1.250000000000000444, -16.78109714094927085, -1.199999999999999956 ) ) ;
#33635 = DIRECTION ( 'NONE',  ( 0.000000000000000000, 0.000000000000000000, 1.000000000000000000 ) ) ;
#33636 = VERTEX_POINT ( 'NONE', #30222 ) ;
#33637 = DIRECTION ( 'NONE',  ( -1.000000000000000000, -0.000000000000000000, 0.000000000000000000 ) ) ;
#33638 = DIRECTION ( 'NONE',  ( 0.000000000000000000, 0.000000000000000000, 1.000000000000000000 ) ) ;
#33639 = CARTESIAN_POINT ( 'NONE',  ( 11.99999999999999822, 51.29473840253317007, -63.97538442413369353 ) ) ;
#33640 = FACE_OUTER_BOUND ( 'NONE', #12433, .T. ) ;
#33641 = ADVANCED_FACE ( 'NONE', ( #18929 ), #343, .T. ) ;
#33642 = LINE ( 'NONE', #44669, #18946 ) ;
#33643 = ORIENTED_EDGE ( 'NONE', *, *, #44687, .F. ) ;
#33644 = EDGE_CURVE ( 'NONE', #5621, #29354, #4370, .T. ) ;
#33645 = VECTOR ( 'NONE', #41468, 1000.000000000000114 ) ;
#33646 = VECTOR ( 'NONE', #12317, 1000.000000000000000 ) ;
#33647 = EDGE_CURVE ( 'NONE', #40057, #9769, #1216, .T. ) ;
#33648 = AXIS2_PLACEMENT_3D ( 'NONE', #14250, #40208, #29166 ) ;
#33649 = AXIS2_PLACEMENT_3D ( 'NONE', #19094, #41619, #38193 ) ;
#33650 = ADVANCED_FACE ( 'NONE', ( #48322 ), #45143, .F. ) ;
#33651 = DIRECTION ( 'NONE',  ( 0.000000000000000000, -0.3826834323650774028, -0.9238795325112919565 ) ) ;
#33652 = VERTEX_POINT ( 'NONE', #15521 ) ;
#33653 = AXIS2_PLACEMENT_3D ( 'NONE', #9301, #1485, #16412 ) ;
#33654 = VECTOR ( 'NONE', #38771, 1000.000000000000000 ) ;
#33655 = CARTESIAN_POINT ( 'NONE',  ( 10.00000000000000000, 36.13751322684449718, -21.40280677340333071 ) ) ;
#33656 = CIRCLE ( 'NONE', #39931, 82.00000000000000000 ) ;
#33657 = LINE ( 'NONE', #123, #41384 ) ;
#33658 = CARTESIAN_POINT ( 'NONE',  ( 10.00000000000000000, 0.000000000000000000, 0.000000000000000000 ) ) ;
#33659 = ORIENTED_EDGE ( 'NONE', *, *, #10799, .T. ) ;
#33660 = DIRECTION ( 'NONE',  ( 0.000000000000000000, 0.000000000000000000, 1.000000000000000000 ) ) ;
#33661 = ORIENTED_EDGE ( 'NONE', *, *, #34080, .T. ) ;
#33662 = ORIENTED_EDGE ( 'NONE', *, *, #22653, .F. ) ;
#33663 = EDGE_LOOP ( 'NONE', ( #9458, #33671, #1353, #24223 ) ) ;
#33664 = CYLINDRICAL_SURFACE ( 'NONE', #22564, 77.49899999999999523 ) ;
#33665 = CARTESIAN_POINT ( 'NONE',  ( 5.000000000000000000, -16.65560815589439159, 38.55633173627004595 ) ) ;
#33666 = LINE ( 'NONE', #3575, #1660 ) ;
#33667 = VERTEX_POINT ( 'NONE', #30452 ) ;
#33668 = EDGE_LOOP ( 'NONE', ( #19406, #11894, #2897, #46922 ) ) ;
#33669 = ORIENTED_EDGE ( 'NONE', *, *, #22153, .F. ) ;
#33670 = CARTESIAN_POINT ( 'NONE',  ( -10.00000000000000000, 0.000000000000000000, 0.000000000000000000 ) ) ;
#33671 = ORIENTED_EDGE ( 'NONE', *, *, #27370, .F. ) ;
#33672 = DIRECTION ( 'NONE',  ( -1.000000000000000000, -0.000000000000000000, 0.000000000000000000 ) ) ;
#33673 = FACE_OUTER_BOUND ( 'NONE', #29291, .T. ) ;
#33674 = DIRECTION ( 'NONE',  ( 0.000000000000000000, -0.9510565162951566398, 0.3090169943749381809 ) ) ;
#33675 = DIRECTION ( 'NONE',  ( 0.7950889364178798102, -0.6064928550163511956, 0.000000000000000000 ) ) ;
#33676 = DIRECTION ( 'NONE',  ( 0.000000000000000000, -0.7071067811865389130, -0.7071067811865561215 ) ) ;
#33677 = DIRECTION ( 'NONE',  ( -1.000000000000000000, -0.000000000000000000, 0.000000000000000000 ) ) ;
#33678 = DIRECTION ( 'NONE',  ( 0.000000000000000000, -0.8660254037844374864, 0.5000000000000019984 ) ) ;
#33680 = ADVANCED_FACE ( 'NONE', ( #37065 ), #26049, .F. ) ;
#33679 = EDGE_LOOP ( 'NONE', ( #47500, #33888, #35838, #24128 ) ) ;
#33681 = CARTESIAN_POINT ( 'NONE',  ( 6.000000000000000000, 80.55351364060589958, 15.33399622253512540 ) ) ;
#33682 = CARTESIAN_POINT ( 'NONE',  ( 0.000000000000000000, 16.00000000000000000, 2.500000000000000000 ) ) ;
#33683 = EDGE_LOOP ( 'NONE', ( #2256, #40525, #6735, #43727 ) ) ;
#33684 = CIRCLE ( 'NONE', #31374, 31.99999999999998934 ) ;
#33685 = CARTESIAN_POINT ( 'NONE',  ( 11.99999999999999822, 0.000000000000000000, 0.000000000000000000 ) ) ;
#33686 = EDGE_CURVE ( 'NONE', #35257, #2423, #14800, .T. ) ;
#33687 = EDGE_LOOP ( 'NONE', ( #46800, #45727, #2921, #27289 ) ) ;
#33688 = AXIS2_PLACEMENT_3D ( 'NONE', #42282, #43251, #28316 ) ;
#33689 = DIRECTION ( 'NONE',  ( 0.000000000000000000, 0.4539904997395477482, -0.8910065241883674547 ) ) ;
#33690 = VECTOR ( 'NONE', #18744, 1000.000000000000000 ) ;
#33691 = VECTOR ( 'NONE', #45002, 1000.000000000000114 ) ;
#33692 = EDGE_CURVE ( 'NONE', #12857, #30611, #46574, .T. ) ;
#33693 = CARTESIAN_POINT ( 'NONE',  ( -3.000000000000002665, 2.353404862842836044E-15, 19.21700905503013601 ) ) ;
#33694 = CARTESIAN_POINT ( 'NONE',  ( 4.999999999999999112, -16.65560815589383381, -38.55633173627028754 ) ) ;
#33695 = DIRECTION ( 'NONE',  ( -1.000000000000000000, -0.000000000000000000, -0.000000000000000000 ) ) ;
#33696 = EDGE_CURVE ( 'NONE', #33667, #14588, #38752, .T. ) ;
#33697 = CIRCLE ( 'NONE', #21956, 31.99999999999999289 ) ;
#33698 = DIRECTION ( 'NONE',  ( 1.000000000000000000, 0.000000000000000000, 0.000000000000000000 ) ) ;
#33699 = CYLINDRICAL_SURFACE ( 'NONE', #24752, 37.49900000000000233 ) ;
#33700 = AXIS2_PLACEMENT_3D ( 'NONE', #21711, #44234, #43985 ) ;
#33701 = CARTESIAN_POINT ( 'NONE',  ( 12.00000000000000000, -1.278221433540507546, -26.51162292216071492 ) ) ;
#33702 = ORIENTED_EDGE ( 'NONE', *, *, #37418, .F. ) ;
#33703 = DIRECTION ( 'NONE',  ( 0.000000000000000000, 0.000000000000000000, -1.000000000000000000 ) ) ;
#33704 = CYLINDRICAL_SURFACE ( 'NONE', #19041, 82.00000000000000000 ) ;
#33705 = EDGE_CURVE ( 'NONE', #20259, #24269, #15043, .T. ) ;
#33706 = EDGE_CURVE ( 'NONE', #11474, #35410, #29719, .T. ) ;
#33707 = EDGE_LOOP ( 'NONE', ( #2420, #4886, #13342, #812 ) ) ;
#33708 = VERTEX_POINT ( 'NONE', #3776 ) ;
#33709 = EDGE_LOOP ( 'NONE', ( #15404, #4903, #25292, #46380 ) ) ;
#33710 = FACE_OUTER_BOUND ( 'NONE', #8431, .T. ) ;
#33711 = CARTESIAN_POINT ( 'NONE',  ( 11.99999999999999822, 70.53064760720316428, -26.01480285779861035 ) ) ;
#33712 = ORIENTED_EDGE ( 'NONE', *, *, #17692, .F. ) ;
#33713 = PRODUCT_DEFINITION ( 'UNKNOWN', '', #2198, #33041 ) ;
#33714 = VECTOR ( 'NONE', #26366, 1000.000000000000227 ) ;
#33715 = CIRCLE ( 'NONE', #11819, 77.49899999999999523 ) ;
#33716 = DIRECTION ( 'NONE',  ( 0.000000000000000000, 0.000000000000000000, -1.000000000000000000 ) ) ;
#33717 = AXIS2_PLACEMENT_3D ( 'NONE', #27082, #11437, #38094 ) ;
#33718 = AXIS2_PLACEMENT_3D ( 'NONE', #16578, #1909, #46697 ) ;
#33719 = EDGE_LOOP ( 'NONE', ( #17415, #433, #47975, #43086 ) ) ;
#33720 = ORIENTED_EDGE ( 'NONE', *, *, #39138, .F. ) ;
#33721 = CARTESIAN_POINT ( 'NONE',  ( 0.000000000000000000, 16.65560815589411092, 38.55633173627015253 ) ) ;
#33722 = DIRECTION ( 'NONE',  ( 0.000000000000000000, -0.1564344650402381132, 0.9876883405951365491 ) ) ;
#33723 = CARTESIAN_POINT ( 'NONE',  ( 10.00000000000000000, -59.03342792756231461, -46.54456581323868392 ) ) ;
#33724 = EDGE_LOOP ( 'NONE', ( #30391, #18714, #4608, #14602 ) ) ;
#33725 = CARTESIAN_POINT ( 'NONE',  ( -10.00000000000000000, 0.000000000000000000, 0.000000000000000000 ) ) ;
#33726 = EDGE_LOOP ( 'NONE', ( #48190, #8423, #1477, #28910 ) ) ;
#33727 = CARTESIAN_POINT ( 'NONE',  ( 0.000000000000000000, -120.0000000000000000, 2.500000000000000000 ) ) ;
#33728 = DIRECTION ( 'NONE',  ( 0.000000000000000000, -0.9945218953682740670, -0.1045284632676459352 ) ) ;
#33729 = CARTESIAN_POINT ( 'NONE',  ( 6.000000000000000000, -39.47590169984898267, 71.87247863392400404 ) ) ;
#33730 = ORIENTED_EDGE ( 'NONE', *, *, #23760, .T. ) ;
#33731 = ORIENTED_EDGE ( 'NONE', *, *, #13808, .T. ) ;
#33732 = CARTESIAN_POINT ( 'NONE',  ( 5.000000000000000000, 63.97538442413498672, -51.29473840253155714 ) ) ;
#33733 = CARTESIAN_POINT ( 'NONE',  ( 50.00005079999999680, 12.24744871391588852, 2.500000000000003553 ) ) ;
#33734 = EDGE_CURVE ( 'NONE', #39455, #3739, #37791, .T. ) ;
#33735 = ORIENTED_EDGE ( 'NONE', *, *, #18767, .T. ) ;
#33736 = VERTEX_POINT ( 'NONE', #11384 ) ;
#33737 = DIRECTION ( 'NONE',  ( 0.000000000000000000, -0.9781476007338041345, 0.2079116908177663092 ) ) ;
#33738 = VERTEX_POINT ( 'NONE', #41238 ) ;
#33739 = CARTESIAN_POINT ( 'NONE',  ( 0.000000000000000000, -10.96151621346461447, -35.95386929396268272 ) ) ;
#33740 = ADVANCED_FACE ( 'NONE', ( #22618 ), #22857, .T. ) ;
#33741 = DIRECTION ( 'NONE',  ( 1.000000000000000000, 0.000000000000000000, 0.000000000000000000 ) ) ;
#33742 = FACE_OUTER_BOUND ( 'NONE', #28941, .T. ) ;
#33743 = DIRECTION ( 'NONE',  ( -1.000000000000000000, -0.000000000000000000, 0.000000000000000000 ) ) ;
#33744 = LINE ( 'NONE', #26425, #179 ) ;
#33745 = LINE ( 'NONE', #37671, #9372 ) ;
#33746 = EDGE_CURVE ( 'NONE', #23138, #33708, #43431, .T. ) ;
#33748 = CIRCLE ( 'NONE', #47037, 31.99999999999998934 ) ;
#33747 = LINE ( 'NONE', #41121, #45105 ) ;
#33749 = DIRECTION ( 'NONE',  ( -1.000000000000000000, 0.000000000000000000, 0.000000000000000000 ) ) ;
#33750 = DIRECTION ( 'NONE',  ( 0.000000000000000000, 0.000000000000000000, 1.000000000000000000 ) ) ;
#33751 = VERTEX_POINT ( 'NONE', #40995 ) ;
#33752 = VECTOR ( 'NONE', #25959, 1000.000000000000114 ) ;
#33753 = CARTESIAN_POINT ( 'NONE',  ( 11.99999999999999822, 0.000000000000000000, 0.000000000000000000 ) ) ;
#33754 = DIRECTION ( 'NONE',  ( 0.000000000000000000, 0.000000000000000000, 1.000000000000000000 ) ) ;
#33755 = DIRECTION ( 'NONE',  ( 0.000000000000000000, 0.000000000000000000, 1.000000000000000000 ) ) ;
#33756 = VECTOR ( 'NONE', #13120, 1000.000000000000000 ) ;
#33757 = EDGE_CURVE ( 'NONE', #31567, #32256, #40508, .T. ) ;
#33758 = ADVANCED_FACE ( 'NONE', ( #48086 ), #22389, .T. ) ;
#33759 = ORIENTED_EDGE ( 'NONE', *, *, #9430, .T. ) ;
#33760 = CARTESIAN_POINT ( 'NONE',  ( -21.33958957442910886, -129.9559990355020034, -5.500000000000000000 ) ) ;
#33761 = AXIS2_PLACEMENT_3D ( 'NONE', #34443, #26159, #25901 ) ;
#33762 = CARTESIAN_POINT ( 'NONE',  ( 0.000000000000000000, -41.19522573413689059, -65.64334221924951862 ) ) ;
#33763 = CARTESIAN_POINT ( 'NONE',  ( 0.000000000000000000, 26.79245525562762253, -32.34446384429942611 ) ) ;
#33764 = ORIENTED_EDGE ( 'NONE', *, *, #22706, .F. ) ;
#33765 = EDGE_CURVE ( 'NONE', #19183, #14880, #47338, .T. ) ;
#33766 = VERTEX_POINT ( 'NONE', #46108 ) ;
#33767 = DIRECTION ( 'NONE',  ( -1.000000000000000000, -0.000000000000000000, -0.000000000000000000 ) ) ;
#33768 = AXIS2_PLACEMENT_3D ( 'NONE', #11725, #8292, #30091 ) ;
#33769 = ORIENTED_EDGE ( 'NONE', *, *, #17208, .T. ) ;
#33770 = ORIENTED_EDGE ( 'NONE', *, *, #26562, .F. ) ;
#33771 = EDGE_LOOP ( 'NONE', ( #676, #33268, #46676, #40971 ) ) ;
#33772 = ORIENTED_EDGE ( 'NONE', *, *, #4171, .F. ) ;
#33773 = DIRECTION ( 'NONE',  ( 0.000000000000000000, -0.9723699203976741146, -0.2334453638559160493 ) ) ;
#33774 = DIRECTION ( 'NONE',  ( -1.000000000000000000, 0.000000000000000000, 0.000000000000000000 ) ) ;
#33775 = ORIENTED_EDGE ( 'NONE', *, *, #42232, .T. ) ;
#33776 = ORIENTED_EDGE ( 'NONE', *, *, #35541, .F. ) ;
#33777 = DIRECTION ( 'NONE',  ( -1.000000000000000000, 0.000000000000000000, 0.000000000000000000 ) ) ;
#33778 = AXIS2_PLACEMENT_3D ( 'NONE', #28380, #36911, #7062 ) ;
#33779 = ORIENTED_EDGE ( 'NONE', *, *, #42005, .T. ) ;
#33780 = PLANE ( 'NONE',  #44998 ) ;
#33781 = CARTESIAN_POINT ( 'NONE',  ( 4.999999999999999112, -2.663952781846440576, 41.91543099594817789 ) ) ;
#33782 = ORIENTED_EDGE ( 'NONE', *, *, #26246, .F. ) ;
#33783 = VECTOR ( 'NONE', #44294, 1000.000000000000114 ) ;
#33784 = VERTEX_POINT ( 'NONE', #23343 ) ;
#33785 = CARTESIAN_POINT ( 'NONE',  ( 0.000000000000000000, -74.18225833017913828, 34.94270380257611208 ) ) ;
#33786 = DIRECTION ( 'NONE',  ( -1.000000000000000000, -0.000000000000000000, 0.000000000000000000 ) ) ;
#33787 = ORIENTED_EDGE ( 'NONE', *, *, #35037, .F. ) ;
#33788 = CARTESIAN_POINT ( 'NONE',  ( -12.50000000000000000, -107.5000000000000000, 2.500000000000000000 ) ) ;
#33789 = DIRECTION ( 'NONE',  ( 1.000000000000000000, 0.000000000000000000, 0.000000000000000000 ) ) ;
#33790 = VERTEX_POINT ( 'NONE', #12578 ) ;
#33791 = DIRECTION ( 'NONE',  ( 0.000000000000000000, 0.000000000000000000, 1.000000000000000000 ) ) ;
#33792 = EDGE_LOOP ( 'NONE', ( #10112, #29799 ) ) ;
#33793 = CARTESIAN_POINT ( 'NONE',  ( 11.99999999999999822, 8.966570791700714693, 81.50828551894230145 ) ) ;
#33794 = FACE_OUTER_BOUND ( 'NONE', #48413, .T. ) ;
#33795 = VERTEX_POINT ( 'NONE', #45613 ) ;
#33796 = VECTOR ( 'NONE', #7475, 1000.000000000000000 ) ;
#33797 = EDGE_CURVE ( 'NONE', #28683, #29530, #6703, .T. ) ;
#33798 = CARTESIAN_POINT ( 'NONE',  ( 0.000000000000000000, -80.55351364060599906, 15.33399622253456585 ) ) ;
#33799 = CARTESIAN_POINT ( 'NONE',  ( 11.99999999999999822, 71.27951684758026829, 30.41916302227139113 ) ) ;
#33800 = PLANE ( 'NONE',  #12825 ) ;
#33801 = EDGE_CURVE ( 'NONE', #28193, #13250, #35082, .T. ) ;
#33802 = CARTESIAN_POINT ( 'NONE',  ( 0.000000000000000000, 41.91543099594818500, -2.663952781846294915 ) ) ;
#33803 = EDGE_CURVE ( 'NONE', #34159, #22253, #44994, .T. ) ;
#33804 = DIRECTION ( 'NONE',  ( 0.000000000000000000, 0.000000000000000000, 1.000000000000000000 ) ) ;
#33805 = EDGE_CURVE ( 'NONE', #48194, #23375, #2776, .T. ) ;
#33806 = LINE ( 'NONE', #48019, #1257 ) ;
#33807 = VERTEX_POINT ( 'NONE', #1800 ) ;
#33808 = DIRECTION ( 'NONE',  ( -0.8225049752423776450, -0.5687579148473765889, 0.000000000000000000 ) ) ;
#33810 = EDGE_CURVE ( 'NONE', #27708, #46337, #8894, .T. ) ;
#33809 = DIRECTION ( 'NONE',  ( 0.000000000000000000, 0.8090169943749445647, 0.5877852522924770229 ) ) ;
#33811 = DIRECTION ( 'NONE',  ( -1.000000000000000000, 0.000000000000000000, 0.000000000000000000 ) ) ;
#33812 = DIRECTION ( 'NONE',  ( 1.000000000000000000, 0.000000000000000000, 0.000000000000000000 ) ) ;
#33813 = AXIS2_PLACEMENT_3D ( 'NONE', #22501, #6845, #17847 ) ;
#33814 = DIRECTION ( 'NONE',  ( -1.000000000000000000, 0.000000000000000000, -0.000000000000000000 ) ) ;
#33815 = DIRECTION ( 'NONE',  ( 1.000000000000000000, -0.000000000000000000, -0.000000000000000000 ) ) ;
#33817 = AXIS2_PLACEMENT_3D ( 'NONE', #43423, #6696, #18163 ) ;
#33816 = DIRECTION ( 'NONE',  ( -1.000000000000000000, 0.000000000000000000, -0.000000000000000000 ) ) ;
#33818 = DIRECTION ( 'NONE',  ( -1.000000000000000000, 0.000000000000000000, 0.000000000000000000 ) ) ;
#33819 = EDGE_CURVE ( 'NONE', #11732, #21639, #34855, .T. ) ;
#33820 = AXIS2_PLACEMENT_3D ( 'NONE', #31196, #1328, #23841 ) ;
#33821 = VERTEX_POINT ( 'NONE', #16257 ) ;
#33822 = VECTOR ( 'NONE', #42733, 1000.000000000000000 ) ;
#33823 = LINE ( 'NONE', #37748, #12809 ) ;
#33824 = ORIENTED_EDGE ( 'NONE', *, *, #10774, .T. ) ;
#33825 = EDGE_CURVE ( 'NONE', #45805, #6579, #24734, .T. ) ;
#33826 = LINE ( 'NONE', #12535, #31504 ) ;
#33827 = AXIS2_PLACEMENT_3D ( 'NONE', #35962, #10255, #6119 ) ;
#33828 = DIRECTION ( 'NONE',  ( -1.908195823574487804E-17, -1.387778780781445676E-17, 1.000000000000000000 ) ) ;
#33829 = AXIS2_PLACEMENT_3D ( 'NONE', #28324, #38882, #39611 ) ;
#33830 = DIRECTION ( 'NONE',  ( -1.000000000000000000, -0.000000000000000000, 0.000000000000000000 ) ) ;
#33831 = CIRCLE ( 'NONE', #11164, 16.00000000000000000 ) ;
#33832 = ORIENTED_EDGE ( 'NONE', *, *, #34174, .T. ) ;
#33833 = ADVANCED_FACE ( 'NONE', ( #31191, #23109 ), #38521, .T. ) ;
#33834 = CIRCLE ( 'NONE', #8813, 31.99999999999999645 ) ;
#33835 = AXIS2_PLACEMENT_3D ( 'NONE', #37810, #34358, #15537 ) ;
#33836 = CARTESIAN_POINT ( 'NONE',  ( 11.99999999999999822, -34.44570377933647620, 69.42325613327427902 ) ) ;
#33837 = ORIENTED_EDGE ( 'NONE', *, *, #29501, .F. ) ;
#33838 = EDGE_CURVE ( 'NONE', #29381, #41954, #12236, .T. ) ;
#33839 = DIRECTION ( 'NONE',  ( 0.000000000000000000, 0.000000000000000000, 1.000000000000000000 ) ) ;
#33840 = DIRECTION ( 'NONE',  ( 1.000000000000000000, 0.000000000000000000, -0.000000000000000000 ) ) ;
#33842 = ORIENTED_EDGE ( 'NONE', *, *, #16923, .T. ) ;
#33841 = CARTESIAN_POINT ( 'NONE',  ( 10.00000000000000000, -0.8828120875903202602, 37.48860685352291000 ) ) ;
#33843 = ORIENTED_EDGE ( 'NONE', *, *, #27471, .T. ) ;
#33844 = AXIS2_PLACEMENT_3D ( 'NONE', #32339, #13966, #43363 ) ;
#33845 = DIRECTION ( 'NONE',  ( -1.000000000000000000, -0.000000000000000000, 0.000000000000000000 ) ) ;
#33846 = CARTESIAN_POINT ( 'NONE',  ( -4.250000000000000000, -13.95926121303099343, 0.000000000000000000 ) ) ;
#33847 = PLANE ( 'NONE',  #133 ) ;
#33848 = AXIS2_PLACEMENT_3D ( 'NONE', #24966, #46785, #17860 ) ;
#33849 = DIRECTION ( 'NONE',  ( 0.000000000000000000, 0.9876883405951371042, 0.1564344650402346715 ) ) ;
#33850 = ORIENTED_EDGE ( 'NONE', *, *, #5209, .F. ) ;
#33851 = PLANE ( 'NONE',  #43553 ) ;
#33852 = VERTEX_POINT ( 'NONE', #30952 ) ;
#33853 = EDGE_LOOP ( 'NONE', ( #673, #7827, #33494, #30263 ) ) ;
#33854 = ADVANCED_FACE ( 'NONE', ( #5241 ), #4511, .F. ) ;
#33855 = AXIS2_PLACEMENT_3D ( 'NONE', #36400, #40333, #39840 ) ;
#33856 = CARTESIAN_POINT ( 'NONE',  ( 11.99999999999999822, -68.67312586194971402, -35.91791733033549860 ) ) ;
#33857 = AXIS2_PLACEMENT_3D ( 'NONE', #32252, #28095, #20257 ) ;
#33858 = ADVANCED_FACE ( 'NONE', ( #15763 ), #20154, .T. ) ;
#33859 = DIRECTION ( 'NONE',  ( -1.000000000000000000, -0.000000000000000000, 0.000000000000000000 ) ) ;
#33860 = CARTESIAN_POINT ( 'NONE',  ( 11.99999999999999822, -51.02545421589285723, -55.20638768913812555 ) ) ;
#33861 = DIRECTION ( 'NONE',  ( 0.000000000000000000, 0.9876883405951381034, -0.1564344650402276216 ) ) ;
#33862 = ORIENTED_EDGE ( 'NONE', *, *, #22597, .F. ) ;
#33863 = DIRECTION ( 'NONE',  ( -1.000000000000000000, 0.000000000000000000, 0.000000000000000000 ) ) ;
#33864 = AXIS2_PLACEMENT_3D ( 'NONE', #48150, #40806, #47894 ) ;
#33865 = CARTESIAN_POINT ( 'NONE',  ( 10.00000000000000000, 37.58145647212453611, 0.6853352020791767529 ) ) ;
#33866 = EDGE_CURVE ( 'NONE', #17937, #22938, #13762, .T. ) ;
#33867 = LINE ( 'NONE', #36814, #2403 ) ;
#33868 = CARTESIAN_POINT ( 'NONE',  ( 0.000000000000000000, 0.000000000000000000, 0.000000000000000000 ) ) ;
#33869 = DIRECTION ( 'NONE',  ( -0.000000000000000000, -0.000000000000000000, -1.000000000000000000 ) ) ;
#33870 = AXIS2_PLACEMENT_3D ( 'NONE', #14885, #28493, #16985 ) ;
#33871 = DIRECTION ( 'NONE',  ( -0.4796670183876317051, 0.8774505977381972244, 0.000000000000000000 ) ) ;
#33873 = EDGE_CURVE ( 'NONE', #6771, #33652, #5986, .T. ) ;
#33872 = DIRECTION ( 'NONE',  ( -1.000000000000000000, 0.000000000000000000, 0.000000000000000000 ) ) ;
#33874 = DIRECTION ( 'NONE',  ( -1.000000000000000000, -0.000000000000000000, 0.000000000000000000 ) ) ;
#33875 = AXIS2_PLACEMENT_3D ( 'NONE', #45839, #33830, #23539 ) ;
#33876 = DIRECTION ( 'NONE',  ( 0.000000000000000000, 0.8660254037844359321, 0.5000000000000046629 ) ) ;
#33877 = FACE_OUTER_BOUND ( 'NONE', #20007, .T. ) ;
#33878 = AXIS2_PLACEMENT_3D ( 'NONE', #3506, #14537, #32418 ) ;
#33879 = PLANE ( 'NONE',  #10632 ) ;
#33880 = DIRECTION ( 'NONE',  ( -1.000000000000000000, 0.000000000000000000, -0.000000000000000000 ) ) ;
#33881 = CARTESIAN_POINT ( 'NONE',  ( 11.99999999999999822, 0.000000000000000000, 0.000000000000000000 ) ) ;
#33882 = DIRECTION ( 'NONE',  ( -1.000000000000000000, 0.000000000000000000, 0.000000000000000000 ) ) ;
#33883 = DIRECTION ( 'NONE',  ( 0.000000000000000000, 0.8526401643540935105, -0.5224985647159466895 ) ) ;
#33884 = CYLINDRICAL_SURFACE ( 'NONE', #26008, 15.99999999999999645 ) ;
#33885 = ORIENTED_EDGE ( 'NONE', *, *, #26536, .F. ) ;
#33886 = EDGE_LOOP ( 'NONE', ( #2983, #33433, #44980, #4950 ) ) ;
#33887 = AXIS2_PLACEMENT_3D ( 'NONE', #41128, #26433, #19071 ) ;
#33888 = ORIENTED_EDGE ( 'NONE', *, *, #35651, .F. ) ;
#33889 = VECTOR ( 'NONE', #3530, 1000.000000000000000 ) ;
#33890 = AXIS2_PLACEMENT_3D ( 'NONE', #26350, #30273, #13348 ) ;
#33891 = AXIS2_PLACEMENT_3D ( 'NONE', #27709, #42642, #9101 ) ;
#33892 = DIRECTION ( 'NONE',  ( 0.000000000000000000, 0.000000000000000000, 1.000000000000000000 ) ) ;
#33893 = ORIENTED_EDGE ( 'NONE', *, *, #39198, .F. ) ;
#33894 = AXIS2_PLACEMENT_3D ( 'NONE', #44323, #29396, #28897 ) ;
#33895 = AXIS2_PLACEMENT_3D ( 'NONE', #39012, #21116, #5476 ) ;
#33896 = CARTESIAN_POINT ( 'NONE',  ( -3.000000000000000000, 22.07842321921481243, 8.187992925817422218 ) ) ;
#33897 = LINE ( 'NONE', #34610, #13301 ) ;
#33898 = FACE_OUTER_BOUND ( 'NONE', #13802, .T. ) ;
#33899 = ORIENTED_EDGE ( 'NONE', *, *, #32603, .F. ) ;
#33900 = CARTESIAN_POINT ( 'NONE',  ( 8.452893869119503023, -12.51233732111638375, -1.199999999999999956 ) ) ;
#33901 = ORIENTED_EDGE ( 'NONE', *, *, #1025, .F. ) ;
#33902 = ORIENTED_EDGE ( 'NONE', *, *, #32561, .F. ) ;
#33903 = VERTEX_POINT ( 'NONE', #42687 ) ;
#33904 = AXIS2_PLACEMENT_3D ( 'NONE', #63, #22590, #15265 ) ;
#33905 = CARTESIAN_POINT ( 'NONE',  ( 10.00000000000000000, 30.80686688397041451, -21.53537804866048688 ) ) ;
#33906 = DIRECTION ( 'NONE',  ( -1.000000000000000000, 0.000000000000000000, -0.000000000000000000 ) ) ;
#33907 = CARTESIAN_POINT ( 'NONE',  ( 22.63442173698368620, -133.7816164738524378, 2.500000000000000000 ) ) ;
#33908 = ORIENTED_EDGE ( 'NONE', *, *, #15973, .F. ) ;
#33909 = ORIENTED_EDGE ( 'NONE', *, *, #32715, .T. ) ;
#33910 = LINE ( 'NONE', #31230, #16170 ) ;
#33911 = VERTEX_POINT ( 'NONE', #24079 ) ;
#33912 = EDGE_CURVE ( 'NONE', #28886, #13717, #39594, .T. ) ;
#33913 = CYLINDRICAL_SURFACE ( 'NONE', #11335, 31.99999999999998579 ) ;
#33914 = CARTESIAN_POINT ( 'NONE',  ( 11.99999999999999822, 62.50329211542494789, -41.76937507738723099 ) ) ;
#33915 = LINE ( 'NONE', #398, #8074 ) ;
#33916 = CARTESIAN_POINT ( 'NONE',  ( -10.90076147243505211, 1.679431090506078290E-15, -13.71319123027096865 ) ) ;
#33917 = DIRECTION ( 'NONE',  ( 0.000000000000000000, 0.000000000000000000, 1.000000000000000000 ) ) ;
#33918 = EDGE_CURVE ( 'NONE', #20499, #24200, #18473, .T. ) ;
#33919 = CARTESIAN_POINT ( 'NONE',  ( 10.00000000000000000, 0.000000000000000000, 0.000000000000000000 ) ) ;
#33920 = LINE ( 'NONE', #36633, #8433 ) ;
#33921 = PRESENTATION_STYLE_ASSIGNMENT (( #18988 ) ) ;
#33922 = DIRECTION ( 'NONE',  ( -1.000000000000000000, 0.000000000000000000, -0.000000000000000000 ) ) ;
#33923 = ORIENTED_EDGE ( 'NONE', *, *, #10526, .F. ) ;
#33924 = DIRECTION ( 'NONE',  ( 1.000000000000000000, 0.000000000000000000, -0.000000000000000000 ) ) ;
#33925 = AXIS2_PLACEMENT_3D ( 'NONE', #20878, #31913, #16478 ) ;
#33926 = ORIENTED_EDGE ( 'NONE', *, *, #31512, .F. ) ;
#33927 = ORIENTED_EDGE ( 'NONE', *, *, #40181, .F. ) ;
#33929 = EDGE_CURVE ( 'NONE', #3743, #17460, #8176, .T. ) ;
#33928 = CARTESIAN_POINT ( 'NONE',  ( 10.00000000000000000, 0.000000000000000000, 0.000000000000000000 ) ) ;
#33930 = VECTOR ( 'NONE', #26174, 1000.000000000000000 ) ;
#33931 = CIRCLE ( 'NONE', #4250, 16.00000000000000000 ) ;
#33932 = DIRECTION ( 'NONE',  ( -1.000000000000000000, -0.000000000000000000, 0.000000000000000000 ) ) ;
#33933 = ADVANCED_FACE ( 'NONE', ( #35810, #35575 ), #27999, .F. ) ;
#33934 = DIRECTION ( 'NONE',  ( -1.000000000000000000, 0.000000000000000000, 0.000000000000000000 ) ) ;
#33935 = CARTESIAN_POINT ( 'NONE',  ( 15.00000000000000000, -19.89357724624986545, 12.59942793731086219 ) ) ;
#33936 = LINE ( 'NONE', #11920, #8406 ) ;
#33937 = ORIENTED_EDGE ( 'NONE', *, *, #25873, .T. ) ;
#33938 = VECTOR ( 'NONE', #9985, 1000.000000000000000 ) ;
#33939 = AXIS2_PLACEMENT_3D ( 'NONE', #2003, #12763, #27700 ) ;
#33940 = DIRECTION ( 'NONE',  ( 0.000000000000000000, -0.3090169943749548342, 0.9510565162951511997 ) ) ;
#33941 = CARTESIAN_POINT ( 'NONE',  ( 10.00000000000000000, -35.38097989696503021, -12.42422080174676147 ) ) ;
#33942 = AXIS2_PLACEMENT_3D ( 'NONE', #30056, #22229, #37154 ) ;
#33943 = DIRECTION ( 'NONE',  ( 0.000000000000000000, 0.000000000000000000, 1.000000000000000000 ) ) ;
#33944 =( NAMED_UNIT ( * ) PLANE_ANGLE_UNIT ( ) SI_UNIT ( $, .RADIAN. ) );
#33945 = CARTESIAN_POINT ( 'NONE',  ( -10.00000000000000000, 0.000000000000000000, 0.000000000000000000 ) ) ;
#33946 = AXIS2_PLACEMENT_3D ( 'NONE', #5368, #37937, #719 ) ;
#33947 = ORIENTED_EDGE ( 'NONE', *, *, #28618, .F. ) ;
#33948 = ORIENTED_EDGE ( 'NONE', *, *, #37455, .T. ) ;
#33949 = ORIENTED_EDGE ( 'NONE', *, *, #45210, .F. ) ;
#33950 = CARTESIAN_POINT ( 'NONE',  ( 0.000000000000000000, 33.79645857604513992, -16.45098606841138178 ) ) ;
#33951 = CARTESIAN_POINT ( 'NONE',  ( 5.000000000000002665, 3.894527615419058009, -81.90746397400384637 ) ) ;
#33952 = VERTEX_POINT ( 'NONE', #2505 ) ;
#33953 = VECTOR ( 'NONE', #44048, 1000.000000000000114 ) ;
#33954 = ADVANCED_FACE ( 'NONE', ( #24797 ), #10333, .F. ) ;
#33955 = CYLINDRICAL_SURFACE ( 'NONE', #30420, 77.49899999999999523 ) ;
#33956 = CIRCLE ( 'NONE', #1950, 16.00000000000000000 ) ;
#33957 = VECTOR ( 'NONE', #41977, 1000.000000000000000 ) ;
#33958 = EDGE_CURVE ( 'NONE', #41511, #20399, #39739, .T. ) ;
#33959 = EDGE_LOOP ( 'NONE', ( #42800, #13340, #13705, #5837 ) ) ;
#33960 = ORIENTED_EDGE ( 'NONE', *, *, #25291, .T. ) ;
#33961 = PRODUCT_DEFINITION_SHAPE ( 'NONE', 'NONE',  #48457 ) ;
#33962 = EDGE_CURVE ( 'NONE', #10970, #21061, #16906, .T. ) ;
#33963 = DIRECTION ( 'NONE',  ( 0.000000000000000000, 0.3826834323650907810, -0.9238795325112864054 ) ) ;
#33965 = ORIENTED_EDGE ( 'NONE', *, *, #47712, .T. ) ;
#33964 = CARTESIAN_POINT ( 'NONE',  ( 12.50000000000000000, -132.5000000000000000, -40.00000000000000000 ) ) ;
#33966 = CARTESIAN_POINT ( 'NONE',  ( 11.99999999999999822, 0.8261519478431255115, 77.49459641780886443 ) ) ;
#33967 = AXIS2_PLACEMENT_3D ( 'NONE', #48115, #14601, #18961 ) ;
#33968 = VERTEX_POINT ( 'NONE', #36287 ) ;
#33969 = CARTESIAN_POINT ( 'NONE',  ( 10.00000000000000000, -12.93880638057259169, -76.41127070299286572 ) ) ;
#33970 = EDGE_LOOP ( 'NONE', ( #47131, #20603, #25929, #18564 ) ) ;
#33971 = ORIENTED_EDGE ( 'NONE', *, *, #18095, .T. ) ;
#33972 = VECTOR ( 'NONE', #21228, 1000.000000000000000 ) ;
#33973 = CARTESIAN_POINT ( 'NONE',  ( 1.499592026101426168, -120.0349822133818094, 2.500000000000000000 ) ) ;
#33974 = CIRCLE ( 'NONE', #1142, 31.99999999999998579 ) ;
#33975 = AXIS2_PLACEMENT_3D ( 'NONE', #25495, #22058, #3211 ) ;
#33976 = DIRECTION ( 'NONE',  ( 0.000000000000000000, -0.8910065241883626808, -0.4539904997395568520 ) ) ;
#33977 = EDGE_CURVE ( 'NONE', #11749, #4261, #5712, .T. ) ;
#33978 = CARTESIAN_POINT ( 'NONE',  ( 0.000000000000000000, 0.000000000000000000, 42.00000000000001421 ) ) ;
#33980 = ORIENTED_EDGE ( 'NONE', *, *, #17112, .F. ) ;
#33979 = VECTOR ( 'NONE', #18740, 1000.000000000000000 ) ;
#33981 = EDGE_CURVE ( 'NONE', #47549, #8466, #33315, .T. ) ;
#33982 = EDGE_CURVE ( 'NONE', #16811, #37458, #3619, .T. ) ;
#33983 = ORIENTED_EDGE ( 'NONE', *, *, #42033, .T. ) ;
#33984 = CARTESIAN_POINT ( 'NONE',  ( -7.670864526094549163, -97.73662565058241114, 5.500000000000000000 ) ) ;
#33985 = CARTESIAN_POINT ( 'NONE',  ( 10.00000000000000000, 0.000000000000000000, 0.000000000000000000 ) ) ;
#33986 = ORIENTED_EDGE ( 'NONE', *, *, #48049, .F. ) ;
#33987 = VERTEX_POINT ( 'NONE', #14014 ) ;
#33988 = DIRECTION ( 'NONE',  ( -1.000000000000000000, 0.000000000000000000, 0.000000000000000000 ) ) ;
#33989 = ORIENTED_EDGE ( 'NONE', *, *, #12601, .T. ) ;
#33990 = CARTESIAN_POINT ( 'NONE',  ( 11.99999999999999822, 66.50666863322055633, -39.78640506895536078 ) ) ;
#33991 = LINE ( 'NONE', #22504, #1948 ) ;
#33992 = DIRECTION ( 'NONE',  ( 0.000000000000000000, 0.000000000000000000, 1.000000000000000000 ) ) ;
#33993 = DIRECTION ( 'NONE',  ( 1.000000000000000000, 0.000000000000000000, 0.000000000000000000 ) ) ;
#33994 = DIRECTION ( 'NONE',  ( 0.000000000000000000, 0.3090169943749580539, -0.9510565162951500895 ) ) ;
#33995 = DIRECTION ( 'NONE',  ( -1.000000000000000000, 0.000000000000000000, 0.000000000000000000 ) ) ;
#33996 = DIRECTION ( 'NONE',  ( 0.000000000000000000, 0.000000000000000000, -1.000000000000000000 ) ) ;
#33997 = AXIS2_PLACEMENT_3D ( 'NONE', #22980, #33741, #19059 ) ;
#33998 = DIRECTION ( 'NONE',  ( -1.000000000000000000, -0.000000000000000000, 0.000000000000000000 ) ) ;
#33999 = CARTESIAN_POINT ( 'NONE',  ( -3.000000000000000000, -19.89357724624987256, -12.59942793731086041 ) ) ;
#34000 = VECTOR ( 'NONE', #23333, 1000.000000000000000 ) ;
#34001 = DIRECTION ( 'NONE',  ( -1.000000000000000000, 0.000000000000000000, -0.000000000000000000 ) ) ;
#34002 = CARTESIAN_POINT ( 'NONE',  ( 22.08297821871651934, -111.8242998470044540, -5.500000000000000000 ) ) ;
#34003 = CARTESIAN_POINT ( 'NONE',  ( 0.000000000000000000, -77.49459641780886443, -0.8261519478439277586 ) ) ;
#34004 = ORIENTED_EDGE ( 'NONE', *, *, #37260, .F. ) ;
#34005 = CIRCLE ( 'NONE', #2734, 77.49900000000000944 ) ;
#34006 = CIRCLE ( 'NONE', #9801, 15.99999999999999822 ) ;
#34007 = UNCERTAINTY_MEASURE_WITH_UNIT (LENGTH_MEASURE( 1.000000000000000082E-05 ), #21796, 'distance_accuracy_value', 'NONE');
#34008 = CARTESIAN_POINT ( 'NONE',  ( -10.00000000000000000, 0.000000000000000000, 0.000000000000000000 ) ) ;
#34009 = AXIS2_PLACEMENT_3D ( 'NONE', #11911, #25185, #47945 ) ;
#34010 = CARTESIAN_POINT ( 'NONE',  ( 0.000000000000000000, -34.44570377933647620, 69.42325613327427902 ) ) ;
#34011 = CARTESIAN_POINT ( 'NONE',  ( 10.00000000000000000, 22.64427369931212297, -30.00120703465181293 ) ) ;
#34012 = CIRCLE ( 'NONE', #12937, 31.99999999999998224 ) ;
#34013 = ORIENTED_EDGE ( 'NONE', *, *, #27115, .F. ) ;
#34014 = ADVANCED_FACE ( 'NONE', ( #31925 ), #13298, .T. ) ;
#34015 = ORIENTED_EDGE ( 'NONE', *, *, #39897, .T. ) ;
#34016 = ADVANCED_FACE ( 'NONE', ( #32615 ), #28222, .T. ) ;
#34017 = DIRECTION ( 'NONE',  ( 0.000000000000000000, -0.9969173337331287410, 0.07845909572783495156 ) ) ;
#34018 = ORIENTED_EDGE ( 'NONE', *, *, #7174, .T. ) ;
#34019 = EDGE_CURVE ( 'NONE', #1962, #33236, #35665, .T. ) ;
#34020 = EDGE_LOOP ( 'NONE', ( #12059, #45662, #47887, #40847 ) ) ;
#34021 = VERTEX_POINT ( 'NONE', #9607 ) ;
#34022 = AXIS2_PLACEMENT_3D ( 'NONE', #1691, #20039, #31320 ) ;
#34023 = VERTEX_POINT ( 'NONE', #10101 ) ;
#34024 = ADVANCED_FACE ( 'NONE', ( #6679 ), #24555, .F. ) ;
#34025 = VECTOR ( 'NONE', #33871, 999.9999999999998863 ) ;
#34026 = DIRECTION ( 'NONE',  ( -1.000000000000000000, 0.000000000000000000, 0.000000000000000000 ) ) ;
#34027 = VERTEX_POINT ( 'NONE', #36524 ) ;
#34028 = ORIENTED_EDGE ( 'NONE', *, *, #949, .T. ) ;
#34029 = FACE_OUTER_BOUND ( 'NONE', #23200, .T. ) ;
#34030 = ORIENTED_EDGE ( 'NONE', *, *, #549, .F. ) ;
#34031 = DIRECTION ( 'NONE',  ( 0.000000000000000000, 0.3826834323650841752, 0.9238795325112891810 ) ) ;
#34032 = FACE_OUTER_BOUND ( 'NONE', #31062, .T. ) ;
#34033 = ORIENTED_EDGE ( 'NONE', *, *, #7782, .F. ) ;
#34034 = EDGE_CURVE ( 'NONE', #2290, #20052, #9835, .T. ) ;
#34035 = CARTESIAN_POINT ( 'NONE',  ( 15.00000000000000000, -19.89357724624986545, 12.59942793731086219 ) ) ;
#34036 = EDGE_CURVE ( 'NONE', #25837, #10624, #3583, .T. ) ;
#34037 = ORIENTED_EDGE ( 'NONE', *, *, #44437, .T. ) ;
#34038 = CYLINDRICAL_SURFACE ( 'NONE', #36727, 77.49899999999999523 ) ;
#34039 = FACE_OUTER_BOUND ( 'NONE', #37947, .T. ) ;
#34040 = AXIS2_PLACEMENT_3D ( 'NONE', #1535, #13509, #5217 ) ;
#34041 = AXIS2_PLACEMENT_3D ( 'NONE', #6894, #25488, #47748 ) ;
#34042 = VERTEX_POINT ( 'NONE', #5970 ) ;
#34043 = DIRECTION ( 'NONE',  ( -1.000000000000000000, 0.000000000000000000, 0.000000000000000000 ) ) ;
#34044 = ORIENTED_EDGE ( 'NONE', *, *, #21054, .F. ) ;
#34045 = EDGE_LOOP ( 'NONE', ( #39013, #41270, #47820, #1300 ) ) ;
#34046 = DIRECTION ( 'NONE',  ( 0.000000000000000000, 0.3090169943749410120, 0.9510565162951557516 ) ) ;
#34047 = CARTESIAN_POINT ( 'NONE',  ( 10.00000000000000000, 55.16347631943129670, -60.67117009219074220 ) ) ;
#34048 = ORIENTED_EDGE ( 'NONE', *, *, #31312, .F. ) ;
#34049 = DIRECTION ( 'NONE',  ( 0.000000000000000000, 0.3090169943749410120, 0.9510565162951556406 ) ) ;
#34050 = VECTOR ( 'NONE', #35322, 1000.000000000000000 ) ;
#34051 = DIRECTION ( 'NONE',  ( -1.000000000000000000, -0.000000000000000000, 0.000000000000000000 ) ) ;
#34052 = DIRECTION ( 'NONE',  ( 0.000000000000000000, -0.6494480483301739993, -0.7604059656000391465 ) ) ;
#34053 = AXIS2_PLACEMENT_3D ( 'NONE', #26764, #34569, #27747 ) ;
#34054 = FACE_OUTER_BOUND ( 'NONE', #9488, .T. ) ;
#34055 = CARTESIAN_POINT ( 'NONE',  ( 11.99999999999999822, -35.91791733033525702, 68.67312586194982771 ) ) ;
#34056 = EDGE_CURVE ( 'NONE', #18005, #35465, #29409, .T. ) ;
#34057 = DIRECTION ( 'NONE',  ( -1.000000000000000000, 0.000000000000000000, 0.000000000000000000 ) ) ;
#34058 = DIRECTION ( 'NONE',  ( 0.000000000000000000, -0.9510565162951565288, 0.3090169943749383474 ) ) ;
#34059 = CARTESIAN_POINT ( 'NONE',  ( 10.00000000000000000, -6.903761155837252694, -77.19088730480530103 ) ) ;
#34060 = CARTESIAN_POINT ( 'NONE',  ( 10.00000000000000000, 21.32104025579158701, -30.84782396557194772 ) ) ;
#34061 = AXIS2_PLACEMENT_3D ( 'NONE', #9409, #16288, #4785 ) ;
#34062 = LINE ( 'NONE', #25746, #45518 ) ;
#34063 = DIRECTION ( 'NONE',  ( 0.000000000000000000, -0.7071067811865389130, -0.7071067811865561215 ) ) ;
#34064 = LINE ( 'NONE', #45096, #2187 ) ;
#34065 = VECTOR ( 'NONE', #15740, 1000.000000000000000 ) ;
#34066 = DIRECTION ( 'NONE',  ( 0.000000000000000000, 0.7071067811865439090, 0.7071067811865512365 ) ) ;
#34067 = ORIENTED_EDGE ( 'NONE', *, *, #30109, .T. ) ;
#34068 = EDGE_LOOP ( 'NONE', ( #35880, #16539, #9171, #39515 ) ) ;
#34069 = CIRCLE ( 'NONE', #17643, 31.99999999999998934 ) ;
#34070 = DIRECTION ( 'NONE',  ( -1.000000000000000000, 0.000000000000000000, -0.000000000000000000 ) ) ;
#34071 = ORIENTED_EDGE ( 'NONE', *, *, #45829, .F. ) ;
#34072 = DIRECTION ( 'NONE',  ( -1.000000000000000000, 0.000000000000000000, -0.000000000000000000 ) ) ;
#34073 = APPLICATION_PROTOCOL_DEFINITION ( 'draft international standard', 'automotive_design', 1998, #3183 ) ;
#34074 = PLANE ( 'NONE',  #2590 ) ;
#34075 = MECHANICAL_DESIGN_GEOMETRIC_PRESENTATION_REPRESENTATION (  '', ( #9872 ), #27849 ) ;
#34076 = ORIENTED_EDGE ( 'NONE', *, *, #25636, .T. ) ;
#34077 = AXIS2_PLACEMENT_3D ( 'NONE', #35483, #47680, #14171 ) ;
#34078 = ORIENTED_EDGE ( 'NONE', *, *, #5885, .T. ) ;
#34079 = CARTESIAN_POINT ( 'NONE',  ( -3.000000000000000000, -13.04903810567647682, -19.60159698893442481 ) ) ;
#34080 = EDGE_CURVE ( 'NONE', #45900, #24990, #17190, .T. ) ;
#34081 = VECTOR ( 'NONE', #40678, 1000.000000000000000 ) ;
#34082 = ORIENTED_EDGE ( 'NONE', *, *, #18561, .F. ) ;
#34083 = CIRCLE ( 'NONE', #13660, 77.49899999999998101 ) ;
#34084 = EDGE_CURVE ( 'NONE', #3949, #33371, #28612, .T. ) ;
#34085 = DIRECTION ( 'NONE',  ( 0.000000000000000000, 0.000000000000000000, 1.000000000000000000 ) ) ;
#34086 = CIRCLE ( 'NONE', #30902, 12.49999999999999645 ) ;
#34087 = EDGE_CURVE ( 'NONE', #21133, #36907, #2814, .T. ) ;
#34088 = CARTESIAN_POINT ( 'NONE',  ( 10.00000000000000000, 0.000000000000000000, 0.000000000000000000 ) ) ;
#34090 = ORIENTED_EDGE ( 'NONE', *, *, #34087, .F. ) ;
#34089 = DIRECTION ( 'NONE',  ( -1.000000000000000000, 0.000000000000000000, 0.000000000000000000 ) ) ;
#34091 = ORIENTED_EDGE ( 'NONE', *, *, #7698, .T. ) ;
#34092 = AXIS2_PLACEMENT_3D ( 'NONE', #23522, #24249, #1745 ) ;
#34093 = AXIS2_PLACEMENT_3D ( 'NONE', #13994, #28913, #43847 ) ;
#34094 = DIRECTION ( 'NONE',  ( 0.1736481776669309418, -0.9848077530122080203, 0.000000000000000000 ) ) ;
#34095 = DIRECTION ( 'NONE',  ( 0.000000000000000000, 0.000000000000000000, 1.000000000000000000 ) ) ;
#34096 = ADVANCED_FACE ( 'NONE', ( #36998 ), #44835, .T. ) ;
#34097 = CARTESIAN_POINT ( 'NONE',  ( 15.00000000000000000, 0.000000000000000000, 0.000000000000000000 ) ) ;
#34098 = CIRCLE ( 'NONE', #48155, 31.99999999999999289 ) ;
#34099 = CARTESIAN_POINT ( 'NONE',  ( 15.00000000000000000, 16.83928648764945635, 16.46020748918027010 ) ) ;
#34100 = VERTEX_POINT ( 'NONE', #25985 ) ;
#34101 = DIRECTION ( 'NONE',  ( -1.000000000000000000, -0.000000000000000000, 0.000000000000000000 ) ) ;
#34102 = VERTEX_POINT ( 'NONE', #40930 ) ;
#34103 = ORIENTED_EDGE ( 'NONE', *, *, #6752, .T. ) ;
#34104 = EDGE_CURVE ( 'NONE', #47105, #24099, #37731, .T. ) ;
#34105 = CARTESIAN_POINT ( 'NONE',  ( 0.000000000000000000, 14.67089635893713684, 73.72996012237443608 ) ) ;
#34106 = CARTESIAN_POINT ( 'NONE',  ( 10.00000000000000000, -71.21200624218766961, -40.65526001592689909 ) ) ;
#34107 = DIRECTION ( 'NONE',  ( 0.9827303690289279636, 0.1850432970638681840, 0.000000000000000000 ) ) ;
#34108 = LINE ( 'NONE', #30683, #18794 ) ;
#34109 = VERTEX_POINT ( 'NONE', #26245 ) ;
#34110 = DIRECTION ( 'NONE',  ( 0.000000000000000000, 0.000000000000000000, 1.000000000000000000 ) ) ;
#34111 = DIRECTION ( 'NONE',  ( 0.000000000000000000, 0.000000000000000000, 1.000000000000000000 ) ) ;
#34112 = DIRECTION ( 'NONE',  ( -1.000000000000000000, 0.000000000000000000, 0.000000000000000000 ) ) ;
#34113 = CYLINDRICAL_SURFACE ( 'NONE', #8006, 31.99999999999998579 ) ;
#34114 = EDGE_CURVE ( 'NONE', #5335, #29594, #47767, .T. ) ;
#34115 = DIRECTION ( 'NONE',  ( -1.000000000000000000, -0.000000000000000000, 0.000000000000000000 ) ) ;
#34116 = AXIS2_PLACEMENT_3D ( 'NONE', #36906, #3375, #44506 ) ;
#34117 = CARTESIAN_POINT ( 'NONE',  ( 5.000000000000002665, -81.90746397400386059, -3.894527615418773347 ) ) ;
#34118 = DIRECTION ( 'NONE',  ( 0.000000000000000000, 0.07845909572784512398, -0.9969173337331279638 ) ) ;
#34119 = CARTESIAN_POINT ( 'NONE',  ( 10.00000000000000178, 0.000000000000000000, 21.00000000000000000 ) ) ;
#34120 = CIRCLE ( 'NONE', #35705, 42.00000000000000000 ) ;
#34121 = CARTESIAN_POINT ( 'NONE',  ( -10.00000000000000000, 0.000000000000000000, 0.000000000000000000 ) ) ;
#34122 = DIRECTION ( 'NONE',  ( 0.000000000000000000, 0.000000000000000000, 1.000000000000000000 ) ) ;
#34123 = DIRECTION ( 'NONE',  ( -1.000000000000000000, 0.000000000000000000, 0.000000000000000000 ) ) ;
#34124 = EDGE_CURVE ( 'NONE', #30814, #39658, #23926, .T. ) ;
#34125 = ORIENTED_EDGE ( 'NONE', *, *, #48451, .F. ) ;
#34126 = DIRECTION ( 'NONE',  ( -1.000000000000000000, 0.000000000000000000, 0.000000000000000000 ) ) ;
#34127 = DIRECTION ( 'NONE',  ( -1.000000000000000000, 0.000000000000000000, 0.000000000000000000 ) ) ;
#34128 = CARTESIAN_POINT ( 'NONE',  ( 5.000000000000000000, 32.34446384429971744, 26.79245525562726016 ) ) ;
#34129 = VERTEX_POINT ( 'NONE', #41186 ) ;
#34130 = CIRCLE ( 'NONE', #2110, 31.99999999999998224 ) ;
#34131 = DIRECTION ( 'NONE',  ( 0.000000000000000000, 0.000000000000000000, -1.000000000000000000 ) ) ;
#34132 = ORIENTED_EDGE ( 'NONE', *, *, #35711, .T. ) ;
#34133 = AXIS2_PLACEMENT_3D ( 'NONE', #38664, #20277, #35209 ) ;
#34134 = EDGE_CURVE ( 'NONE', #32362, #33911, #41413, .T. ) ;
#34135 = ORIENTED_EDGE ( 'NONE', *, *, #20530, .T. ) ;
#34136 = ORIENTED_EDGE ( 'NONE', *, *, #18721, .F. ) ;
#34137 = EDGE_CURVE ( 'NONE', #27337, #26404, #33806, .T. ) ;
#34138 = ORIENTED_EDGE ( 'NONE', *, *, #2813, .T. ) ;
#34139 = FACE_OUTER_BOUND ( 'NONE', #10083, .T. ) ;
#34140 = ORIENTED_EDGE ( 'NONE', *, *, #39876, .F. ) ;
#34141 = ORIENTED_EDGE ( 'NONE', *, *, #15315, .F. ) ;
#34142 = EDGE_CURVE ( 'NONE', #22817, #48195, #17656, .T. ) ;
#34143 = AXIS2_PLACEMENT_3D ( 'NONE', #27312, #38321, #37837 ) ;
#34144 = CARTESIAN_POINT ( 'NONE',  ( 2.047646702416564768, -96.54137380445985173, -5.500000000000000000 ) ) ;
#34145 = EDGE_CURVE ( 'NONE', #30146, #28808, #11322, .T. ) ;
#34146 = EDGE_CURVE ( 'NONE', #6148, #19113, #7637, .T. ) ;
#34147 =( REPRESENTATION_RELATIONSHIP ('NONE','NONE', #5957, #22809 ) REPRESENTATION_RELATIONSHIP_WITH_TRANSFORMATION ( #4703 )SHAPE_REPRESENTATION_RELATIONSHIP( ) );
#34148 = DIRECTION ( 'NONE',  ( -1.000000000000000000, -0.000000000000000000, 0.000000000000000000 ) ) ;
#34149 = DIRECTION ( 'NONE',  ( -1.000000000000000000, 0.000000000000000000, 0.000000000000000000 ) ) ;
#34150 = EDGE_LOOP ( 'NONE', ( #2674, #185, #14772, #24006 ) ) ;
#34151 = CIRCLE ( 'NONE', #20895, 31.99999999999999645 ) ;
#34152 = DIRECTION ( 'NONE',  ( -1.000000000000000000, 0.000000000000000000, 0.000000000000000000 ) ) ;
#34153 = ORIENTED_EDGE ( 'NONE', *, *, #34614, .T. ) ;
#34154 = CARTESIAN_POINT ( 'NONE',  ( -10.00000000000000000, 0.000000000000000000, 0.000000000000000000 ) ) ;
#34155 = CARTESIAN_POINT ( 'NONE',  ( 0.000000000000000000, -33.00180498840060039, 17.80606268964528027 ) ) ;
#34156 = ORIENTED_EDGE ( 'NONE', *, *, #30239, .F. ) ;
#34157 = ORIENTED_EDGE ( 'NONE', *, *, #9449, .T. ) ;
#34158 = CIRCLE ( 'NONE', #45890, 16.00000000000000000 ) ;
#34159 = VERTEX_POINT ( 'NONE', #279 ) ;
#34160 = DIRECTION ( 'NONE',  ( -1.000000000000000000, -0.000000000000000000, -0.000000000000000000 ) ) ;
#34161 = ORIENTED_EDGE ( 'NONE', *, *, #11341, .T. ) ;
#34162 = DIRECTION ( 'NONE',  ( 0.000000000000000000, 1.000000000000000000, -1.224646799147353207E-16 ) ) ;
#34163 = DIRECTION ( 'NONE',  ( -1.000000000000000000, -0.000000000000000000, 0.000000000000000000 ) ) ;
#34164 = DIRECTION ( 'NONE',  ( -1.000000000000000000, 0.000000000000000000, 0.000000000000000000 ) ) ;
#34165 = CARTESIAN_POINT ( 'NONE',  ( 0.000000000000000000, -81.50828551894220197, -8.966570791701586884 ) ) ;
#34166 = FACE_OUTER_BOUND ( 'NONE', #17955, .T. ) ;
#34167 = DIRECTION ( 'NONE',  ( 0.000000000000000000, 0.000000000000000000, 1.000000000000000000 ) ) ;
#34168 = DIRECTION ( 'NONE',  ( 0.000000000000000000, -0.4999999999999913403, -0.8660254037844435926 ) ) ;
#34169 = DIRECTION ( 'NONE',  ( 0.000000000000000000, 0.000000000000000000, -1.000000000000000000 ) ) ;
#34170 = DIRECTION ( 'NONE',  ( 0.000000000000000000, 0.000000000000000000, -1.000000000000000000 ) ) ;
#34171 = VERTEX_POINT ( 'NONE', #15235 ) ;
#34172 = CIRCLE ( 'NONE', #1343, 11.59999999999999964 ) ;
#34173 = CYLINDRICAL_SURFACE ( 'NONE', #31413, 77.49899999999999523 ) ;
#34174 = EDGE_CURVE ( 'NONE', #37702, #23496, #44356, .T. ) ;
#34175 = VERTEX_POINT ( 'NONE', #11559 ) ;
#34176 = ORIENTED_EDGE ( 'NONE', *, *, #48208, .T. ) ;
#34177 = CARTESIAN_POINT ( 'NONE',  ( 10.00000000000000000, 6.903761155838878061, -77.19088730480517313 ) ) ;
#34178 = DIRECTION ( 'NONE',  ( -1.000000000000000000, 0.000000000000000000, -0.000000000000000000 ) ) ;
#34179 = CYLINDRICAL_SURFACE ( 'NONE', #42355, 31.99999999999999289 ) ;
#34180 = CARTESIAN_POINT ( 'NONE',  ( 0.000000000000000000, 0.000000000000000000, 0.000000000000000000 ) ) ;
#34181 = ADVANCED_FACE ( 'NONE', ( #48266 ), #4213, .F. ) ;
#34182 = DIRECTION ( 'NONE',  ( 0.000000000000000000, 0.000000000000000000, 1.000000000000000000 ) ) ;
#34183 = DIRECTION ( 'NONE',  ( -1.000000000000000000, -0.000000000000000000, -0.000000000000000000 ) ) ;
#34184 = EDGE_CURVE ( 'NONE', #33636, #15030, #21830, .T. ) ;
#34185 = AXIS2_PLACEMENT_3D ( 'NONE', #19174, #38030, #30673 ) ;
#34186 = DIRECTION ( 'NONE',  ( 0.000000000000000000, -0.5877852522924802425, 0.8090169943749422332 ) ) ;
#34187 = DIRECTION ( 'NONE',  ( 0.000000000000000000, 0.000000000000000000, 1.000000000000000000 ) ) ;
#34188 = DIRECTION ( 'NONE',  ( 0.000000000000000000, 0.000000000000000000, -1.000000000000000000 ) ) ;
#34189 = ORIENTED_EDGE ( 'NONE', *, *, #4090, .T. ) ;
#34190 = VERTEX_POINT ( 'NONE', #7395 ) ;
#34191 = VECTOR ( 'NONE', #11795, 1000.000000000000000 ) ;
#34192 = ADVANCED_FACE ( 'NONE', ( #22334 ), #29433, .T. ) ;
#34193 = ORIENTED_EDGE ( 'NONE', *, *, #40462, .F. ) ;
#34194 = ORIENTED_EDGE ( 'NONE', *, *, #5950, .T. ) ;
#34195 = ORIENTED_EDGE ( 'NONE', *, *, #25405, .T. ) ;
#34196 = CARTESIAN_POINT ( 'NONE',  ( -10.00000000000000000, 0.000000000000000000, 0.000000000000000000 ) ) ;
#34197 = EDGE_CURVE ( 'NONE', #36905, #28265, #14745, .T. ) ;
#34198 = CARTESIAN_POINT ( 'NONE',  ( -3.000000000000000000, 24.81905959214275370, -9.408202855044498492 ) ) ;
#34199 = VERTEX_POINT ( 'NONE', #11067 ) ;
#34200 = VECTOR ( 'NONE', #2007, 1000.000000000000000 ) ;
#34201 = EDGE_CURVE ( 'NONE', #26799, #42769, #19839, .T. ) ;
#34202 = DIRECTION ( 'NONE',  ( -1.000000000000000000, 0.000000000000000000, -0.000000000000000000 ) ) ;
#34203 = ORIENTED_EDGE ( 'NONE', *, *, #23677, .T. ) ;
#34204 = EDGE_CURVE ( 'NONE', #23962, #39152, #30402, .T. ) ;
#34205 = EDGE_LOOP ( 'NONE', ( #29418, #45472, #29591, #16416 ) ) ;
#34206 = DIRECTION ( 'NONE',  ( -1.000000000000000000, -0.000000000000000000, -0.000000000000000000 ) ) ;
#34207 = CARTESIAN_POINT ( 'NONE',  ( -3.000000000000000000, 8.688484142254221609, -21.88630264137359660 ) ) ;
#34208 = CIRCLE ( 'NONE', #16989, 31.99999999999998579 ) ;
#34209 = DIRECTION ( 'NONE',  ( -1.000000000000000000, 0.000000000000000000, -0.000000000000000000 ) ) ;
#34210 = VERTEX_POINT ( 'NONE', #12521 ) ;
#34211 = CARTESIAN_POINT ( 'NONE',  ( 10.00000000000000000, 27.13269053701132094, -25.88420570971372570 ) ) ;
#34212 = ORIENTED_EDGE ( 'NONE', *, *, #46, .T. ) ;
#34213 = ORIENTED_EDGE ( 'NONE', *, *, #42992, .T. ) ;
#34214 = CARTESIAN_POINT ( 'NONE',  ( 5.000000000000000000, 22.48208911017551870, -35.47612816024499693 ) ) ;
#34215 = AXIS2_PLACEMENT_3D ( 'NONE', #1871, #19978, #47779 ) ;
#34216 = DIRECTION ( 'NONE',  ( 0.000000000000000000, 0.7604059656000276002, 0.6494480483301876550 ) ) ;
#34217 = DIRECTION ( 'NONE',  ( 1.000000000000000000, 0.000000000000000000, 0.000000000000000000 ) ) ;
#34218 = AXIS2_PLACEMENT_3D ( 'NONE', #16113, #34934, #31046 ) ;
#34219 = ORIENTED_EDGE ( 'NONE', *, *, #18778, .F. ) ;
#34220 = ORIENTED_EDGE ( 'NONE', *, *, #21305, .T. ) ;
#34221 =( NAMED_UNIT ( * ) PLANE_ANGLE_UNIT ( ) SI_UNIT ( $, .RADIAN. ) );
#34222 = FACE_OUTER_BOUND ( 'NONE', #5332, .T. ) ;
#34223 = ORIENTED_EDGE ( 'NONE', *, *, #41610, .T. ) ;
#34224 = LINE ( 'NONE', #205, #44722 ) ;
#34225 = ORIENTED_EDGE ( 'NONE', *, *, #35238, .F. ) ;
#34226 = CARTESIAN_POINT ( 'NONE',  ( 0.000000000000000000, 37.58145647212453611, 16.68533520207917675 ) ) ;
#34227 = CARTESIAN_POINT ( 'NONE',  ( 0.000000000000000000, 0.000000000000000000, 0.000000000000000000 ) ) ;
#34228 = DIRECTION ( 'NONE',  ( 0.000000000000000000, 0.000000000000000000, -1.000000000000000000 ) ) ;
#34229 = CARTESIAN_POINT ( 'NONE',  ( 4.999999999999999112, 41.81611651403868990, -3.925862922255709542 ) ) ;
#34230 = COLOUR_RGB ( '', 0.40784314, 0.44705882, 0.49803922) ;
#34231 = DIRECTION ( 'NONE',  ( -1.000000000000000000, -0.000000000000000000, 0.000000000000000000 ) ) ;
#34232 = CARTESIAN_POINT ( 'NONE',  ( 23.30762065077924916, -123.0008031590507329, -2.500000000000000000 ) ) ;
#34233 = DIRECTION ( 'NONE',  ( 1.000000000000000000, 0.000000000000000000, 0.000000000000000000 ) ) ;
#34234 = DIRECTION ( 'NONE',  ( 0.000000000000000000, 0.000000000000000000, 1.000000000000000000 ) ) ;
#34235 = LINE ( 'NONE', #15646, #16045 ) ;
#34236 = ORIENTED_EDGE ( 'NONE', *, *, #43394, .T. ) ;
#34237 = EDGE_CURVE ( 'NONE', #30209, #38886, #20040, .T. ) ;
#34238 = DIRECTION ( 'NONE',  ( 0.000000000000000000, 0.000000000000000000, 1.000000000000000000 ) ) ;
#34239 = PLANE ( 'NONE',  #42628 ) ;
#34240 = FACE_OUTER_BOUND ( 'NONE', #48404, .T. ) ;
#34241 = ORIENTED_EDGE ( 'NONE', *, *, #33137, .F. ) ;
#34242 = CARTESIAN_POINT ( 'NONE',  ( -10.00000000000000000, 0.000000000000000000, 0.000000000000000000 ) ) ;
#34243 = AXIS2_PLACEMENT_3D ( 'NONE', #6782, #20749, #28322 ) ;
#34244 = ORIENTED_EDGE ( 'NONE', *, *, #22036, .T. ) ;
#34245 = CARTESIAN_POINT ( 'NONE',  ( 10.00000000000000000, -20.40083707022935400, 72.35432306680478121 ) ) ;
#34246 = ADVANCED_FACE ( 'NONE', ( #1001 ), #45313, .T. ) ;
#34247 = CARTESIAN_POINT ( 'NONE',  ( 5.000000000000000000, -21.40280677340398086, 36.13751322684410638 ) ) ;
#34248 = ORIENTED_EDGE ( 'NONE', *, *, #46822, .F. ) ;
#34249 = ADVANCED_FACE ( 'NONE', ( #15699 ), #8110, .T. ) ;
#34250 = ADVANCED_FACE ( 'NONE', ( #19363 ), #30634, .T. ) ;
#34251 = ORIENTED_EDGE ( 'NONE', *, *, #42609, .T. ) ;
#34252 = EDGE_CURVE ( 'NONE', #27123, #26989, #26723, .T. ) ;
#34253 = CARTESIAN_POINT ( 'NONE',  ( 32.50000000000000000, -120.0000000000000000, 2.500000000000000000 ) ) ;
#34254 = ORIENTED_EDGE ( 'NONE', *, *, #30206, .F. ) ;
#34255 = ORIENTED_EDGE ( 'NONE', *, *, #4595, .F. ) ;
#34256 = ADVANCED_FACE ( 'NONE', ( #26972, #4684 ), #23764, .F. ) ;
#34257 = VERTEX_POINT ( 'NONE', #27691 ) ;
#34258 =( GEOMETRIC_REPRESENTATION_CONTEXT ( 3 ) GLOBAL_UNCERTAINTY_ASSIGNED_CONTEXT ( ( #29125 ) ) GLOBAL_UNIT_ASSIGNED_CONTEXT ( ( #48040, #18428, #3007 ) ) REPRESENTATION_CONTEXT ( 'NONE', 'WORKASPACE' ) );
#34259 = AXIS2_PLACEMENT_3D ( 'NONE', #15478, #19601, #45828 ) ;
#34260 = DIRECTION ( 'NONE',  ( -1.000000000000000000, -0.000000000000000000, 0.000000000000000000 ) ) ;
#34261 = ORIENTED_EDGE ( 'NONE', *, *, #32462, .T. ) ;
#34262 = DIRECTION ( 'NONE',  ( -1.000000000000000000, 0.000000000000000000, -0.000000000000000000 ) ) ;
#34263 = ORIENTED_EDGE ( 'NONE', *, *, #13915, .F. ) ;
#34264 = DIRECTION ( 'NONE',  ( -1.000000000000000000, 0.000000000000000000, 0.000000000000000000 ) ) ;
#34265 = ORIENTED_EDGE ( 'NONE', *, *, #6916, .F. ) ;
#34266 = CARTESIAN_POINT ( 'NONE',  ( -10.00000000000000000, 0.000000000000000000, 0.000000000000000000 ) ) ;
#34267 = CARTESIAN_POINT ( 'NONE',  ( 0.000000000000000000, 65.64334221924909230, 41.19522573413756561 ) ) ;
#34268 = ORIENTED_EDGE ( 'NONE', *, *, #26607, .F. ) ;
#34269 = CARTESIAN_POINT ( 'NONE',  ( 11.99999999999999822, 0.000000000000000000, 0.000000000000000000 ) ) ;
#34270 = ORIENTED_EDGE ( 'NONE', *, *, #11939, .T. ) ;
#34271 = EDGE_CURVE ( 'NONE', #46234, #29434, #44291, .T. ) ;
#34273 = ORIENTED_EDGE ( 'NONE', *, *, #42942, .F. ) ;
#34272 = DIRECTION ( 'NONE',  ( -0.000000000000000000, -0.000000000000000000, 1.000000000000000000 ) ) ;
#34274 = DIRECTION ( 'NONE',  ( 0.000000000000000000, 0.000000000000000000, 1.000000000000000000 ) ) ;
#34275 = ORIENTED_EDGE ( 'NONE', *, *, #10331, .F. ) ;
#34276 = FACE_OUTER_BOUND ( 'NONE', #4948, .T. ) ;
#34277 = ORIENTED_EDGE ( 'NONE', *, *, #6367, .F. ) ;
#34278 = DIRECTION ( 'NONE',  ( 0.000000000000000000, 0.000000000000000000, -1.000000000000000000 ) ) ;
#34279 = FACE_OUTER_BOUND ( 'NONE', #33180, .T. ) ;
#34280 = ORIENTED_EDGE ( 'NONE', *, *, #28083, .F. ) ;
#34281 = AXIS2_PLACEMENT_3D ( 'NONE', #16384, #46246, #46967 ) ;
#34282 = CARTESIAN_POINT ( 'NONE',  ( -43.60332556124591719, -117.0000000000000000, -2.500000000000000000 ) ) ;
#34283 = FACE_OUTER_BOUND ( 'NONE', #3217, .T. ) ;
#34284 = CYLINDRICAL_SURFACE ( 'NONE', #11244, 82.00000000000000000 ) ;
#34285 = CIRCLE ( 'NONE', #46789, 0.9999999999999991118 ) ;
#34286 = CARTESIAN_POINT ( 'NONE',  ( 10.00000000000000000, -22.74946021919153694, 29.81001611431000597 ) ) ;
#34287 = DIRECTION ( 'NONE',  ( 0.000000000000000000, 0.000000000000000000, -1.000000000000000000 ) ) ;
#34288 = DIRECTION ( 'NONE',  ( -1.000000000000000000, 0.000000000000000000, -0.000000000000000000 ) ) ;
#34289 = VERTEX_POINT ( 'NONE', #15947 ) ;
#34290 = ADVANCED_FACE ( 'NONE', ( #1503 ), #23517, .T. ) ;
#34291 = LINE ( 'NONE', #4686, #2792 ) ;
#34292 = DIRECTION ( 'NONE',  ( 0.000000000000000000, 0.000000000000000000, 1.000000000000000000 ) ) ;
#34293 = CARTESIAN_POINT ( 'NONE',  ( 10.00000000000000000, 22.74946021919133088, 29.81001611431016229 ) ) ;
#34294 = ORIENTED_EDGE ( 'NONE', *, *, #9279, .F. ) ;
#34295 = EDGE_CURVE ( 'NONE', #9289, #28089, #34120, .T. ) ;
#34296 = CARTESIAN_POINT ( 'NONE',  ( 10.00000000000000000, -17.80606268964516659, -33.00180498840066434 ) ) ;
#34297 = FACE_OUTER_BOUND ( 'NONE', #7161, .T. ) ;
#34298 = EDGE_LOOP ( 'NONE', ( #37568, #39601, #41805, #43012 ) ) ;
#34299 = CARTESIAN_POINT ( 'NONE',  ( 10.00000000000000000, 8.840884882375075193, 74.65374052328651544 ) ) ;
#34300 = CYLINDRICAL_SURFACE ( 'NONE', #10024, 31.99999999999999289 ) ;
#34301 = EDGE_CURVE ( 'NONE', #16579, #15125, #42626, .T. ) ;
#34302 = ORIENTED_EDGE ( 'NONE', *, *, #45252, .F. ) ;
#34303 = DIRECTION ( 'NONE',  ( -0.000000000000000000, 0.000000000000000000, 1.000000000000000000 ) ) ;
#34304 = ORIENTED_EDGE ( 'NONE', *, *, #30182, .T. ) ;
#34305 = CYLINDRICAL_SURFACE ( 'NONE', #22882, 77.49899999999999523 ) ;
#34306 = PRODUCT_CONTEXT ( 'NONE', #14148, 'mechanical' ) ;
#34307 = CARTESIAN_POINT ( 'NONE',  ( 22.94323693612312809, -114.6983135802921083, 5.500000000000000000 ) ) ;
#34308 = EDGE_LOOP ( 'NONE', ( #28754, #13138, #10095, #26019 ) ) ;
#34309 = EDGE_CURVE ( 'NONE', #8338, #29506, #12264, .T. ) ;
#34310 = EDGE_CURVE ( 'NONE', #44612, #47223, #27116, .T. ) ;
#34311 = CARTESIAN_POINT ( 'NONE',  ( 10.00000000000000000, -10.74501242461308159, 35.92658777277507909 ) ) ;
#34312 = VECTOR ( 'NONE', #21908, 1000.000000000000000 ) ;
#34313 = ORIENTED_EDGE ( 'NONE', *, *, #46853, .F. ) ;
#34314 = AXIS2_PLACEMENT_3D ( 'NONE', #43674, #14552, #39540 ) ;
#34315 = EDGE_CURVE ( 'NONE', #44874, #46424, #41158, .T. ) ;
#34316 = CARTESIAN_POINT ( 'NONE',  ( 10.00000000000000000, -17.80606268964516659, -33.00180498840066434 ) ) ;
#34317 = CARTESIAN_POINT ( 'NONE',  ( 10.00000000000000000, -62.50329211542465657, 41.76937507738766442 ) ) ;
#34319 = ORIENTED_EDGE ( 'NONE', *, *, #46084, .T. ) ;
#34318 = CARTESIAN_POINT ( 'NONE',  ( 10.00000000000000178, 1.530808498934191521E-15, -12.50000000000000000 ) ) ;
#34320 = EDGE_LOOP ( 'NONE', ( #28232, #43830, #42148, #12794 ) ) ;
#34321 = DIRECTION ( 'NONE',  ( -1.000000000000000000, 0.000000000000000000, 0.000000000000000000 ) ) ;
#34322 = CYLINDRICAL_SURFACE ( 'NONE', #44464, 31.99999999999998579 ) ;
#34323 = CARTESIAN_POINT ( 'NONE',  ( 10.00000000000000000, 29.81001611431041098, -22.74946021919100403 ) ) ;
#34324 = CYLINDRICAL_SURFACE ( 'NONE', #3084, 16.00000000000000000 ) ;
#34325 = ORIENTED_EDGE ( 'NONE', *, *, #42005, .F. ) ;
#34326 = CARTESIAN_POINT ( 'NONE',  ( 6.000000000000000000, -76.69515212745996280, -29.01471420065643869 ) ) ;
#34327 = EDGE_LOOP ( 'NONE', ( #19198, #3434, #21854, #14352 ) ) ;
#34328 = ORIENTED_EDGE ( 'NONE', *, *, #44864, .F. ) ;
#34329 = CYLINDRICAL_SURFACE ( 'NONE', #32494, 77.49899999999999523 ) ;
#34330 = ORIENTED_EDGE ( 'NONE', *, *, #30472, .F. ) ;
#34331 = CARTESIAN_POINT ( 'NONE',  ( -3.000000000000000000, -22.67460108101774807, -6.353146135318215038 ) ) ;
#34332 = DIRECTION ( 'NONE',  ( 0.000000000000000000, -0.9510565162951566398, 0.3090169943749381809 ) ) ;
#34333 = DIRECTION ( 'NONE',  ( -0.000000000000000000, -0.000000000000000000, -1.000000000000000000 ) ) ;
#34334 = ORIENTED_EDGE ( 'NONE', *, *, #29933, .T. ) ;
#34335 = DIRECTION ( 'NONE',  ( -1.000000000000000000, 0.000000000000000000, 0.000000000000000000 ) ) ;
#34336 = CYLINDRICAL_SURFACE ( 'NONE', #25219, 16.00000000000000000 ) ;
#34338 = EDGE_CURVE ( 'NONE', #10794, #2137, #16148, .T. ) ;
#34337 = CARTESIAN_POINT ( 'NONE',  ( 0.000000000000000000, 73.44644590900092851, -24.73286445877629092 ) ) ;
#34339 = DIRECTION ( 'NONE',  ( 0.000000000000000000, 0.000000000000000000, 1.000000000000000000 ) ) ;
#34341 = VECTOR ( 'NONE', #38221, 1000.000000000000000 ) ;
#34340 = DIRECTION ( 'NONE',  ( 0.000000000000000000, 0.000000000000000000, -1.000000000000000000 ) ) ;
#34342 = ADVANCED_FACE ( 'NONE', ( #19127 ), #23046, .T. ) ;
#34343 = VECTOR ( 'NONE', #9459, 1000.000000000000000 ) ;
#34344 = CARTESIAN_POINT ( 'NONE',  ( 0.000000000000000000, 2.571758278209441661E-15, -21.00000000000000000 ) ) ;
#34345 = CARTESIAN_POINT ( 'NONE',  ( 15.00000000000000000, -20.55727247249748402, -16.78983467731284307 ) ) ;
#34346 = CYLINDRICAL_SURFACE ( 'NONE', #5990, 37.49900000000000233 ) ;
#34348 = EDGE_CURVE ( 'NONE', #36067, #39062, #13473, .T. ) ;
#34347 = AXIS2_PLACEMENT_3D ( 'NONE', #3561, #7484, #7227 ) ;
#34349 = CARTESIAN_POINT ( 'NONE',  ( 11.99999999999999822, -65.58780272294048075, -36.73666225445966660 ) ) ;
#34350 = DIRECTION ( 'NONE',  ( -1.000000000000000000, 0.000000000000000000, -0.000000000000000000 ) ) ;
#34351 = ADVANCED_FACE ( 'NONE', ( #17369 ), #5904, .T. ) ;
#34352 = DIRECTION ( 'NONE',  ( 0.000000000000000000, 0.3090169943749410675, 0.9510565162951556406 ) ) ;
#34353 = ORIENTED_EDGE ( 'NONE', *, *, #38, .F. ) ;
#34354 = DIRECTION ( 'NONE',  ( 0.000000000000000000, 0.000000000000000000, 1.000000000000000000 ) ) ;
#34355 = DIRECTION ( 'NONE',  ( 0.000000000000000000, 0.000000000000000000, 1.000000000000000000 ) ) ;
#34356 = DIRECTION ( 'NONE',  ( -1.000000000000000000, 0.000000000000000000, 0.000000000000000000 ) ) ;
#34357 = EDGE_LOOP ( 'NONE', ( #32304, #44213, #44454, #4534 ) ) ;
#34358 = DIRECTION ( 'NONE',  ( -1.000000000000000000, 0.000000000000000000, 0.000000000000000000 ) ) ;
#34359 = VERTEX_POINT ( 'NONE', #9799 ) ;
#34360 = ADVANCED_FACE ( 'NONE', ( #17140 ), #16910, .F. ) ;
#34361 = EDGE_CURVE ( 'NONE', #22636, #4251, #41971, .T. ) ;
#34362 = ADVANCED_FACE ( 'NONE', ( #35262 ), #17619, .T. ) ;
#34363 = VERTEX_POINT ( 'NONE', #32088 ) ;
#34364 = ORIENTED_EDGE ( 'NONE', *, *, #10342, .T. ) ;
#34365 = CARTESIAN_POINT ( 'NONE',  ( -32.50000000000000000, -120.0000000000000000, -2.500000000000000000 ) ) ;
#34366 = ORIENTED_EDGE ( 'NONE', *, *, #39351, .F. ) ;
#34367 = EDGE_CURVE ( 'NONE', #35720, #11988, #46644, .T. ) ;
#34368 = CIRCLE ( 'NONE', #24218, 31.99999999999999289 ) ;
#34369 = DIRECTION ( 'NONE',  ( 0.000000000000000000, -0.4067366430758010409, 0.9135454576426005335 ) ) ;
#34370 = AXIS2_PLACEMENT_3D ( 'NONE', #20182, #12852, #9168 ) ;
#34371 = CARTESIAN_POINT ( 'NONE',  ( 0.000000000000000000, 54.21277698773675979, 55.38113227695801299 ) ) ;
#34372 = DIRECTION ( 'NONE',  ( 0.000000000000000000, 0.000000000000000000, -1.000000000000000000 ) ) ;
#34373 = CIRCLE ( 'NONE', #10180, 16.00000000000000000 ) ;
#34374 = ORIENTED_EDGE ( 'NONE', *, *, #20264, .T. ) ;
#34375 = LINE ( 'NONE', #34616, #18759 ) ;
#34376 = ORIENTED_EDGE ( 'NONE', *, *, #16904, .T. ) ;
#34377 = ORIENTED_EDGE ( 'NONE', *, *, #34412, .F. ) ;
#34378 = AXIS2_PLACEMENT_3D ( 'NONE', #7114, #10557, #6399 ) ;
#34379 = CARTESIAN_POINT ( 'NONE',  ( 10.00000000000000000, -36.73666225445940370, 65.58780272294062286 ) ) ;
#34380 = DIRECTION ( 'NONE',  ( 0.000000000000000000, -0.9510565162951510887, 0.3090169943749551673 ) ) ;
#34381 = ORIENTED_EDGE ( 'NONE', *, *, #13097, .F. ) ;
#34382 = EDGE_LOOP ( 'NONE', ( #4859, #27293, #46776, #29290 ) ) ;
#34383 = AXIS2_PLACEMENT_3D ( 'NONE', #13996, #40661, #18129 ) ;
#34384 = CARTESIAN_POINT ( 'NONE',  ( 0.000000000000000000, -3.894527615418457600, 81.90746397400387480 ) ) ;
#34385 = ORIENTED_EDGE ( 'NONE', *, *, #29221, .T. ) ;
#34386 = CARTESIAN_POINT ( 'NONE',  ( 0.000000000000000000, 16.83928648764945279, -16.46020748918028076 ) ) ;
#34387 = DIRECTION ( 'NONE',  ( -1.000000000000000000, -0.000000000000000000, -0.000000000000000000 ) ) ;
#34388 = CARTESIAN_POINT ( 'NONE',  ( 0.000000000000000000, 0.000000000000000000, 0.000000000000000000 ) ) ;
#34389 = CARTESIAN_POINT ( 'NONE',  ( 0.000000000000000000, 0.8828120875905820508, -37.48860685352290290 ) ) ;
#34390 = CARTESIAN_POINT ( 'NONE',  ( -70.53423027509626309, -217.0820393249940423, -5.500000000000000000 ) ) ;
#34391 = CARTESIAN_POINT ( 'NONE',  ( 0.000000000000000000, 5.202137450156389953, 37.22597642581160216 ) ) ;
#34392 = CARTESIAN_POINT ( 'NONE',  ( 10.00000000000000000, 25.88420570971438650, -27.13269053701069566 ) ) ;
#34393 = CARTESIAN_POINT ( 'NONE',  ( 10.00000000000000000, 44.88180994100468268, -63.18004540532978552 ) ) ;
#34394 = DIRECTION ( 'NONE',  ( 0.000000000000000000, 0.000000000000000000, -1.000000000000000000 ) ) ;
#34395 = CARTESIAN_POINT ( 'NONE',  ( -3.759344165985237129, 2.343521743652961183E-15, 19.05560546998412974 ) ) ;
#34396 = ORIENTED_EDGE ( 'NONE', *, *, #42563, .F. ) ;
#34397 = ORIENTED_EDGE ( 'NONE', *, *, #32067, .F. ) ;
#34398 = DIRECTION ( 'NONE',  ( 0.000000000000000000, 0.3090169943749461745, -0.9510565162951539753 ) ) ;
#34399 = EDGE_CURVE ( 'NONE', #37878, #6565, #23186, .T. ) ;
#34400 = CARTESIAN_POINT ( 'NONE',  ( 0.000000000000000000, 0.000000000000000000, -5.500000000000000000 ) ) ;
#34401 = CARTESIAN_POINT ( 'NONE',  ( 0.000000000000000000, 0.000000000000000000, 0.000000000000000000 ) ) ;
#34402 = CARTESIAN_POINT ( 'NONE',  ( -12.40464318976452596, 10.41032311384371489, 42.00000000000001421 ) ) ;
#34403 = EDGE_CURVE ( 'NONE', #36833, #24283, #24491, .T. ) ;
#34404 = ADVANCED_FACE ( 'NONE', ( #24246 ), #47484, .T. ) ;
#34405 = FACE_OUTER_BOUND ( 'NONE', #18805, .T. ) ;
#34406 = CARTESIAN_POINT ( 'NONE',  ( 10.00000000000000000, -26.08949754953005495, -27.05870788708258701 ) ) ;
#34407 = EDGE_CURVE ( 'NONE', #46450, #2889, #43346, .T. ) ;
#34408 = CIRCLE ( 'NONE', #42254, 16.00000000000000000 ) ;
#34409 = CARTESIAN_POINT ( 'NONE',  ( 0.000000000000000000, -63.97538442413463855, 51.29473840253199768 ) ) ;
#34410 = DIRECTION ( 'NONE',  ( 0.000000000000000000, -0.9510565162951565288, 0.3090169943749384029 ) ) ;
#34411 = AXIS2_PLACEMENT_3D ( 'NONE', #42051, #22954, #15857 ) ;
#34412 = EDGE_CURVE ( 'NONE', #19565, #32725, #28647, .T. ) ;
#34413 = CIRCLE ( 'NONE', #32105, 16.00000000000000000 ) ;
#34414 = AXIS2_PLACEMENT_3D ( 'NONE', #1235, #4892, #8796 ) ;
#34415 = SURFACE_STYLE_FILL_AREA ( #23412 ) ;
#34416 = FACE_OUTER_BOUND ( 'NONE', #14397, .T. ) ;
#34417 = MECHANICAL_DESIGN_GEOMETRIC_PRESENTATION_REPRESENTATION (  '', ( #7879 ), #26646 ) ;
#34418 = ORIENTED_EDGE ( 'NONE', *, *, #5988, .F. ) ;
#34419 = ADVANCED_FACE ( 'NONE', ( #28652 ), #32562, .F. ) ;
#34420 = AXIS2_PLACEMENT_3D ( 'NONE', #11786, #41179, #11554 ) ;
#34421 = VERTEX_POINT ( 'NONE', #20322 ) ;
#34422 = AXIS2_PLACEMENT_3D ( 'NONE', #26465, #34272, #31359 ) ;
#34423 = ADVANCED_FACE ( 'NONE', ( #10037 ), #13240, .T. ) ;
#34424 = ORIENTED_EDGE ( 'NONE', *, *, #47846, .F. ) ;
#34425 = ORIENTED_EDGE ( 'NONE', *, *, #25776, .T. ) ;
#34426 = CARTESIAN_POINT ( 'NONE',  ( 14.59956846177685996, -138.4757300459248484, 5.500000000000000000 ) ) ;
#34427 = EDGE_LOOP ( 'NONE', ( #11427, #6837, #1701, #394 ) ) ;
#34428 = ORIENTED_EDGE ( 'NONE', *, *, #2118, .F. ) ;
#34429 = EDGE_CURVE ( 'NONE', #31590, #34673, #1994, .T. ) ;
#34430 = CARTESIAN_POINT ( 'NONE',  ( 10.00000000000000000, -33.80338159004273280, -16.23288003029533044 ) ) ;
#34431 = ORIENTED_EDGE ( 'NONE', *, *, #11715, .T. ) ;
#34432 = ORIENTED_EDGE ( 'NONE', *, *, #36370, .T. ) ;
#34433 = CARTESIAN_POINT ( 'NONE',  ( 15.00000000000000000, 16.83928648764922542, -16.46020748918050458 ) ) ;
#34435 = ORIENTED_EDGE ( 'NONE', *, *, #19673, .T. ) ;
#34434 = DIRECTION ( 'NONE',  ( -1.000000000000000000, 0.000000000000000000, 0.000000000000000000 ) ) ;
#34436 = ADVANCED_FACE ( 'NONE', ( #43095 ), #9548, .T. ) ;
#34437 = FACE_OUTER_BOUND ( 'NONE', #38802, .T. ) ;
#34439 = ORIENTED_EDGE ( 'NONE', *, *, #21868, .T. ) ;
#34438 = CIRCLE ( 'NONE', #11793, 31.99999999999998579 ) ;
#34440 = CARTESIAN_POINT ( 'NONE',  ( 2.500000000000000444, 8.494897427831771708, 0.000000000000000000 ) ) ;
#34441 = ORIENTED_EDGE ( 'NONE', *, *, #7233, .F. ) ;
#34442 = VERTEX_POINT ( 'NONE', #2934 ) ;
#34443 = CARTESIAN_POINT ( 'NONE',  ( 10.00000000000000000, 0.000000000000000000, 0.000000000000000000 ) ) ;
#34444 = VECTOR ( 'NONE', #18690, 1000.000000000000000 ) ;
#34445 = CIRCLE ( 'NONE', #25859, 31.99999999999999289 ) ;
#34446 = DIRECTION ( 'NONE',  ( -1.000000000000000000, 0.000000000000000000, -0.000000000000000000 ) ) ;
#34447 = ORIENTED_EDGE ( 'NONE', *, *, #44024, .T. ) ;
#34448 = CYLINDRICAL_SURFACE ( 'NONE', #40100, 37.49900000000000233 ) ;
#34449 = DIRECTION ( 'NONE',  ( 1.000000000000000000, -0.000000000000000000, -0.000000000000000000 ) ) ;
#34450 = VERTEX_POINT ( 'NONE', #3161 ) ;
#34451 = AXIS2_PLACEMENT_3D ( 'NONE', #4858, #1436, #16134 ) ;
#34452 = ORIENTED_EDGE ( 'NONE', *, *, #39558, .T. ) ;
#34453 = AXIS2_PLACEMENT_3D ( 'NONE', #18338, #25670, #472 ) ;
#34455 = EDGE_CURVE ( 'NONE', #919, #9826, #48202, .T. ) ;
#34454 = DIRECTION ( 'NONE',  ( 0.000000000000000000, 0.000000000000000000, 1.000000000000000000 ) ) ;
#34456 = DIRECTION ( 'NONE',  ( -1.000000000000000000, -0.000000000000000000, -0.000000000000000000 ) ) ;
#34457 = ORIENTED_EDGE ( 'NONE', *, *, #26329, .T. ) ;
#34458 = AXIS2_PLACEMENT_3D ( 'NONE', #33984, #12217, #30558 ) ;
#34459 = ADVANCED_FACE ( 'NONE', ( #18089 ), #36467, .F. ) ;
#34460 = FACE_OUTER_BOUND ( 'NONE', #5568, .T. ) ;
#34461 = EDGE_LOOP ( 'NONE', ( #2294, #29693, #29738, #10437 ) ) ;
#34462 = LINE ( 'NONE', #30336, #36344 ) ;
#34463 = CARTESIAN_POINT ( 'NONE',  ( 0.000000000000000000, -79.10210256391383155, 21.60688246758557796 ) ) ;
#34464 = CARTESIAN_POINT ( 'NONE',  ( -0.2999999999999947153, 0.000000000000000000, 0.000000000000000000 ) ) ;
#34465 = DIRECTION ( 'NONE',  ( 0.000000000000000000, 0.000000000000000000, -1.000000000000000000 ) ) ;
#34466 = CARTESIAN_POINT ( 'NONE',  ( 10.00000000000000000, -35.92658777277517856, 10.74501242461269257 ) ) ;
#34467 = EDGE_CURVE ( 'NONE', #9308, #20063, #7543, .T. ) ;
#34468 = CARTESIAN_POINT ( 'NONE',  ( 11.99999999999999822, -77.19088730480528682, 6.903761155837505825 ) ) ;
#34469 = LINE ( 'NONE', #217, #21605 ) ;
#34470 = CARTESIAN_POINT ( 'NONE',  ( 10.00000000000000000, 0.000000000000000000, 0.000000000000000000 ) ) ;
#34471 = EDGE_CURVE ( 'NONE', #41935, #19037, #32556, .T. ) ;
#34472 = DIRECTION ( 'NONE',  ( -1.000000000000000000, -0.000000000000000000, -0.000000000000000000 ) ) ;
#34473 = FILL_AREA_STYLE_COLOUR ( '', #28825 ) ;
#34474 = CARTESIAN_POINT ( 'NONE',  ( 11.99999999999999822, -62.50329211542465657, 41.76937507738766442 ) ) ;
#34475 = ORIENTED_EDGE ( 'NONE', *, *, #2306, .T. ) ;
#34476 = VERTEX_POINT ( 'NONE', #33278 ) ;
#34477 = AXIS2_PLACEMENT_3D ( 'NONE', #5708, #13530, #20631 ) ;
#34478 = AXIS2_PLACEMENT_3D ( 'NONE', #43451, #17475, #36087 ) ;
#34479 = UNCERTAINTY_MEASURE_WITH_UNIT (LENGTH_MEASURE( 1.000000000000000082E-05 ), #37118, 'distance_accuracy_value', 'NONE');
#34480 = DIRECTION ( 'NONE',  ( 0.000000000000000000, 0.000000000000000000, 1.000000000000000000 ) ) ;
#34481 = ORIENTED_EDGE ( 'NONE', *, *, #13861, .T. ) ;
#34482 = AXIS2_PLACEMENT_3D ( 'NONE', #31846, #13224, #13706 ) ;
#34483 = CIRCLE ( 'NONE', #20403, 31.99999999999999645 ) ;
#34484 = PLANE ( 'NONE',  #8860 ) ;
#34485 = LINE ( 'NONE', #7595, #23741 ) ;
#34486 = ORIENTED_EDGE ( 'NONE', *, *, #8759, .F. ) ;
#34487 = AXIS2_PLACEMENT_3D ( 'NONE', #42553, #15627, #20263 ) ;
#34488 = ORIENTED_EDGE ( 'NONE', *, *, #32448, .F. ) ;
#34489 = AXIS2_PLACEMENT_3D ( 'NONE', #335, #27025, #15513 ) ;
#34490 = CARTESIAN_POINT ( 'NONE',  ( 10.00000000000000000, -17.28742895386139722, 75.54627589209937355 ) ) ;
#34491 = CIRCLE ( 'NONE', #23568, 37.49900000000001654 ) ;
#34492 = VERTEX_POINT ( 'NONE', #6856 ) ;
#34493 = EDGE_LOOP ( 'NONE', ( #31242, #34565, #41145, #19864 ) ) ;
#34494 = ORIENTED_EDGE ( 'NONE', *, *, #31031, .F. ) ;
#34495 = VERTEX_POINT ( 'NONE', #3661 ) ;
#34496 = CARTESIAN_POINT ( 'NONE',  ( 10.00000000000000000, 0.000000000000000000, 0.000000000000000000 ) ) ;
#34497 = ORIENTED_EDGE ( 'NONE', *, *, #39018, .T. ) ;
#34498 = CARTESIAN_POINT ( 'NONE',  ( 11.99999999999999822, 44.99326035066149387, -68.55367621811095091 ) ) ;
#34499 = VERTEX_POINT ( 'NONE', #18591 ) ;
#34500 = DIRECTION ( 'NONE',  ( 0.000000000000000000, 0.000000000000000000, 1.000000000000000000 ) ) ;
#34501 = ORIENTED_EDGE ( 'NONE', *, *, #18760, .F. ) ;
#34502 = DIRECTION ( 'NONE',  ( 0.000000000000000000, 0.000000000000000000, 1.000000000000000000 ) ) ;
#34503 = CARTESIAN_POINT ( 'NONE',  ( 11.99999999999999822, 76.41127070299273782, 12.93880638057342836 ) ) ;
#34504 = ORIENTED_EDGE ( 'NONE', *, *, #9891, .T. ) ;
#34505 = CARTESIAN_POINT ( 'NONE',  ( -6.170112525937322623, 10.87104923258428180, -54.99999999999998579 ) ) ;
#34506 = VERTEX_POINT ( 'NONE', #48439 ) ;
#34507 = AXIS2_PLACEMENT_3D ( 'NONE', #30513, #15107, #48385 ) ;
#34508 = CARTESIAN_POINT ( 'NONE',  ( 22.08297821871651578, -111.8242998470044540, -2.500000000000000000 ) ) ;
#34509 = CARTESIAN_POINT ( 'NONE',  ( 5.000000000000000000, 35.47612816024523852, 22.48208911017513145 ) ) ;
#34510 = EDGE_LOOP ( 'NONE', ( #37391, #12992, #39523, #17946 ) ) ;
#34511 = CIRCLE ( 'NONE', #36104, 16.00000000000000355 ) ;
#34512 = DIRECTION ( 'NONE',  ( 0.000000000000000000, 0.07845909572784530439, -0.9969173337331279638 ) ) ;
#34513 = ORIENTED_EDGE ( 'NONE', *, *, #40249, .F. ) ;
#34514 = ORIENTED_EDGE ( 'NONE', *, *, #46306, .T. ) ;
#34515 = EDGE_CURVE ( 'NONE', #31321, #27284, #22510, .T. ) ;
#34516 = CARTESIAN_POINT ( 'NONE',  ( 10.00000000000000000, 0.000000000000000000, 0.000000000000000000 ) ) ;
#34517 = CARTESIAN_POINT ( 'NONE',  ( 1.029419772574596825, -118.9089936151275140, -2.500000000000000000 ) ) ;
#34518 = AXIS2_PLACEMENT_3D ( 'NONE', #9837, #5689, #16944 ) ;
#34519 = LINE ( 'NONE', #38216, #23765 ) ;
#34520 = CARTESIAN_POINT ( 'NONE',  ( -3.000000000000000000, 24.81905959214261514, 9.408202855044825341 ) ) ;
#34521 = DIRECTION ( 'NONE',  ( -1.000000000000000000, -0.000000000000000000, -0.000000000000000000 ) ) ;
#34522 = ADVANCED_FACE ( 'NONE', ( #29369 ), #14687, .F. ) ;
#34523 = AXIS2_PLACEMENT_3D ( 'NONE', #23580, #35577, #20156 ) ;
#34524 = DIRECTION ( 'NONE',  ( -1.000000000000000000, 0.000000000000000000, 0.000000000000000000 ) ) ;
#34525 = VECTOR ( 'NONE', #29306, 1000.000000000000000 ) ;
#34526 = FACE_OUTER_BOUND ( 'NONE', #14644, .T. ) ;
#34527 = DIRECTION ( 'NONE',  ( -1.000000000000000000, -0.000000000000000000, 0.000000000000000000 ) ) ;
#34528 = ORIENTED_EDGE ( 'NONE', *, *, #38177, .F. ) ;
#34529 = DIRECTION ( 'NONE',  ( 0.000000000000000000, -0.8526401643540970632, 0.5224985647159409163 ) ) ;
#34530 = CARTESIAN_POINT ( 'NONE',  ( -3.000000000000000000, 8.688484142253939169, 21.88630264137371029 ) ) ;
#34531 = CARTESIAN_POINT ( 'NONE',  ( 0.000000000000000000, 73.72996012237440766, 14.67089635893739619 ) ) ;
#34532 = EDGE_CURVE ( 'NONE', #15854, #12049, #514, .T. ) ;
#34533 = ORIENTED_EDGE ( 'NONE', *, *, #18566, .T. ) ;
#34534 = AXIS2_PLACEMENT_3D ( 'NONE', #43022, #38380, #39104 ) ;
#34535 = EDGE_CURVE ( 'NONE', #27549, #38979, #34151, .T. ) ;
#34536 = DIRECTION ( 'NONE',  ( 1.000000000000000000, 0.000000000000000000, 0.000000000000000000 ) ) ;
#34537 = DIRECTION ( 'NONE',  ( -1.000000000000000000, -0.000000000000000000, -0.000000000000000000 ) ) ;
#34538 = DIRECTION ( 'NONE',  ( -1.000000000000000000, 0.000000000000000000, 0.000000000000000000 ) ) ;
#34539 = CARTESIAN_POINT ( 'NONE',  ( 10.00000000000000000, 0.000000000000000000, 0.000000000000000000 ) ) ;
#34540 = VERTEX_POINT ( 'NONE', #32781 ) ;
#34541 = CARTESIAN_POINT ( 'NONE',  ( 6.938893903907228378E-15, 1.932465207890948911E-15, 15.77977592589476608 ) ) ;
#34542 = ORIENTED_EDGE ( 'NONE', *, *, #25950, .T. ) ;
#34543 = LINE ( 'NONE', #5430, #32291 ) ;
#34544 = FACE_OUTER_BOUND ( 'NONE', #41869, .T. ) ;
#34545 = VERTEX_POINT ( 'NONE', #47956 ) ;
#34546 = VECTOR ( 'NONE', #17974, 1000.000000000000000 ) ;
#34547 = AXIS2_PLACEMENT_3D ( 'NONE', #27929, #1975, #13457 ) ;
#34548 = LINE ( 'NONE', #42398, #42590 ) ;
#34549 = VERTEX_POINT ( 'NONE', #216 ) ;
#34550 = VECTOR ( 'NONE', #31973, 1000.000000000000227 ) ;
#34551 = ADVANCED_FACE ( 'NONE', ( #44296 ), #29113, .T. ) ;
#34552 = CARTESIAN_POINT ( 'NONE',  ( 0.000000000000000000, -77.16300072079681627, 27.74655509720641078 ) ) ;
#34553 = DIRECTION ( 'NONE',  ( 0.000000000000000000, 0.000000000000000000, 1.000000000000000000 ) ) ;
#34555 = EDGE_LOOP ( 'NONE', ( #43223, #32107, #8565, #15678 ) ) ;
#34554 = CARTESIAN_POINT ( 'NONE',  ( 11.99999999999999822, -62.50329211542407393, -41.76937507738853839 ) ) ;
#34556 = AXIS2_PLACEMENT_3D ( 'NONE', #24149, #32223, #20463 ) ;
#34557 = EDGE_CURVE ( 'NONE', #9209, #35598, #10770, .T. ) ;
#34558 = ORIENTED_EDGE ( 'NONE', *, *, #19161, .F. ) ;
#34559 = ADVANCED_FACE ( 'NONE', ( #11256 ), #3403, .T. ) ;
#34560 = CIRCLE ( 'NONE', #5631, 16.00000000000000000 ) ;
#34561 = CARTESIAN_POINT ( 'NONE',  ( 11.99999999999999822, 0.000000000000000000, 0.000000000000000000 ) ) ;
#34562 = PLANE ( 'NONE',  #34837 ) ;
#34563 = PLANE ( 'NONE',  #8731 ) ;
#34564 = DIRECTION ( 'NONE',  ( -1.000000000000000000, -0.000000000000000000, -0.000000000000000000 ) ) ;
#34565 = ORIENTED_EDGE ( 'NONE', *, *, #46940, .F. ) ;
#34566 = FACE_OUTER_BOUND ( 'NONE', #23203, .T. ) ;
#34567 = ORIENTED_EDGE ( 'NONE', *, *, #20268, .T. ) ;
#34568 = ORIENTED_EDGE ( 'NONE', *, *, #2418, .F. ) ;
#34569 = DIRECTION ( 'NONE',  ( 1.000000000000000000, 0.000000000000000000, 0.000000000000000000 ) ) ;
#34570 = VERTEX_POINT ( 'NONE', #44533 ) ;
#34571 = LINE ( 'NONE', #27260, #16025 ) ;
#34572 = DIRECTION ( 'NONE',  ( -1.000000000000000000, 0.000000000000000000, 0.000000000000000000 ) ) ;
#34573 = CARTESIAN_POINT ( 'NONE',  ( 15.00000000000000000, 6.762365576493310826, -25.66652317338401090 ) ) ;
#34574 = ORIENTED_EDGE ( 'NONE', *, *, #2769, .F. ) ;
#34575 = CARTESIAN_POINT ( 'NONE',  ( 0.000000000000000000, 0.000000000000000000, 0.000000000000000000 ) ) ;
#34576 = EDGE_CURVE ( 'NONE', #37461, #3370, #33747, .T. ) ;
#34577 = DIRECTION ( 'NONE',  ( -1.000000000000000000, 0.000000000000000000, -0.000000000000000000 ) ) ;
#34578 = ADVANCED_FACE ( 'NONE', ( #37433 ), #27926, .F. ) ;
#34579 = EDGE_CURVE ( 'NONE', #36859, #40057, #9149, .T. ) ;
#34580 = CARTESIAN_POINT ( 'NONE',  ( 10.00000000000000000, 77.49459641780886443, 0.8261519478433866359 ) ) ;
#34581 = AXIS2_PLACEMENT_3D ( 'NONE', #23583, #5720, #20642 ) ;
#34582 = DIRECTION ( 'NONE',  ( 0.000000000000000000, 0.000000000000000000, 1.000000000000000000 ) ) ;
#34583 = DIRECTION ( 'NONE',  ( 0.000000000000000000, -0.7071067811865535679, 0.7071067811865413555 ) ) ;
#34584 = CIRCLE ( 'NONE', #47855, 82.00000000000000000 ) ;
#34585 = DIRECTION ( 'NONE',  ( -1.000000000000000000, -0.000000000000000000, 0.000000000000000000 ) ) ;
#34586 = LINE ( 'NONE', #5471, #15780 ) ;
#34587 = DIRECTION ( 'NONE',  ( -1.000000000000000000, 0.000000000000000000, 0.000000000000000000 ) ) ;
#34588 = VECTOR ( 'NONE', #16129, 1000.000000000000000 ) ;
#34589 = CIRCLE ( 'NONE', #18203, 82.00000000000000000 ) ;
#34590 = DIRECTION ( 'NONE',  ( -1.000000000000000000, 0.000000000000000000, 0.000000000000000000 ) ) ;
#34591 = DIRECTION ( 'NONE',  ( -0.8541291221503261033, 0.5200609990133016058, 0.000000000000000000 ) ) ;
#34592 = AXIS2_PLACEMENT_3D ( 'NONE', #4742, #32149, #43158 ) ;
#34593 = ORIENTED_EDGE ( 'NONE', *, *, #9331, .T. ) ;
#34594 = PRODUCT_RELATED_PRODUCT_CATEGORY ( 'part', '', ( #10492 ) ) ;
#34595 = DIRECTION ( 'NONE',  ( 0.000000000000000000, 0.000000000000000000, 1.000000000000000000 ) ) ;
#34596 = DIRECTION ( 'NONE',  ( 0.000000000000000000, -1.000000000000000000, -1.047444401652940007E-14 ) ) ;
#34597 = ORIENTED_EDGE ( 'NONE', *, *, #31300, .T. ) ;
#34598 = EDGE_LOOP ( 'NONE', ( #21871, #16251, #46312, #26940 ) ) ;
#34599 = CARTESIAN_POINT ( 'NONE',  ( 10.00000000000000000, -2.956366410620109519, -75.11725578898472122 ) ) ;
#34600 = ORIENTED_EDGE ( 'NONE', *, *, #43707, .F. ) ;
#34601 = ORIENTED_EDGE ( 'NONE', *, *, #42098, .T. ) ;
#34602 = ORIENTED_EDGE ( 'NONE', *, *, #14385, .T. ) ;
#34603 = ORIENTED_EDGE ( 'NONE', *, *, #9300, .F. ) ;
#34604 = AXIS2_PLACEMENT_3D ( 'NONE', #38238, #30649, #38969 ) ;
#34605 = ORIENTED_EDGE ( 'NONE', *, *, #505, .T. ) ;
#34606 = VERTEX_POINT ( 'NONE', #21542 ) ;
#34607 = AXIS2_PLACEMENT_3D ( 'NONE', #4913, #4676, #34278 ) ;
#34608 = ADVANCED_FACE ( 'NONE', ( #30344 ), #26429, .T. ) ;
#34609 = DIRECTION ( 'NONE',  ( 0.000000000000000000, -0.9781476007338065770, -0.2079116908177544853 ) ) ;
#34610 = CARTESIAN_POINT ( 'NONE',  ( 0.000000000000000000, 26.50000000000000000, -1.500000000000001332 ) ) ;
#34611 = AXIS2_PLACEMENT_3D ( 'NONE', #1373, #1857, #12392 ) ;
#34612 = CIRCLE ( 'NONE', #22157, 16.00000000000000355 ) ;
#34613 = DIRECTION ( 'NONE',  ( -1.000000000000000000, -0.000000000000000000, 0.000000000000000000 ) ) ;
#34614 = EDGE_CURVE ( 'NONE', #44761, #12437, #19302, .T. ) ;
#34615 = ORIENTED_EDGE ( 'NONE', *, *, #4049, .F. ) ;
#34616 = CARTESIAN_POINT ( 'NONE',  ( 11.99999999999999822, -44.88180994100419952, 63.18004540533013369 ) ) ;
#34617 = CIRCLE ( 'NONE', #40892, 82.00000000000000000 ) ;
#34618 = ORIENTED_EDGE ( 'NONE', *, *, #20497, .T. ) ;
#34619 = EDGE_CURVE ( 'NONE', #15250, #43433, #31073, .T. ) ;
#34620 = VECTOR ( 'NONE', #14684, 1000.000000000000000 ) ;
#34621 = LINE ( 'NONE', #1105, #6939 ) ;
#34622 = CARTESIAN_POINT ( 'NONE',  ( 10.00000000000000000, 25.88420570971400991, 27.13269053701105449 ) ) ;
#34623 = DIRECTION ( 'NONE',  ( -1.000000000000000000, 0.000000000000000000, -0.000000000000000000 ) ) ;
#34624 = ORIENTED_EDGE ( 'NONE', *, *, #36484, .F. ) ;
#34625 = VECTOR ( 'NONE', #31187, 1000.000000000000000 ) ;
#34626 = ORIENTED_EDGE ( 'NONE', *, *, #16531, .F. ) ;
#34627 = VERTEX_POINT ( 'NONE', #23231 ) ;
#34628 = DIRECTION ( 'NONE',  ( -0.02332147558787674158, -0.9997280174009349762, 0.000000000000000000 ) ) ;
#34629 = ORIENTED_EDGE ( 'NONE', *, *, #39415, .T. ) ;
#34630 = DIRECTION ( 'NONE',  ( -1.000000000000000000, 0.000000000000000000, 0.000000000000000000 ) ) ;
#34631 = AXIS2_PLACEMENT_3D ( 'NONE', #32106, #47026, #24039 ) ;
#34632 = DIRECTION ( 'NONE',  ( 0.000000000000000000, -0.4539904997395542430, 0.8910065241883641241 ) ) ;
#34633 = DIRECTION ( 'NONE',  ( 0.000000000000000000, 0.5877852522924741363, -0.8090169943749465631 ) ) ;
#34634 = LINE ( 'NONE', #38093, #13607 ) ;
#34635 = DIRECTION ( 'NONE',  ( -1.000000000000000000, 0.000000000000000000, 0.000000000000000000 ) ) ;
#34636 = DIRECTION ( 'NONE',  ( -1.000000000000000000, 0.000000000000000000, 0.000000000000000000 ) ) ;
#34637 = AXIS2_PLACEMENT_3D ( 'NONE', #29690, #6227, #44146 ) ;
#34638 = LINE ( 'NONE', #34392, #47872 ) ;
#34639 = EDGE_CURVE ( 'NONE', #9519, #6523, #2129, .T. ) ;
#34640 = EDGE_CURVE ( 'NONE', #38187, #45729, #38163, .T. ) ;
#34641 = CYLINDRICAL_SURFACE ( 'NONE', #44560, 31.99999999999999289 ) ;
#34642 = DIRECTION ( 'NONE',  ( 0.000000000000000000, 0.000000000000000000, 1.000000000000000000 ) ) ;
#34643 = CARTESIAN_POINT ( 'NONE',  ( 10.00000000000000000, 0.000000000000000000, 0.000000000000000000 ) ) ;
#34644 = CARTESIAN_POINT ( 'NONE',  ( 10.00000000000000000, 0.000000000000000000, 0.000000000000000000 ) ) ;
#34645 = EDGE_LOOP ( 'NONE', ( #39905, #42286, #10872, #47941 ) ) ;
#34646 = VERTEX_POINT ( 'NONE', #7811 ) ;
#34647 = DIRECTION ( 'NONE',  ( -1.000000000000000000, 0.000000000000000000, 0.000000000000000000 ) ) ;
#34648 = CARTESIAN_POINT ( 'NONE',  ( 12.00000000000000000, 14.60985201121703980, -18.46759930825707841 ) ) ;
#34649 = CARTESIAN_POINT ( 'NONE',  ( 15.00000000000000000, 5.835314593368470248, -22.81335362449854642 ) ) ;
#34650 = AXIS2_PLACEMENT_3D ( 'NONE', #41603, #3913, #22282 ) ;
#34651 = CARTESIAN_POINT ( 'NONE',  ( 0.000000000000000000, 71.27951684758026829, 30.41916302227139113 ) ) ;
#34652 = CARTESIAN_POINT ( 'NONE',  ( 114.1267819554180392, -82.91796067500511924, 5.500000000000000000 ) ) ;
#34654 = VECTOR ( 'NONE', #40101, 999.9999999999998863 ) ;
#34653 = CARTESIAN_POINT ( 'NONE',  ( 0.000000000000000000, -30.80686688396994910, -21.53537804866113703 ) ) ;
#34655 = EDGE_CURVE ( 'NONE', #14299, #32923, #20036, .T. ) ;
#34656 = ORIENTED_EDGE ( 'NONE', *, *, #27077, .T. ) ;
#34657 = DIRECTION ( 'NONE',  ( 0.000000000000000000, 0.000000000000000000, 1.000000000000000000 ) ) ;
#34658 = CARTESIAN_POINT ( 'NONE',  ( 11.99999999999999822, 35.91791733033476675, 68.67312586195008350 ) ) ;
#34659 = VERTEX_POINT ( 'NONE', #30571 ) ;
#34660 = VECTOR ( 'NONE', #44893, 1000.000000000000000 ) ;
#34661 = CIRCLE ( 'NONE', #35468, 31.99999999999998579 ) ;
#34662 = CIRCLE ( 'NONE', #24507, 32.00000000000000000 ) ;
#34663 =( NAMED_UNIT ( * ) PLANE_ANGLE_UNIT ( ) SI_UNIT ( $, .RADIAN. ) );
#34664 = DIRECTION ( 'NONE',  ( 0.000000000000000000, 0.000000000000000000, -1.000000000000000000 ) ) ;
#34665 = ORIENTED_EDGE ( 'NONE', *, *, #8655, .F. ) ;
#34666 = VECTOR ( 'NONE', #28537, 1000.000000000000000 ) ;
#34667 = AXIS2_PLACEMENT_3D ( 'NONE', #6192, #39732, #28708 ) ;
#34668 = ORIENTED_EDGE ( 'NONE', *, *, #10738, .T. ) ;
#34669 = AXIS2_PLACEMENT_3D ( 'NONE', #26198, #37451, #45045 ) ;
#34670 = PLANE ( 'NONE',  #5404 ) ;
#34671 = ORIENTED_EDGE ( 'NONE', *, *, #22816, .F. ) ;
#34672 = AXIS2_PLACEMENT_3D ( 'NONE', #17651, #9830, #10561 ) ;
#34673 = VERTEX_POINT ( 'NONE', #42080 ) ;
#34674 = CARTESIAN_POINT ( 'NONE',  ( 11.59999999999999787, 1.420590287010929336E-15, -43.79999999999998295 ) ) ;
#34675 = CARTESIAN_POINT ( 'NONE',  ( 11.99999999999999822, 0.000000000000000000, 0.000000000000000000 ) ) ;
#34676 = ADVANCED_FACE ( 'NONE', ( #45492 ), #1201, .T. ) ;
#34677 = VERTEX_POINT ( 'NONE', #42315 ) ;
#34678 = VERTEX_POINT ( 'NONE', #37924 ) ;
#34679 = ADVANCED_FACE ( 'NONE', ( #31079 ), #4405, .F. ) ;
#34680 = AXIS2_PLACEMENT_3D ( 'NONE', #20397, #16980, #42199 ) ;
#34681 = DIRECTION ( 'NONE',  ( 0.000000000000000000, -0.9945218953682730678, 0.1045284632676570929 ) ) ;
#34683 = ORIENTED_EDGE ( 'NONE', *, *, #6367, .T. ) ;
#34682 = DIRECTION ( 'NONE',  ( 0.000000000000000000, 1.000000000000000000, 0.000000000000000000 ) ) ;
#34685 = CYLINDRICAL_SURFACE ( 'NONE', #32166, 31.99999999999998579 ) ;
#34684 = AXIS2_PLACEMENT_3D ( 'NONE', #26236, #12281, #41178 ) ;
#34686 = ORIENTED_EDGE ( 'NONE', *, *, #720, .F. ) ;
#34687 = DIRECTION ( 'NONE',  ( 0.000000000000000000, -0.4067366430758009299, -0.9135454576426005335 ) ) ;
#34688 = EDGE_CURVE ( 'NONE', #29506, #36854, #6049, .T. ) ;
#34689 = EDGE_LOOP ( 'NONE', ( #27022, #43382, #18578, #9592 ) ) ;
#34690 = ORIENTED_EDGE ( 'NONE', *, *, #46853, .T. ) ;
#34691 = DIRECTION ( 'NONE',  ( -1.000000000000000000, 0.000000000000000000, 0.000000000000000000 ) ) ;
#34692 = VECTOR ( 'NONE', #23337, 1000.000000000000000 ) ;
#34693 = CIRCLE ( 'NONE', #32341, 31.99999999999999289 ) ;
#34694 = DIRECTION ( 'NONE',  ( 0.000000000000000000, 0.000000000000000000, 1.000000000000000000 ) ) ;
#34695 = VECTOR ( 'NONE', #34127, 1000.000000000000000 ) ;
#34696 = ORIENTED_EDGE ( 'NONE', *, *, #2932, .T. ) ;
#34697 = DIRECTION ( 'NONE',  ( 0.000000000000000000, 0.000000000000000000, 1.000000000000000000 ) ) ;
#34698 = CARTESIAN_POINT ( 'NONE',  ( 10.00000000000000000, 0.000000000000000000, 0.000000000000000000 ) ) ;
#34699 = CARTESIAN_POINT ( 'NONE',  ( 10.00000000000000000, -70.53064760720336324, 26.01480285779810231 ) ) ;
#34700 = VERTEX_POINT ( 'NONE', #34468 ) ;
#34701 = ORIENTED_EDGE ( 'NONE', *, *, #3588, .F. ) ;
#34702 = EDGE_CURVE ( 'NONE', #6878, #21795, #23708, .T. ) ;
#34703 = DIRECTION ( 'NONE',  ( 0.000000000000000000, 0.000000000000000000, 1.000000000000000000 ) ) ;
#34704 = DIRECTION ( 'NONE',  ( 0.000000000000000000, 0.3090169943749482839, -0.9510565162951533091 ) ) ;
#34705 = CIRCLE ( 'NONE', #19085, 82.00000000000000000 ) ;
#34706 = CIRCLE ( 'NONE', #30818, 16.00000000000000000 ) ;
#34707 = EDGE_LOOP ( 'NONE', ( #5403, #34542, #32984, #45187 ) ) ;
#34708 = EDGE_CURVE ( 'NONE', #36840, #15559, #31842, .T. ) ;
#34709 = CYLINDRICAL_SURFACE ( 'NONE', #18151, 12.49999999999999645 ) ;
#34710 = ORIENTED_EDGE ( 'NONE', *, *, #47124, .T. ) ;
#34711 = VECTOR ( 'NONE', #24931, 1000.000000000000000 ) ;
#34712 = CARTESIAN_POINT ( 'NONE',  ( -10.00000000000000000, 0.000000000000000000, 0.000000000000000000 ) ) ;
#34713 = DIRECTION ( 'NONE',  ( -1.000000000000000000, -0.000000000000000000, -0.000000000000000000 ) ) ;
#34714 = LINE ( 'NONE', #30826, #11278 ) ;
#34715 = CARTESIAN_POINT ( 'NONE',  ( 11.99999999999999822, 46.53671651293948486, 59.03961581697416250 ) ) ;
#34716 = VECTOR ( 'NONE', #26596, 1000.000000000000000 ) ;
#34717 = DIRECTION ( 'NONE',  ( 0.000000000000000000, -0.5877852522924625900, -0.8090169943749551118 ) ) ;
#34718 = DIRECTION ( 'NONE',  ( -1.000000000000000000, 0.000000000000000000, 0.000000000000000000 ) ) ;
#34719 = EDGE_CURVE ( 'NONE', #41352, #43656, #15888, .T. ) ;
#34720 = DIRECTION ( 'NONE',  ( -0.000000000000000000, 0.8090169943749504489, -0.5877852522924689183 ) ) ;
#34721 = CARTESIAN_POINT ( 'NONE',  ( 0.000000000000000000, -30.41916302227060598, -71.27951684758059514 ) ) ;
#34722 = ORIENTED_EDGE ( 'NONE', *, *, #10160, .T. ) ;
#34723 = CARTESIAN_POINT ( 'NONE',  ( -0.2999999999999947153, 0.000000000000000000, -12.50000000000000000 ) ) ;
#34724 = VERTEX_POINT ( 'NONE', #16372 ) ;
#34725 = ORIENTED_EDGE ( 'NONE', *, *, #6934, .F. ) ;
#34726 = EDGE_CURVE ( 'NONE', #14894, #32964, #29476, .T. ) ;
#34727 = CYLINDRICAL_SURFACE ( 'NONE', #5849, 31.99999999999998579 ) ;
#34728 = CIRCLE ( 'NONE', #32409, 82.00000000000000000 ) ;
#34729 = ORIENTED_EDGE ( 'NONE', *, *, #3350, .T. ) ;
#34730 = CIRCLE ( 'NONE', #15228, 31.99999999999999645 ) ;
#34731 = CIRCLE ( 'NONE', #39321, 82.00000000000000000 ) ;
#34732 = CARTESIAN_POINT ( 'NONE',  ( 0.000000000000000000, -0.8299999999999999600, 0.000000000000000000 ) ) ;
#34733 = DIRECTION ( 'NONE',  ( -1.000000000000000000, 0.000000000000000000, -0.000000000000000000 ) ) ;
#34734 = EDGE_LOOP ( 'NONE', ( #15845, #15656, #43793, #3509 ) ) ;
#34735 = VERTEX_POINT ( 'NONE', #4870 ) ;
#34736 = VECTOR ( 'NONE', #6522, 1000.000000000000114 ) ;
#34737 = CONICAL_SURFACE ( 'NONE', #23815, 15.39727592608509177, 1.361356816555577609 ) ;
#34738 = AXIS2_PLACEMENT_3D ( 'NONE', #40562, #44714, #11189 ) ;
#34739 = EDGE_CURVE ( 'NONE', #39062, #25700, #9946, .T. ) ;
#34740 = CARTESIAN_POINT ( 'NONE',  ( 10.00000000000000000, -10.30890764327441822, 81.34940948281332851 ) ) ;
#34741 = VERTEX_POINT ( 'NONE', #15415 ) ;
#34742 = EDGE_CURVE ( 'NONE', #28319, #12709, #34923, .T. ) ;
#34743 = ORIENTED_EDGE ( 'NONE', *, *, #21551, .T. ) ;
#34744 = ORIENTED_EDGE ( 'NONE', *, *, #34271, .T. ) ;
#34745 = ORIENTED_EDGE ( 'NONE', *, *, #13504, .T. ) ;
#34746 = ORIENTED_EDGE ( 'NONE', *, *, #43121, .T. ) ;
#34747 = VECTOR ( 'NONE', #11432, 1000.000000000000000 ) ;
#34748 = ADVANCED_FACE ( 'NONE', ( #8303 ), #4625, .T. ) ;
#34749 = DIRECTION ( 'NONE',  ( -1.000000000000000000, 0.000000000000000000, -0.000000000000000000 ) ) ;
#34750 = ORIENTED_EDGE ( 'NONE', *, *, #18933, .T. ) ;
#34751 = ORIENTED_EDGE ( 'NONE', *, *, #18111, .F. ) ;
#34752 = CARTESIAN_POINT ( 'NONE',  ( -10.00000000000000000, 0.000000000000000000, 0.000000000000000000 ) ) ;
#34753 = ADVANCED_FACE ( 'NONE', ( #17314 ), #16861, .T. ) ;
#34754 = VERTEX_POINT ( 'NONE', #24192 ) ;
#34755 = DIRECTION ( 'NONE',  ( 0.000000000000000000, 0.9876883405951371042, 0.1564344650402347547 ) ) ;
#34756 = DIRECTION ( 'NONE',  ( 0.000000000000000000, 0.000000000000000000, 1.000000000000000000 ) ) ;
#34757 = CARTESIAN_POINT ( 'NONE',  ( 10.00000000000000000, -51.29473840253269401, 63.97538442413405591 ) ) ;
#34758 = ORIENTED_EDGE ( 'NONE', *, *, #16807, .T. ) ;
#34759 = DIRECTION ( 'NONE',  ( 0.000000000000000000, 0.000000000000000000, 1.000000000000000000 ) ) ;
#34760 = ORIENTED_EDGE ( 'NONE', *, *, #41955, .F. ) ;
#34761 = DIRECTION ( 'NONE',  ( -0.000000000000000000, 0.000000000000000000, -1.000000000000000000 ) ) ;
#34762 = AXIS2_PLACEMENT_3D ( 'NONE', #45256, #37666, #22262 ) ;
#34763 = DIRECTION ( 'NONE',  ( -1.000000000000000000, -0.000000000000000000, -0.000000000000000000 ) ) ;
#34764 = ORIENTED_EDGE ( 'NONE', *, *, #6268, .T. ) ;
#34765 = DIRECTION ( 'NONE',  ( -1.000000000000000000, -0.000000000000000000, -0.000000000000000000 ) ) ;
#34766 = ORIENTED_EDGE ( 'NONE', *, *, #43755, .T. ) ;
#34767 = VERTEX_POINT ( 'NONE', #23965 ) ;
#34768 = DIRECTION ( 'NONE',  ( 0.3853207896976523772, -0.9227826878668550226, 0.000000000000000000 ) ) ;
#34769 = CIRCLE ( 'NONE', #18379, 15.99999999999999822 ) ;
#34770 = CARTESIAN_POINT ( 'NONE',  ( 0.000000000000000000, 0.000000000000000000, 0.000000000000000000 ) ) ;
#34771 = ORIENTED_EDGE ( 'NONE', *, *, #25776, .F. ) ;
#34772 = LINE ( 'NONE', #38452, #13633 ) ;
#34773 = DIRECTION ( 'NONE',  ( -1.000000000000000000, -0.000000000000000000, -0.000000000000000000 ) ) ;
#34774 = CYLINDRICAL_SURFACE ( 'NONE', #40948, 31.99999999999998579 ) ;
#34775 = CARTESIAN_POINT ( 'NONE',  ( -4.250000000000000000, -13.95926121303099343, -1.199999999999999956 ) ) ;
#34776 = LINE ( 'NONE', #42625, #43849 ) ;
#34777 = DIRECTION ( 'NONE',  ( -1.000000000000000000, 0.000000000000000000, 0.000000000000000000 ) ) ;
#34778 = EDGE_CURVE ( 'NONE', #24346, #46450, #40421, .T. ) ;
#34779 = VECTOR ( 'NONE', #39268, 1000.000000000000000 ) ;
#34780 = VECTOR ( 'NONE', #42991, 1000.000000000000000 ) ;
#34781 = FACE_OUTER_BOUND ( 'NONE', #45338, .T. ) ;
#34782 = LINE ( 'NONE', #5657, #3689 ) ;
#34783 = CARTESIAN_POINT ( 'NONE',  ( 0.000000000000000000, 12.93880638057313703, 76.41127070299276625 ) ) ;
#34784 = VECTOR ( 'NONE', #16793, 1000.000000000000000 ) ;
#34785 = DIRECTION ( 'NONE',  ( -1.000000000000000000, -0.000000000000000000, 0.000000000000000000 ) ) ;
#34786 = DIRECTION ( 'NONE',  ( 1.000000000000000000, -0.000000000000000000, -0.000000000000000000 ) ) ;
#34787 = CARTESIAN_POINT ( 'NONE',  ( 0.000000000000000000, -75.11764819372149304, 2.946379043146075905 ) ) ;
#34788 = LINE ( 'NONE', #12528, #8488 ) ;
#34789 = CIRCLE ( 'NONE', #13693, 16.00000000000000000 ) ;
#34790 = ORIENTED_EDGE ( 'NONE', *, *, #22714, .F. ) ;
#34791 = ORIENTED_EDGE ( 'NONE', *, *, #21977, .F. ) ;
#34792 = DIRECTION ( 'NONE',  ( 0.000000000000000000, 0.8910065241883691201, -0.4539904997395446951 ) ) ;
#34793 = ORIENTED_EDGE ( 'NONE', *, *, #36424, .F. ) ;
#34794 = DIRECTION ( 'NONE',  ( 1.000000000000000000, -0.000000000000000000, -0.000000000000000000 ) ) ;
#34795 = APPLICATION_PROTOCOL_DEFINITION ( 'draft international standard', 'automotive_design', 1998, #40098 ) ;
#34796 = AXIS2_PLACEMENT_3D ( 'NONE', #27635, #4873, #24199 ) ;
#34797 = DIRECTION ( 'NONE',  ( 0.000000000000000000, 0.000000000000000000, 1.000000000000000000 ) ) ;
#34798 = VERTEX_POINT ( 'NONE', #43285 ) ;
#34799 = AXIS2_PLACEMENT_3D ( 'NONE', #46345, #27763, #42688 ) ;
#34800 = EDGE_CURVE ( 'NONE', #35770, #1468, #41204, .T. ) ;
#34801 = CIRCLE ( 'NONE', #30798, 31.99999999999998579 ) ;
#34802 = CARTESIAN_POINT ( 'NONE',  ( 5.000000000000000000, -21.60688246758642705, 79.10210256391360417 ) ) ;
#34803 = ORIENTED_EDGE ( 'NONE', *, *, #9174, .F. ) ;
#34805 = EDGE_CURVE ( 'NONE', #26939, #17075, #37273, .T. ) ;
#34804 = FACE_OUTER_BOUND ( 'NONE', #47473, .T. ) ;
#34806 = ORIENTED_EDGE ( 'NONE', *, *, #48287, .T. ) ;
#34807 = CIRCLE ( 'NONE', #41088, 31.99999999999999645 ) ;
#34808 = VECTOR ( 'NONE', #40254, 1000.000000000000000 ) ;
#34809 = CARTESIAN_POINT ( 'NONE',  ( 10.00000000000000000, 0.000000000000000000, 0.000000000000000000 ) ) ;
#34810 = EDGE_CURVE ( 'NONE', #10117, #39461, #14641, .T. ) ;
#34811 = CARTESIAN_POINT ( 'NONE',  ( -3.000000000000000000, 16.83928648764923253, 16.46020748918050458 ) ) ;
#34812 = ORIENTED_EDGE ( 'NONE', *, *, #2078, .F. ) ;
#34814 = ORIENTED_EDGE ( 'NONE', *, *, #2445, .T. ) ;
#34813 = CARTESIAN_POINT ( 'NONE',  ( 12.50000000000000000, -107.5000000000000000, 2.500000000000000000 ) ) ;
#34815 = ORIENTED_EDGE ( 'NONE', *, *, #47765, .T. ) ;
#34816 = VECTOR ( 'NONE', #33869, 1000.000000000000000 ) ;
#34817 = EDGE_CURVE ( 'NONE', #40828, #29191, #30254, .T. ) ;
#34818 = DIRECTION ( 'NONE',  ( -1.000000000000000000, 0.000000000000000000, 0.000000000000000000 ) ) ;
#34819 = CIRCLE ( 'NONE', #9809, 31.99999999999998579 ) ;
#34820 = AXIS2_PLACEMENT_3D ( 'NONE', #41882, #19566, #34502 ) ;
#34821 = FACE_OUTER_BOUND ( 'NONE', #41378, .T. ) ;
#34822 = CARTESIAN_POINT ( 'NONE',  ( 11.99999999999999822, 74.65491531819118620, -8.830959090342659579 ) ) ;
#34823 = CARTESIAN_POINT ( 'NONE',  ( 11.99999999999999822, 66.50666863322000211, 39.78640506895628448 ) ) ;
#34824 = DIRECTION ( 'NONE',  ( 0.000000000000000000, 0.000000000000000000, 1.000000000000000000 ) ) ;
#34825 = ORIENTED_EDGE ( 'NONE', *, *, #21770, .T. ) ;
#34826 = CARTESIAN_POINT ( 'NONE',  ( 10.00000000000000000, 14.67089635893819377, -73.72996012237423713 ) ) ;
#34827 = ORIENTED_EDGE ( 'NONE', *, *, #37424, .F. ) ;
#34828 = ORIENTED_EDGE ( 'NONE', *, *, #8602, .F. ) ;
#34829 = CARTESIAN_POINT ( 'NONE',  ( 0.000000000000000000, -14.54903810567645195, -22.19967320028775504 ) ) ;
#34830 = EDGE_LOOP ( 'NONE', ( #24414, #25138, #43613, #19377 ) ) ;
#34831 = DIRECTION ( 'NONE',  ( 0.000000000000000000, -0.8090169943749403458, -0.5877852522924830181 ) ) ;
#34832 = AXIS2_PLACEMENT_3D ( 'NONE', #12614, #27306, #31722 ) ;
#34833 = LINE ( 'NONE', #43152, #33654 ) ;
#34834 = CARTESIAN_POINT ( 'NONE',  ( -19.90058851926621131, -132.5883508287165853, 5.500000000000000000 ) ) ;
#34835 = EDGE_LOOP ( 'NONE', ( #3115, #47544, #27338, #29651 ) ) ;
#34836 = CARTESIAN_POINT ( 'NONE',  ( 0.000000000000000000, 0.000000000000000000, 0.000000000000000000 ) ) ;
#34837 = AXIS2_PLACEMENT_3D ( 'NONE', #38990, #39224, #5692 ) ;
#34838 = DIRECTION ( 'NONE',  ( -1.000000000000000000, 0.000000000000000000, 0.000000000000000000 ) ) ;
#34839 = EDGE_CURVE ( 'NONE', #9856, #17154, #43534, .T. ) ;
#34840 = FACE_OUTER_BOUND ( 'NONE', #3016, .T. ) ;
#34841 = FACE_OUTER_BOUND ( 'NONE', #26097, .T. ) ;
#34842 = AXIS2_PLACEMENT_3D ( 'NONE', #2447, #12522, #32323 ) ;
#34843 = CARTESIAN_POINT ( 'NONE',  ( 10.00000000000000000, 21.32104025579158701, -30.84782396557194772 ) ) ;
#34844 = LINE ( 'NONE', #45146, #34025 ) ;
#34845 = CARTESIAN_POINT ( 'NONE',  ( 11.99999999999999822, 0.000000000000000000, 0.000000000000000000 ) ) ;
#34846 = PLANE ( 'NONE',  #33820 ) ;
#34847 = DIRECTION ( 'NONE',  ( -1.000000000000000000, 0.000000000000000000, -0.000000000000000000 ) ) ;
#34848 = VERTEX_POINT ( 'NONE', #16606 ) ;
#34849 = CIRCLE ( 'NONE', #41123, 37.49900000000000944 ) ;
#34850 = CARTESIAN_POINT ( 'NONE',  ( 0.000000000000000000, -16.65560815589383381, -38.55633173627028754 ) ) ;
#34851 = ORIENTED_EDGE ( 'NONE', *, *, #20846, .T. ) ;
#34852 = ORIENTED_EDGE ( 'NONE', *, *, #34926, .T. ) ;
#34853 = CARTESIAN_POINT ( 'NONE',  ( -18.12185313557660038, -104.9634299478706794, -5.500000000000000000 ) ) ;
#34854 = EDGE_CURVE ( 'NONE', #15510, #18371, #35208, .T. ) ;
#34855 = CIRCLE ( 'NONE', #47381, 30.50000000000000000 ) ;
#34856 = EDGE_CURVE ( 'NONE', #46126, #42000, #39626, .T. ) ;
#34857 = CARTESIAN_POINT ( 'NONE',  ( 0.000000000000000000, 5.835314593368477354, 22.81335362449854642 ) ) ;
#34858 = VECTOR ( 'NONE', #38266, 1000.000000000000000 ) ;
#34859 = ORIENTED_EDGE ( 'NONE', *, *, #41027, .T. ) ;
#34860 = AXIS2_PLACEMENT_3D ( 'NONE', #37077, #18709, #3549 ) ;
#34861 = ORIENTED_EDGE ( 'NONE', *, *, #24813, .T. ) ;
#34862 = CIRCLE ( 'NONE', #23944, 77.49900000000000944 ) ;
#34863 = ORIENTED_EDGE ( 'NONE', *, *, #48180, .T. ) ;
#34864 = EDGE_CURVE ( 'NONE', #35557, #9076, #42767, .T. ) ;
#34865 = AXIS2_PLACEMENT_3D ( 'NONE', #2967, #9586, #39720 ) ;
#34866 = ORIENTED_EDGE ( 'NONE', *, *, #35532, .T. ) ;
#34867 = EDGE_CURVE ( 'NONE', #33766, #1684, #32580, .T. ) ;
#34868 = EDGE_CURVE ( 'NONE', #1357, #31567, #32511, .T. ) ;
#34869 = AXIS2_PLACEMENT_3D ( 'NONE', #35265, #27452, #16668 ) ;
#34870 = CARTESIAN_POINT ( 'NONE',  ( 10.00000000000000000, 35.92658777277511462, 10.74501242461295014 ) ) ;
#34871 = CARTESIAN_POINT ( 'NONE',  ( -30.50000000000000000, -120.0000000000000000, -5.500000000000000000 ) ) ;
#34872 = DIRECTION ( 'NONE',  ( 0.000000000000000000, -1.000000000000000000, -1.040834085586084257E-14 ) ) ;
#34873 = ORIENTED_EDGE ( 'NONE', *, *, #14421, .F. ) ;
#34874 = DIRECTION ( 'NONE',  ( 0.000000000000000000, 0.8090169943749446757, 0.5877852522924769119 ) ) ;
#34875 = EDGE_CURVE ( 'NONE', #33538, #33012, #32265, .T. ) ;
#34876 = VERTEX_POINT ( 'NONE', #1938 ) ;
#34877 = ORIENTED_EDGE ( 'NONE', *, *, #6339, .F. ) ;
#34878 = LINE ( 'NONE', #16522, #45233 ) ;
#34879 = DIRECTION ( 'NONE',  ( -1.000000000000000000, 0.000000000000000000, 0.000000000000000000 ) ) ;
#34880 = DIRECTION ( 'NONE',  ( 1.000000000000000000, 0.000000000000000000, 0.000000000000000000 ) ) ;
#34881 = VECTOR ( 'NONE', #1421, 1000.000000000000000 ) ;
#34882 = ORIENTED_EDGE ( 'NONE', *, *, #31954, .F. ) ;
#34883 = ORIENTED_EDGE ( 'NONE', *, *, #40954, .F. ) ;
#34884 = DIRECTION ( 'NONE',  ( 1.000000000000000000, -0.000000000000000000, -0.000000000000000000 ) ) ;
#34885 = EDGE_LOOP ( 'NONE', ( #34513, #48211, #42198, #12272 ) ) ;
#34886 = LINE ( 'NONE', #27806, #13734 ) ;
#34887 = AXIS2_PLACEMENT_3D ( 'NONE', #33511, #48207, #11008 ) ;
#34888 = FACE_OUTER_BOUND ( 'NONE', #6895, .T. ) ;
#34889 = DIRECTION ( 'NONE',  ( -1.000000000000000000, 0.000000000000000000, 0.000000000000000000 ) ) ;
#34890 = DIRECTION ( 'NONE',  ( 0.000000000000000000, 0.000000000000000000, 1.000000000000000000 ) ) ;
#34891 = DIRECTION ( 'NONE',  ( 0.000000000000000000, 0.000000000000000000, -1.000000000000000000 ) ) ;
#34892 = DIRECTION ( 'NONE',  ( -1.000000000000000000, -0.000000000000000000, -0.000000000000000000 ) ) ;
#34893 = LINE ( 'NONE', #5042, #22096 ) ;
#34894 = EDGE_LOOP ( 'NONE', ( #18951, #29504, #15222, #34273 ) ) ;
#34895 = LINE ( 'NONE', #39057, #10152 ) ;
#34896 = CARTESIAN_POINT ( 'NONE',  ( 0.000000000000000000, 0.000000000000000000, 0.000000000000000000 ) ) ;
#34897 = FACE_OUTER_BOUND ( 'NONE', #3368, .T. ) ;
#34898 = DIRECTION ( 'NONE',  ( 0.000000000000000000, 0.000000000000000000, 1.000000000000000000 ) ) ;
#34899 = EDGE_LOOP ( 'NONE', ( #15087, #14232, #6746, #24874 ) ) ;
#34900 = VERTEX_POINT ( 'NONE', #47189 ) ;
#34901 = AXIS2_PLACEMENT_3D ( 'NONE', #7208, #1934, #3283 ) ;
#34902 = DIRECTION ( 'NONE',  ( 1.000000000000000000, 0.000000000000000000, 0.000000000000000000 ) ) ;
#34903 = CARTESIAN_POINT ( 'NONE',  ( 11.99999999999999822, -55.20638768913797634, 51.02545421589302777 ) ) ;
#34904 = DIRECTION ( 'NONE',  ( -1.000000000000000000, -0.000000000000000000, -0.000000000000000000 ) ) ;
#34905 = CARTESIAN_POINT ( 'NONE',  ( 11.99999999999999822, 0.000000000000000000, 0.000000000000000000 ) ) ;
#34906 = CIRCLE ( 'NONE', #35684, 16.00000000000000000 ) ;
#34907 = EDGE_CURVE ( 'NONE', #34932, #14857, #17731, .T. ) ;
#34908 = LINE ( 'NONE', #24853, #47444 ) ;
#34909 = DIRECTION ( 'NONE',  ( -1.000000000000000000, -0.000000000000000000, -0.000000000000000000 ) ) ;
#34910 = VECTOR ( 'NONE', #16803, 1000.000000000000000 ) ;
#34911 = EDGE_CURVE ( 'NONE', #32361, #14333, #13670, .T. ) ;
#34912 = DIRECTION ( 'NONE',  ( -0.2867529058022035837, 0.9580045777625452175, 0.000000000000000000 ) ) ;
#34913 = LINE ( 'NONE', #38345, #26385 ) ;
#34914 = ORIENTED_EDGE ( 'NONE', *, *, #46531, .T. ) ;
#34915 = ADVANCED_FACE ( 'NONE', ( #46955 ), #12701, .T. ) ;
#34916 = ORIENTED_EDGE ( 'NONE', *, *, #9850, .T. ) ;
#34917 = SURFACE_STYLE_FILL_AREA ( #5795 ) ;
#34918 = EDGE_CURVE ( 'NONE', #16794, #18736, #2910, .T. ) ;
#34919 = CARTESIAN_POINT ( 'NONE',  ( 10.00000000000000000, 75.54627589209970040, -17.28742895386005785 ) ) ;
#34920 = ORIENTED_EDGE ( 'NONE', *, *, #10743, .T. ) ;
#34921 = ORIENTED_EDGE ( 'NONE', *, *, #8252, .T. ) ;
#34922 = EDGE_CURVE ( 'NONE', #28193, #38831, #16247, .T. ) ;
#34923 = CIRCLE ( 'NONE', #13838, 16.00000000000000000 ) ;
#34924 = CARTESIAN_POINT ( 'NONE',  ( 11.99999999999999822, 54.21277698773752007, -55.38113227695726692 ) ) ;
#34925 = ORIENTED_EDGE ( 'NONE', *, *, #768, .T. ) ;
#34926 = EDGE_CURVE ( 'NONE', #4822, #45107, #10950, .T. ) ;
#34927 = EDGE_CURVE ( 'NONE', #22527, #4758, #44719, .T. ) ;
#34928 = ORIENTED_EDGE ( 'NONE', *, *, #4588, .T. ) ;
#34929 = CIRCLE ( 'NONE', #2134, 82.00000000000000000 ) ;
#34930 = CARTESIAN_POINT ( 'NONE',  ( 5.000000000000002665, 71.87247863392471459, -39.47590169984770370 ) ) ;
#34931 = CYLINDRICAL_SURFACE ( 'NONE', #5013, 12.50000000000000000 ) ;
#34932 = VERTEX_POINT ( 'NONE', #44481 ) ;
#34933 = EDGE_LOOP ( 'NONE', ( #13168, #23471, #24096, #28705 ) ) ;
#34934 = DIRECTION ( 'NONE',  ( -1.000000000000000000, 0.000000000000000000, 0.000000000000000000 ) ) ;
#34935 = ADVANCED_FACE ( 'NONE', ( #29318 ), #25868, .F. ) ;
#34937 = ORIENTED_EDGE ( 'NONE', *, *, #34619, .F. ) ;
#34936 = CARTESIAN_POINT ( 'NONE',  ( 10.00000000000000000, 2.663952781846149254, 41.91543099594818500 ) ) ;
#34938 = AXIS2_PLACEMENT_3D ( 'NONE', #2571, #17978, #29255 ) ;
#34939 = FACE_OUTER_BOUND ( 'NONE', #3064, .T. ) ;
#34940 = ORIENTED_EDGE ( 'NONE', *, *, #19909, .T. ) ;
#34941 = CARTESIAN_POINT ( 'NONE',  ( 10.00000000000000000, 37.16516213103277977, 4.992566952385115719 ) ) ;
#34942 = ORIENTED_EDGE ( 'NONE', *, *, #7150, .F. ) ;
#34943 = VERTEX_POINT ( 'NONE', #21957 ) ;
#34944 = CARTESIAN_POINT ( 'NONE',  ( 12.00000000000000000, -26.23277895567251861, -4.042438405569750870 ) ) ;
#34945 = DIRECTION ( 'NONE',  ( 0.000000000000000000, 0.000000000000000000, 1.000000000000000000 ) ) ;
#34946 = EDGE_LOOP ( 'NONE', ( #3167, #9462, #34993, #8076 ) ) ;
#34947 = CARTESIAN_POINT ( 'NONE',  ( 10.00000000000000000, 0.000000000000000000, 0.000000000000000000 ) ) ;
#34948 = DIRECTION ( 'NONE',  ( -1.000000000000000000, 0.000000000000000000, -0.000000000000000000 ) ) ;
#34949 = CARTESIAN_POINT ( 'NONE',  ( 10.00000000000000000, 21.60688246758695641, -79.10210256391344785 ) ) ;
#34950 = ORIENTED_EDGE ( 'NONE', *, *, #12065, .F. ) ;
#34951 = ORIENTED_EDGE ( 'NONE', *, *, #19029, .T. ) ;
#34952 = FACE_OUTER_BOUND ( 'NONE', #30699, .T. ) ;
#34953 = CYLINDRICAL_SURFACE ( 'NONE', #19629, 31.99999999999999289 ) ;
#34954 = CIRCLE ( 'NONE', #31877, 16.00000000000000000 ) ;
#34955 = ORIENTED_EDGE ( 'NONE', *, *, #44470, .F. ) ;
#34956 = DIRECTION ( 'NONE',  ( 0.000000000000000000, 1.000000000000000000, 3.469446951953614189E-15 ) ) ;
#34957 = VERTEX_POINT ( 'NONE', #33464 ) ;
#34958 = CARTESIAN_POINT ( 'NONE',  ( -12.50000000000000000, -132.5000000000000000, -2.500000000000000000 ) ) ;
#34959 = AXIS2_PLACEMENT_3D ( 'NONE', #27334, #30517, #19256 ) ;
#34960 = CARTESIAN_POINT ( 'NONE',  ( 10.00000000000000000, -17.80606268964563554, 33.00180498840040855 ) ) ;
#34961 = CARTESIAN_POINT ( 'NONE',  ( -10.00000000000000000, 0.000000000000000000, 0.000000000000000000 ) ) ;
#34962 = ORIENTED_EDGE ( 'NONE', *, *, #20944, .T. ) ;
#34963 = CARTESIAN_POINT ( 'NONE',  ( 0.000000000000000000, 46.11716303203283474, -67.80270845531839541 ) ) ;
#34964 = DIRECTION ( 'NONE',  ( -1.000000000000000000, -0.000000000000000000, 0.000000000000000000 ) ) ;
#34965 = CARTESIAN_POINT ( 'NONE',  ( 5.000000000000000000, 55.16347631943131802, -60.67117009219075641 ) ) ;
#34966 = EDGE_CURVE ( 'NONE', #7292, #36854, #16995, .T. ) ;
#34967 = CIRCLE ( 'NONE', #13872, 31.99999999999998934 ) ;
#34968 = DIRECTION ( 'NONE',  ( -1.000000000000000000, -0.000000000000000000, -0.000000000000000000 ) ) ;
#34969 = PLANE ( 'NONE',  #10602 ) ;
#34970 = ORIENTED_EDGE ( 'NONE', *, *, #43381, .T. ) ;
#34971 = EDGE_CURVE ( 'NONE', #48222, #31890, #40461, .T. ) ;
#34972 = CARTESIAN_POINT ( 'NONE',  ( -3.000000000000000888, 20.64000000000000057, 0.000000000000000000 ) ) ;
#34973 = EDGE_CURVE ( 'NONE', #21372, #46304, #33227, .T. ) ;
#34974 = ORIENTED_EDGE ( 'NONE', *, *, #22080, .F. ) ;
#34975 = CIRCLE ( 'NONE', #12353, 31.99999999999998579 ) ;
#34976 = CYLINDRICAL_SURFACE ( 'NONE', #29273, 1.000000000000000000 ) ;
#34977 = VERTEX_POINT ( 'NONE', #32973 ) ;
#34978 = VERTEX_POINT ( 'NONE', #3105 ) ;
#34979 = DIRECTION ( 'NONE',  ( 0.000000000000000000, 0.000000000000000000, 1.000000000000000000 ) ) ;
#34980 = DIRECTION ( 'NONE',  ( 0.000000000000000000, -0.4539904997395351471, -0.8910065241883737830 ) ) ;
#34981 = ORIENTED_EDGE ( 'NONE', *, *, #18913, .T. ) ;
#34982 = EDGE_CURVE ( 'NONE', #26337, #35099, #21680, .T. ) ;
#34983 = ADVANCED_FACE ( 'NONE', ( #11194 ), #18038, .F. ) ;
#34984 = ORIENTED_EDGE ( 'NONE', *, *, #7066, .T. ) ;
#34985 = CIRCLE ( 'NONE', #13894, 31.99999999999998224 ) ;
#34986 = EDGE_CURVE ( 'NONE', #39534, #31305, #36533, .T. ) ;
#34987 = DIRECTION ( 'NONE',  ( 0.000000000000000000, 0.000000000000000000, 1.000000000000000000 ) ) ;
#34988 = VERTEX_POINT ( 'NONE', #6555 ) ;
#34989 = STYLED_ITEM ( 'NONE', ( #1510 ), #35540 ) ;
#34990 = EDGE_LOOP ( 'NONE', ( #46956, #5558, #1969, #22278 ) ) ;
#34991 = ORIENTED_EDGE ( 'NONE', *, *, #28353, .T. ) ;
#34992 = ORIENTED_EDGE ( 'NONE', *, *, #33436, .T. ) ;
#34993 = ORIENTED_EDGE ( 'NONE', *, *, #36454, .T. ) ;
#34994 = EDGE_CURVE ( 'NONE', #13012, #38297, #29065, .T. ) ;
#34995 = CARTESIAN_POINT ( 'NONE',  ( 10.00000000000000000, -70.53064760720336324, 26.01480285779810231 ) ) ;
#34996 = ORIENTED_EDGE ( 'NONE', *, *, #14758, .T. ) ;
#34997 = VERTEX_POINT ( 'NONE', #22461 ) ;
#34998 = DIRECTION ( 'NONE',  ( -1.000000000000000000, -0.000000000000000000, 0.000000000000000000 ) ) ;
#34999 = ORIENTED_EDGE ( 'NONE', *, *, #25136, .T. ) ;
#35000 = CARTESIAN_POINT ( 'NONE',  ( 0.000000000000000000, 16.65560815589411092, 38.55633173627015253 ) ) ;
#35001 = LINE ( 'NONE', #47229, #19976 ) ;
#35002 = DIRECTION ( 'NONE',  ( -1.000000000000000000, -0.000000000000000000, -0.000000000000000000 ) ) ;
#35003 = ORIENTED_EDGE ( 'NONE', *, *, #35037, .T. ) ;
#35004 = LINE ( 'NONE', #27672, #27097 ) ;
#35005 = ORIENTED_EDGE ( 'NONE', *, *, #16423, .F. ) ;
#35006 = AXIS2_PLACEMENT_3D ( 'NONE', #36864, #18262, #44459 ) ;
#35007 = DIRECTION ( 'NONE',  ( 0.000000000000000000, 0.4539904997395414754, 0.8910065241883706744 ) ) ;
#35008 = CARTESIAN_POINT ( 'NONE',  ( 0.000000000000000000, 0.000000000000000000, 0.000000000000000000 ) ) ;
#35009 = EDGE_LOOP ( 'NONE', ( #2515, #3623, #9780, #28029 ) ) ;
#35010 = CYLINDRICAL_SURFACE ( 'NONE', #647, 82.00000000000000000 ) ;
#35011 = ORIENTED_EDGE ( 'NONE', *, *, #16521, .T. ) ;
#35012 = ORIENTED_EDGE ( 'NONE', *, *, #31642, .F. ) ;
#35013 = CARTESIAN_POINT ( 'NONE',  ( -22.17439115976385366, -112.2188447712574799, -2.500000000000000000 ) ) ;
#35014 = CARTESIAN_POINT ( 'NONE',  ( 0.000000000000000000, -32.34446384429989507, 26.79245525562703278 ) ) ;
#35015 = DIRECTION ( 'NONE',  ( 0.000000000000000000, -0.2334453638559125521, 0.9723699203976750027 ) ) ;
#35016 = CARTESIAN_POINT ( 'NONE',  ( 12.00000000000000000, -22.67460108101782978, -6.353146135317906840 ) ) ;
#35017 = DIRECTION ( 'NONE',  ( -1.000000000000000000, 0.000000000000000000, 0.000000000000000000 ) ) ;
#35018 = CARTESIAN_POINT ( 'NONE',  ( 0.000000000000000000, 77.19088730480532945, -6.903761155836913410 ) ) ;
#35019 = DIRECTION ( 'NONE',  ( -1.000000000000000000, 0.000000000000000000, -0.000000000000000000 ) ) ;
#35020 = CARTESIAN_POINT ( 'NONE',  ( 0.000000000000000000, -120.0000000000000000, -2.500000000000000000 ) ) ;
#35021 = VECTOR ( 'NONE', #23508, 1000.000000000000000 ) ;
#35022 = LINE ( 'NONE', #28401, #47360 ) ;
#35023 = LINE ( 'NONE', #16200, #36541 ) ;
#35024 = CARTESIAN_POINT ( 'NONE',  ( 0.000000000000000000, -72.35160999960801576, -20.41045688087902121 ) ) ;
#35025 = EDGE_CURVE ( 'NONE', #44331, #42385, #11524, .T. ) ;
#35027 = EDGE_CURVE ( 'NONE', #40610, #20645, #46721, .T. ) ;
#35026 = AXIS2_PLACEMENT_3D ( 'NONE', #4607, #19508, #917 ) ;
#35028 = DIRECTION ( 'NONE',  ( 0.000000000000000000, 0.000000000000000000, 1.000000000000000000 ) ) ;
#35029 = CARTESIAN_POINT ( 'NONE',  ( 0.000000000000000000, 35.92658777277510040, 10.74501242461294659 ) ) ;
#35030 = CARTESIAN_POINT ( 'NONE',  ( 0.000000000000000000, 0.000000000000000000, 0.000000000000000000 ) ) ;
#35031 = EDGE_CURVE ( 'NONE', #41733, #13231, #13903, .T. ) ;
#35033 = VECTOR ( 'NONE', #18732, 1000.000000000000000 ) ;
#35032 = CARTESIAN_POINT ( 'NONE',  ( -3.000000000000000000, 16.83928648764923253, 16.46020748918050458 ) ) ;
#35034 = EDGE_CURVE ( 'NONE', #33355, #28298, #25145, .T. ) ;
#35035 = ORIENTED_EDGE ( 'NONE', *, *, #39198, .T. ) ;
#35036 = ORIENTED_EDGE ( 'NONE', *, *, #9546, .T. ) ;
#35037 = EDGE_CURVE ( 'NONE', #10301, #41947, #36415, .T. ) ;
#35038 = DIRECTION ( 'NONE',  ( 0.000000000000000000, -0.4539904997395542430, 0.8910065241883641241 ) ) ;
#35039 = ADVANCED_FACE ( 'NONE', ( #32732 ), #14143, .T. ) ;
#35040 = ADVANCED_FACE ( 'NONE', ( #25629 ), #657, .T. ) ;
#35041 = CARTESIAN_POINT ( 'NONE',  ( 11.99999999999999822, -59.46389618801999433, 49.70050353004867816 ) ) ;
#35042 = CARTESIAN_POINT ( 'NONE',  ( -11.59999999999999787, 0.000000000000000000, 53.20000000000001705 ) ) ;
#35043 = ORIENTED_EDGE ( 'NONE', *, *, #26627, .T. ) ;
#35044 = EDGE_CURVE ( 'NONE', #24044, #5585, #13094, .T. ) ;
#35045 = ORIENTED_EDGE ( 'NONE', *, *, #28424, .F. ) ;
#35046 = CARTESIAN_POINT ( 'NONE',  ( 13.83832728059186046, -142.6495187161941089, 5.500000000000000000 ) ) ;
#35047 = ORIENTED_EDGE ( 'NONE', *, *, #38770, .T. ) ;
#35048 = DIRECTION ( 'NONE',  ( 0.000000000000000000, 0.000000000000000000, 1.000000000000000000 ) ) ;
#35049 = EDGE_CURVE ( 'NONE', #44578, #24728, #2163, .T. ) ;
#35050 = CARTESIAN_POINT ( 'NONE',  ( 11.99999999999999822, 0.000000000000000000, 0.000000000000000000 ) ) ;
#35051 = DIRECTION ( 'NONE',  ( -1.000000000000000000, 0.000000000000000000, 0.000000000000000000 ) ) ;
#35052 = ORIENTED_EDGE ( 'NONE', *, *, #30500, .T. ) ;
#35054 = ORIENTED_EDGE ( 'NONE', *, *, #38478, .F. ) ;
#35053 = CARTESIAN_POINT ( 'NONE',  ( -3.000000000000000000, -13.04903810567675038, 19.60159698893425428 ) ) ;
#35055 = VERTEX_POINT ( 'NONE', #38342 ) ;
#35056 = CIRCLE ( 'NONE', #35026, 82.00000000000000000 ) ;
#35057 = VECTOR ( 'NONE', #46945, 1000.000000000000000 ) ;
#35058 = VERTEX_POINT ( 'NONE', #45940 ) ;
#35059 = CIRCLE ( 'NONE', #47560, 82.00000000000000000 ) ;
#35060 = FACE_BOUND ( 'NONE', #35937, .T. ) ;
#35061 = CARTESIAN_POINT ( 'NONE',  ( 6.377742925735834234, -145.7647898336708181, 5.500000000000000000 ) ) ;
#35062 = FACE_OUTER_BOUND ( 'NONE', #34427, .T. ) ;
#35063 = DIRECTION ( 'NONE',  ( 1.000000000000000000, 0.000000000000000000, 0.000000000000000000 ) ) ;
#35065 = EDGE_LOOP ( 'NONE', ( #24032, #5327, #6566, #8719 ) ) ;
#35064 = DIRECTION ( 'NONE',  ( 0.000000000000000000, -0.6691306063588577935, -0.7431448254773946882 ) ) ;
#35066 = ORIENTED_EDGE ( 'NONE', *, *, #21162, .F. ) ;
#35067 = DIRECTION ( 'NONE',  ( -1.000000000000000000, -0.000000000000000000, -0.000000000000000000 ) ) ;
#35068 = VERTEX_POINT ( 'NONE', #4812 ) ;
#35069 = ORIENTED_EDGE ( 'NONE', *, *, #39638, .T. ) ;
#35070 = DIRECTION ( 'NONE',  ( 0.000000000000000000, 0.000000000000000000, 1.000000000000000000 ) ) ;
#35071 = ORIENTED_EDGE ( 'NONE', *, *, #2297, .T. ) ;
#35072 = DIRECTION ( 'NONE',  ( 0.000000000000000000, 0.000000000000000000, 1.000000000000000000 ) ) ;
#35073 = CARTESIAN_POINT ( 'NONE',  ( 10.00000000000000000, 30.80686688397010542, 21.53537804866092387 ) ) ;
#35074 = CYLINDRICAL_SURFACE ( 'NONE', #39, 77.49899999999999523 ) ;
#35075 = ORIENTED_EDGE ( 'NONE', *, *, #23956, .F. ) ;
#35076 = DIRECTION ( 'NONE',  ( -1.000000000000000000, -0.000000000000000000, -0.000000000000000000 ) ) ;
#35077 = CYLINDRICAL_SURFACE ( 'NONE', #2562, 31.99999999999999289 ) ;
#35078 = DIRECTION ( 'NONE',  ( 0.000000000000000000, 0.000000000000000000, -1.000000000000000000 ) ) ;
#35079 = CIRCLE ( 'NONE', #8517, 42.00000000000000000 ) ;
#35080 = DIRECTION ( 'NONE',  ( -1.000000000000000000, 0.000000000000000000, -0.000000000000000000 ) ) ;
#35081 = EDGE_CURVE ( 'NONE', #44069, #7113, #6834, .T. ) ;
#35082 = LINE ( 'NONE', #34843, #11399 ) ;
#35083 = CARTESIAN_POINT ( 'NONE',  ( 11.99999999999999822, 6.903761155837791819, 77.19088730480525840 ) ) ;
#35084 = DIRECTION ( 'NONE',  ( -0.000000000000000000, -0.000000000000000000, -1.000000000000000000 ) ) ;
#35085 = DIRECTION ( 'NONE',  ( -1.000000000000000000, -0.000000000000000000, -0.000000000000000000 ) ) ;
#35086 = EDGE_CURVE ( 'NONE', #2942, #37452, #8247, .T. ) ;
#35087 = DIRECTION ( 'NONE',  ( 1.000000000000000000, 0.000000000000000000, 0.000000000000000000 ) ) ;
#35088 = CARTESIAN_POINT ( 'NONE',  ( 12.13205353604972991, -140.1820037904669789, 5.500000000000000000 ) ) ;
#35089 = ADVANCED_FACE ( 'NONE', ( #41305 ), #27101, .F. ) ;
#35090 = ADVANCED_FACE ( 'NONE', ( #4349 ), #44972, .T. ) ;
#35091 = CARTESIAN_POINT ( 'NONE',  ( 15.00000000000000000, 0.000000000000000000, 0.000000000000000000 ) ) ;
#35092 = VECTOR ( 'NONE', #43773, 1000.000000000000000 ) ;
#35093 = VERTEX_POINT ( 'NONE', #15111 ) ;
#35094 = EDGE_CURVE ( 'NONE', #8812, #13864, #9172, .T. ) ;
#35095 = DIRECTION ( 'NONE',  ( 0.000000000000000000, -0.9723699203976789995, 0.2334453638558956767 ) ) ;
#35096 = AXIS2_PLACEMENT_3D ( 'NONE', #25124, #21464, #3088 ) ;
#35097 = DIRECTION ( 'NONE',  ( 0.000000000000000000, 0.000000000000000000, 1.000000000000000000 ) ) ;
#35098 = ORIENTED_EDGE ( 'NONE', *, *, #38484, .T. ) ;
#35099 = VERTEX_POINT ( 'NONE', #38594 ) ;
#35100 = FACE_OUTER_BOUND ( 'NONE', #35499, .T. ) ;
#35101 = EDGE_LOOP ( 'NONE', ( #25940, #25482, #15675, #46014 ) ) ;
#35102 = ORIENTED_EDGE ( 'NONE', *, *, #3299, .T. ) ;
#35103 = DIRECTION ( 'NONE',  ( 0.000000000000000000, -0.9723699203976789995, 0.2334453638558956767 ) ) ;
#35104 = DIRECTION ( 'NONE',  ( 0.000000000000000000, 0.000000000000000000, 1.000000000000000000 ) ) ;
#35106 = ORIENTED_EDGE ( 'NONE', *, *, #24588, .T. ) ;
#35105 = DIRECTION ( 'NONE',  ( -1.000000000000000000, -0.000000000000000000, 0.000000000000000000 ) ) ;
#35107 = ORIENTED_EDGE ( 'NONE', *, *, #9608, .F. ) ;
#35108 = DIRECTION ( 'NONE',  ( 1.000000000000000000, 0.000000000000000000, 0.000000000000000000 ) ) ;
#35109 = VERTEX_POINT ( 'NONE', #19004 ) ;
#35110 = EDGE_LOOP ( 'NONE', ( #23611, #23430, #16387, #39219 ) ) ;
#35111 = DIRECTION ( 'NONE',  ( -1.000000000000000000, 0.000000000000000000, 0.000000000000000000 ) ) ;
#35112 = CYLINDRICAL_SURFACE ( 'NONE', #34061, 77.49899999999999523 ) ;
#35113 = CARTESIAN_POINT ( 'NONE',  ( 20.85212586905262100, -130.9402397935870965, 5.500000000000000000 ) ) ;
#35114 = ADVANCED_FACE ( 'NONE', ( #5060 ), #4575, .T. ) ;
#35115 = ORIENTED_EDGE ( 'NONE', *, *, #18436, .T. ) ;
#35116 = ORIENTED_EDGE ( 'NONE', *, *, #3062, .F. ) ;
#35117 = CIRCLE ( 'NONE', #30454, 31.99999999999999289 ) ;
#35118 = CARTESIAN_POINT ( 'NONE',  ( 10.00000000000000000, -17.67226234102801286, -33.17418723428327354 ) ) ;
#35119 = ORIENTED_EDGE ( 'NONE', *, *, #4240, .T. ) ;
#35120 = FACE_OUTER_BOUND ( 'NONE', #955, .T. ) ;
#35121 = VECTOR ( 'NONE', #31516, 1000.000000000000000 ) ;
#35122 = DIRECTION ( 'NONE',  ( -1.000000000000000000, 0.000000000000000000, 0.000000000000000000 ) ) ;
#35123 = LINE ( 'NONE', #32604, #1758 ) ;
#35124 = DIRECTION ( 'NONE',  ( -1.000000000000000000, 0.000000000000000000, 0.000000000000000000 ) ) ;
#35125 = CARTESIAN_POINT ( 'NONE',  ( 10.00000000000000000, -77.19088730480518734, -6.903761155838607166 ) ) ;
#35126 = LINE ( 'NONE', #8226, #6548 ) ;
#35127 = DIRECTION ( 'NONE',  ( 0.000000000000000000, 0.000000000000000000, 1.000000000000000000 ) ) ;
#35128 = ORIENTED_EDGE ( 'NONE', *, *, #29570, .T. ) ;
#35129 = CARTESIAN_POINT ( 'NONE',  ( 11.99999999999999822, -75.16055320797016748, -18.89407956138335365 ) ) ;
#35130 = CARTESIAN_POINT ( 'NONE',  ( -1.474095553543409487, -120.2775649455957989, -2.500000000000000000 ) ) ;
#35131 = DIRECTION ( 'NONE',  ( -1.000000000000000000, 0.000000000000000000, 0.000000000000000000 ) ) ;
#35132 = CARTESIAN_POINT ( 'NONE',  ( 12.00000000000000355, 0.000000000000000000, 21.00000000000000000 ) ) ;
#35133 = ORIENTED_EDGE ( 'NONE', *, *, #25216, .F. ) ;
#35134 = CIRCLE ( 'NONE', #32048, 77.49899999999999523 ) ;
#35135 =( NAMED_UNIT ( * ) PLANE_ANGLE_UNIT ( ) SI_UNIT ( $, .RADIAN. ) );
#35136 = EDGE_CURVE ( 'NONE', #18133, #2410, #13868, .T. ) ;
#35137 = DIRECTION ( 'NONE',  ( 0.000000000000000000, 0.9510565162951523099, 0.3090169943749514481 ) ) ;
#35138 = DIRECTION ( 'NONE',  ( 0.000000000000000000, -0.9876883405951393247, 0.1564344650402204329 ) ) ;
#35139 = EDGE_CURVE ( 'NONE', #17971, #25651, #33936, .T. ) ;
#35140 = DIRECTION ( 'NONE',  ( 0.000000000000000000, 0.000000000000000000, 1.000000000000000000 ) ) ;
#35141 = DIRECTION ( 'NONE',  ( -1.000000000000000000, 0.000000000000000000, 0.000000000000000000 ) ) ;
#35142 = EDGE_CURVE ( 'NONE', #4911, #6805, #26843, .T. ) ;
#35143 = CARTESIAN_POINT ( 'NONE',  ( 10.00000000000000000, -30.00120703465222149, 22.64427369931158296 ) ) ;
#35144 = CARTESIAN_POINT ( 'NONE',  ( 5.999999999999999112, -46.11716303203233736, 67.80270845531873647 ) ) ;
#35145 = EDGE_LOOP ( 'NONE', ( #14777, #21684, #30217, #16165 ) ) ;
#35146 = EDGE_CURVE ( 'NONE', #14490, #28940, #42805, .T. ) ;
#35147 = DIRECTION ( 'NONE',  ( 0.000000000000000000, 0.000000000000000000, 1.000000000000000000 ) ) ;
#35148 = EDGE_CURVE ( 'NONE', #1345, #41033, #25584, .T. ) ;
#35149 = ORIENTED_EDGE ( 'NONE', *, *, #43456, .F. ) ;
#35150 = SURFACE_SIDE_STYLE ('',( #31262 ) ) ;
#35151 = DIRECTION ( 'NONE',  ( 1.000000000000000000, 0.000000000000000000, 0.000000000000000000 ) ) ;
#35152 = ORIENTED_EDGE ( 'NONE', *, *, #47854, .T. ) ;
#35153 = AXIS2_PLACEMENT_3D ( 'NONE', #47248, #7326, #44531 ) ;
#35154 = ORIENTED_EDGE ( 'NONE', *, *, #17131, .F. ) ;
#35155 = VECTOR ( 'NONE', #40965, 1000.000000000000000 ) ;
#35156 = ORIENTED_EDGE ( 'NONE', *, *, #14984, .F. ) ;
#35157 = DIRECTION ( 'NONE',  ( -1.000000000000000000, -0.000000000000000000, 0.000000000000000000 ) ) ;
#35158 = ORIENTED_EDGE ( 'NONE', *, *, #27522, .F. ) ;
#35159 = EDGE_CURVE ( 'NONE', #9450, #26893, #31881, .T. ) ;
#35160 = AXIS2_PLACEMENT_3D ( 'NONE', #44338, #18628, #17 ) ;
#35161 = CARTESIAN_POINT ( 'NONE',  ( 11.99999999999999822, 26.01480285779837232, 70.53064760720326376 ) ) ;
#35163 = EDGE_LOOP ( 'NONE', ( #22412, #44110, #11113, #45361 ) ) ;
#35162 = CARTESIAN_POINT ( 'NONE',  ( 10.00000000000000000, 0.000000000000000000, 0.000000000000000000 ) ) ;
#35164 = ORIENTED_EDGE ( 'NONE', *, *, #32403, .T. ) ;
#35165 = ORIENTED_EDGE ( 'NONE', *, *, #17681, .T. ) ;
#35166 = ORIENTED_EDGE ( 'NONE', *, *, #40303, .F. ) ;
#35167 = ORIENTED_EDGE ( 'NONE', *, *, #24862, .F. ) ;
#35168 = CARTESIAN_POINT ( 'NONE',  ( 10.00000000000000000, -35.91791733033525702, 68.67312586194982771 ) ) ;
#35170 = ORIENTED_EDGE ( 'NONE', *, *, #17179, .F. ) ;
#35169 = DIRECTION ( 'NONE',  ( -1.000000000000000000, 0.000000000000000000, -0.000000000000000000 ) ) ;
#35171 = DIRECTION ( 'NONE',  ( -1.000000000000000000, 0.000000000000000000, 0.000000000000000000 ) ) ;
#35172 = EDGE_CURVE ( 'NONE', #46920, #3686, #35767, .T. ) ;
#35173 = ORIENTED_EDGE ( 'NONE', *, *, #46704, .T. ) ;
#35174 = ORIENTED_EDGE ( 'NONE', *, *, #10407, .T. ) ;
#35175 = DIRECTION ( 'NONE',  ( 0.000000000000000000, -0.3090169943749349057, -0.9510565162951577500 ) ) ;
#35176 = ORIENTED_EDGE ( 'NONE', *, *, #1035, .F. ) ;
#35177 = ORIENTED_EDGE ( 'NONE', *, *, #31252, .T. ) ;
#35178 = DIRECTION ( 'NONE',  ( 0.4279312458753000703, 0.9038112904824842087, 0.000000000000000000 ) ) ;
#35179 = LINE ( 'NONE', #38880, #42869 ) ;
#35180 = ADVANCED_FACE ( 'NONE', ( #12180 ), #42028, .T. ) ;
#35181 = ORIENTED_EDGE ( 'NONE', *, *, #31700, .T. ) ;
#35182 = DIRECTION ( 'NONE',  ( -1.000000000000000000, -0.000000000000000000, 0.000000000000000000 ) ) ;
#35183 = CARTESIAN_POINT ( 'NONE',  ( 10.00000000000000000, -76.66974797899830207, -11.30684508768422170 ) ) ;
#35184 = DIRECTION ( 'NONE',  ( 0.000000000000000000, -0.07845909572785220165, 0.9969173337331274087 ) ) ;
#35185 = ADVANCED_FACE ( 'NONE', ( #36536 ), #42752, .T. ) ;
#35186 = ORIENTED_EDGE ( 'NONE', *, *, #36586, .F. ) ;
#35187 = VERTEX_POINT ( 'NONE', #31984 ) ;
#35188 = DIRECTION ( 'NONE',  ( 0.000000000000000000, 0.000000000000000000, 1.000000000000000000 ) ) ;
#35189 = VECTOR ( 'NONE', #4542, 1000.000000000000114 ) ;
#35190 = CYLINDRICAL_SURFACE ( 'NONE', #42301, 37.49900000000000233 ) ;
#35191 = ORIENTED_EDGE ( 'NONE', *, *, #31332, .T. ) ;
#35192 = CIRCLE ( 'NONE', #14093, 31.99999999999998224 ) ;
#35193 = CARTESIAN_POINT ( 'NONE',  ( 10.00000000000000000, 0.000000000000000000, 0.000000000000000000 ) ) ;
#35194 = ORIENTED_EDGE ( 'NONE', *, *, #41246, .F. ) ;
#35195 = AXIS2_PLACEMENT_3D ( 'NONE', #26531, #26767, #38037 ) ;
#35196 = AXIS2_PLACEMENT_3D ( 'NONE', #11034, #14717, #8080 ) ;
#35197 = DIRECTION ( 'NONE',  ( -1.000000000000000000, -0.000000000000000000, 0.000000000000000000 ) ) ;
#35198 = DIRECTION ( 'NONE',  ( -1.000000000000000000, -0.000000000000000000, -0.000000000000000000 ) ) ;
#35199 = CARTESIAN_POINT ( 'NONE',  ( 10.00000000000000000, 74.65491531819105830, 8.830959090343693418 ) ) ;
#35200 = EDGE_LOOP ( 'NONE', ( #6673, #11016 ) ) ;
#35201 = FACE_OUTER_BOUND ( 'NONE', #21763, .T. ) ;
#35202 = EDGE_CURVE ( 'NONE', #32964, #13148, #28944, .T. ) ;
#35203 = AXIS2_PLACEMENT_3D ( 'NONE', #3189, #47280, #36964 ) ;
#35204 = EDGE_CURVE ( 'NONE', #20595, #43018, #13134, .T. ) ;
#35205 = EDGE_CURVE ( 'NONE', #708, #21020, #10005, .T. ) ;
#35206 = CARTESIAN_POINT ( 'NONE',  ( 10.00000000000000000, 40.98264845739763018, -9.188173127306866306 ) ) ;
#35207 = CIRCLE ( 'NONE', #14100, 16.00000000000000000 ) ;
#35208 = LINE ( 'NONE', #36163, #28679 ) ;
#35209 = DIRECTION ( 'NONE',  ( 0.000000000000000000, 0.9510565162951544194, -0.3090169943749447867 ) ) ;
#35210 = CIRCLE ( 'NONE', #30529, 82.00000000000000000 ) ;
#35211 = LINE ( 'NONE', #42082, #29350 ) ;
#35212 = FACE_OUTER_BOUND ( 'NONE', #12276, .T. ) ;
#35213 =( NAMED_UNIT ( * ) SI_UNIT ( $, .STERADIAN. ) SOLID_ANGLE_UNIT ( ) );
#35214 = EDGE_CURVE ( 'NONE', #6714, #13681, #39070, .T. ) ;
#35215 = ORIENTED_EDGE ( 'NONE', *, *, #42033, .F. ) ;
#35216 = DIRECTION ( 'NONE',  ( -1.000000000000000000, 0.000000000000000000, -0.000000000000000000 ) ) ;
#35217 = CARTESIAN_POINT ( 'NONE',  ( -25.50183398199384754, -112.6408924756582053, 5.500000000000000000 ) ) ;
#35218 = ORIENTED_EDGE ( 'NONE', *, *, #22820, .F. ) ;
#35219 = ORIENTED_EDGE ( 'NONE', *, *, #1776, .T. ) ;
#35220 = VECTOR ( 'NONE', #38273, 1000.000000000000000 ) ;
#35221 = VECTOR ( 'NONE', #14113, 1000.000000000000000 ) ;
#35222 = CARTESIAN_POINT ( 'NONE',  ( 10.00000000000000000, -55.19960302592029677, -51.03279382321147750 ) ) ;
#35223 = VECTOR ( 'NONE', #24548, 1000.000000000000000 ) ;
#35224 = AXIS2_PLACEMENT_3D ( 'NONE', #13451, #29343, #6583 ) ;
#35225 = ORIENTED_EDGE ( 'NONE', *, *, #4458, .F. ) ;
#35226 = ORIENTED_EDGE ( 'NONE', *, *, #26869, .F. ) ;
#35227 = ORIENTED_EDGE ( 'NONE', *, *, #30844, .T. ) ;
#35228 = CIRCLE ( 'NONE', #24305, 16.00000000000000000 ) ;
#35229 = CIRCLE ( 'NONE', #21148, 16.00000000000000000 ) ;
#35230 = DIRECTION ( 'NONE',  ( 1.000000000000000000, -0.000000000000000000, -0.000000000000000000 ) ) ;
#35231 = EDGE_CURVE ( 'NONE', #21898, #36090, #42061, .T. ) ;
#35232 = ORIENTED_EDGE ( 'NONE', *, *, #28789, .F. ) ;
#35233 = CIRCLE ( 'NONE', #18040, 1.000000000000000888 ) ;
#35234 = EDGE_LOOP ( 'NONE', ( #14888, #42151, #18115, #34920 ) ) ;
#35235 = LINE ( 'NONE', #1237, #38787 ) ;
#35236 = EDGE_LOOP ( 'NONE', ( #33495, #21693, #303, #45783 ) ) ;
#35237 = CARTESIAN_POINT ( 'NONE',  ( 11.99999999999999822, 0.000000000000000000, 0.000000000000000000 ) ) ;
#35238 = EDGE_CURVE ( 'NONE', #22545, #46408, #41260, .T. ) ;
#35239 = DIRECTION ( 'NONE',  ( 0.000000000000000000, 0.1045284632676448111, 0.9945218953682742891 ) ) ;
#35240 = DIRECTION ( 'NONE',  ( -1.000000000000000000, 0.000000000000000000, 0.000000000000000000 ) ) ;
#35241 = ADVANCED_FACE ( 'NONE', ( #23901 ), #10605, .T. ) ;
#35242 = ORIENTED_EDGE ( 'NONE', *, *, #162, .F. ) ;
#35243 = DIRECTION ( 'NONE',  ( -1.000000000000000000, 0.000000000000000000, 0.000000000000000000 ) ) ;
#35244 = VERTEX_POINT ( 'NONE', #20703 ) ;
#35245 = PLANE ( 'NONE',  #23493 ) ;
#35246 = DIRECTION ( 'NONE',  ( 0.000000000000000000, 0.000000000000000000, 1.000000000000000000 ) ) ;
#35247 = DIRECTION ( 'NONE',  ( 0.000000000000000000, 0.000000000000000000, 1.000000000000000000 ) ) ;
#35248 = ORIENTED_EDGE ( 'NONE', *, *, #30627, .F. ) ;
#35249 = ORIENTED_EDGE ( 'NONE', *, *, #26798, .F. ) ;
#35250 = CARTESIAN_POINT ( 'NONE',  ( 0.000000000000000000, -4.261787119644969479, -26.19803753235780519 ) ) ;
#35251 = CARTESIAN_POINT ( 'NONE',  ( 0.000000000000000000, -0.8828120875903202602, 37.48860685352291000 ) ) ;
#35252 = EDGE_CURVE ( 'NONE', #41733, #45238, #28059, .T. ) ;
#35253 = VERTEX_POINT ( 'NONE', #12646 ) ;
#35254 = DIRECTION ( 'NONE',  ( 0.000000000000000000, 0.000000000000000000, -1.000000000000000000 ) ) ;
#35255 = DIRECTION ( 'NONE',  ( 1.000000000000000000, 0.000000000000000000, 0.000000000000000000 ) ) ;
#35256 = CARTESIAN_POINT ( 'NONE',  ( 10.00000000000000000, -10.41901085202107247, 40.68715046381925049 ) ) ;
#35257 = VERTEX_POINT ( 'NONE', #2113 ) ;
#35258 = CARTESIAN_POINT ( 'NONE',  ( 0.000000000000000000, 55.19960302592066625, 51.03279382321107249 ) ) ;
#35259 = EDGE_CURVE ( 'NONE', #27310, #5836, #10786, .T. ) ;
#35260 = CARTESIAN_POINT ( 'NONE',  ( -4.653126046682595884, -146.1313684676804314, 2.500000000000000000 ) ) ;
#35261 = EDGE_CURVE ( 'NONE', #975, #43484, #35639, .T. ) ;
#35263 = AXIS2_PLACEMENT_3D ( 'NONE', #40452, #30, #36752 ) ;
#35262 = FACE_OUTER_BOUND ( 'NONE', #22069, .T. ) ;
#35264 = VECTOR ( 'NONE', #26815, 1000.000000000000000 ) ;
#35265 = CARTESIAN_POINT ( 'NONE',  ( -12.00000000000000000, 0.000000000000000000, 0.000000000000000000 ) ) ;
#35266 = DIRECTION ( 'NONE',  ( 0.7950889364178796992, -0.6064928550163511956, 0.000000000000000000 ) ) ;
#35267 = DIRECTION ( 'NONE',  ( 0.000000000000000000, -0.1045284632676429099, -0.9945218953682744001 ) ) ;
#35268 = CIRCLE ( 'NONE', #42293, 42.00000000000000000 ) ;
#35269 = CIRCLE ( 'NONE', #25889, 32.50000000000000000 ) ;
#35270 = PLANE ( 'NONE',  #4935 ) ;
#35271 = CARTESIAN_POINT ( 'NONE',  ( 15.00000000000000000, 16.61724383029361718, -20.69703378468926402 ) ) ;
#35272 = CARTESIAN_POINT ( 'NONE',  ( 5.000000000000000000, 41.91543099594818500, 2.663952781846291362 ) ) ;
#35273 = FACE_OUTER_BOUND ( 'NONE', #40331, .T. ) ;
#35274 = AXIS2_PLACEMENT_3D ( 'NONE', #25660, #11720, #10756 ) ;
#35275 = ORIENTED_EDGE ( 'NONE', *, *, #20449, .F. ) ;
#35276 = EDGE_CURVE ( 'NONE', #32891, #38425, #13360, .T. ) ;
#35277 = DIRECTION ( 'NONE',  ( 0.000000000000000000, 0.000000000000000000, 1.000000000000000000 ) ) ;
#35278 = CARTESIAN_POINT ( 'NONE',  ( 10.00000000000000000, -75.11764819372145041, -2.946379043147127064 ) ) ;
#35279 = CARTESIAN_POINT ( 'NONE',  ( 5.999999999999999112, 60.67117009219215618, -55.16347631942977614 ) ) ;
#35280 = EDGE_LOOP ( 'NONE', ( #11874, #10028, #28751, #42492 ) ) ;
#35281 = COLOUR_RGB ( '', 0.31764706, 0.68627451, 0.89019608) ;
#35282 = FACE_OUTER_BOUND ( 'NONE', #35065, .T. ) ;
#35283 = DIRECTION ( 'NONE',  ( 0.000000000000000000, 0.000000000000000000, -1.000000000000000000 ) ) ;
#35284 = ORIENTED_EDGE ( 'NONE', *, *, #4531, .T. ) ;
#35285 = CARTESIAN_POINT ( 'NONE',  ( 0.000000000000000000, 31.46837873494978055, 68.27212725128286763 ) ) ;
#35286 = VECTOR ( 'NONE', #1133, 1000.000000000000000 ) ;
#35287 = DIRECTION ( 'NONE',  ( 0.000000000000000000, 0.000000000000000000, 1.000000000000000000 ) ) ;
#35288 = AXIS2_PLACEMENT_3D ( 'NONE', #26522, #4256, #11833 ) ;
#35289 = LINE ( 'NONE', #19623, #38346 ) ;
#35290 = VERTEX_POINT ( 'NONE', #39306 ) ;
#35291 = CARTESIAN_POINT ( 'NONE',  ( 12.13205353604972991, -140.1820037904669789, 5.500000000000000000 ) ) ;
#35292 = AXIS2_PLACEMENT_3D ( 'NONE', #37591, #18509, #26341 ) ;
#35293 = ORIENTED_EDGE ( 'NONE', *, *, #37559, .T. ) ;
#35294 = EDGE_CURVE ( 'NONE', #26344, #36873, #12364, .T. ) ;
#35295 = VECTOR ( 'NONE', #14306, 1000.000000000000000 ) ;
#35296 = ORIENTED_EDGE ( 'NONE', *, *, #29556, .T. ) ;
#35297 = VECTOR ( 'NONE', #35325, 1000.000000000000000 ) ;
#35298 = EDGE_CURVE ( 'NONE', #20236, #11961, #612, .T. ) ;
#35299 = CARTESIAN_POINT ( 'NONE',  ( 0.000000000000000000, 51.02545421589402252, -55.20638768913705263 ) ) ;
#35300 = ORIENTED_EDGE ( 'NONE', *, *, #318, .F. ) ;
#35301 = EDGE_CURVE ( 'NONE', #28791, #10091, #27570, .T. ) ;
#35302 = LINE ( 'NONE', #38256, #41779 ) ;
#35303 = DIRECTION ( 'NONE',  ( 0.000000000000000000, 0.000000000000000000, 1.000000000000000000 ) ) ;
#35304 = DIRECTION ( 'NONE',  ( 1.000000000000000000, 0.000000000000000000, 0.000000000000000000 ) ) ;
#35305 = CARTESIAN_POINT ( 'NONE',  ( 10.00000000000000000, 0.000000000000000000, 0.000000000000000000 ) ) ;
#35306 = ORIENTED_EDGE ( 'NONE', *, *, #15688, .F. ) ;
#35307 = CARTESIAN_POINT ( 'NONE',  ( 0.000000000000000000, 25.88420570971400991, 27.13269053701105449 ) ) ;
#35308 = ORIENTED_EDGE ( 'NONE', *, *, #19235, .T. ) ;
#35309 = ORIENTED_EDGE ( 'NONE', *, *, #3242, .T. ) ;
#35310 = ADVANCED_FACE ( 'NONE', ( #12891 ), #31752, .T. ) ;
#35311 = DIRECTION ( 'NONE',  ( -1.000000000000000000, -0.000000000000000000, 0.000000000000000000 ) ) ;
#35312 = AXIS2_PLACEMENT_3D ( 'NONE', #29874, #3939, #34500 ) ;
#35313 = CARTESIAN_POINT ( 'NONE',  ( 21.07894319797337701, -103.8699611390234878, -2.500000000000000444 ) ) ;
#35314 = CARTESIAN_POINT ( 'NONE',  ( 6.000000000000000000, -44.99326035066007279, -68.55367621811190304 ) ) ;
#35315 = DIRECTION ( 'NONE',  ( 0.000000000000000000, 1.000000000000000000, 0.000000000000000000 ) ) ;
#35316 = ORIENTED_EDGE ( 'NONE', *, *, #37682, .T. ) ;
#35317 = LINE ( 'NONE', #15755, #34692 ) ;
#35318 = CARTESIAN_POINT ( 'NONE',  ( 0.000000000000000000, -76.66974797899828786, -11.30684508768421992 ) ) ;
#35319 = CARTESIAN_POINT ( 'NONE',  ( 11.99999999999999822, 0.000000000000000000, 0.000000000000000000 ) ) ;
#35320 = EDGE_CURVE ( 'NONE', #24209, #39037, #27830, .T. ) ;
#35321 = CYLINDRICAL_SURFACE ( 'NONE', #30698, 12.49999999999999645 ) ;
#35322 = DIRECTION ( 'NONE',  ( -1.000000000000000000, 0.000000000000000000, 0.000000000000000000 ) ) ;
#35323 = CARTESIAN_POINT ( 'NONE',  ( -0.4966694826856976608, -121.4153866697721611, -2.500000000000000000 ) ) ;
#35324 = EDGE_CURVE ( 'NONE', #1645, #30814, #6923, .T. ) ;
#35325 = DIRECTION ( 'NONE',  ( -1.000000000000000000, -0.000000000000000000, -0.000000000000000000 ) ) ;
#35326 = CYLINDRICAL_SURFACE ( 'NONE', #18511, 77.49899999999999523 ) ;
#35327 = CARTESIAN_POINT ( 'NONE',  ( 10.00000000000000000, -79.10210256391353312, -21.60688246758667574 ) ) ;
#35328 = DIRECTION ( 'NONE',  ( -1.000000000000000000, -1.390371824233641368E-16, 0.000000000000000000 ) ) ;
#35329 = ORIENTED_EDGE ( 'NONE', *, *, #7013, .F. ) ;
#35330 = AXIS2_PLACEMENT_3D ( 'NONE', #36107, #21892, #43471 ) ;
#35331 = EDGE_CURVE ( 'NONE', #40544, #41750, #14998, .T. ) ;
#35332 = ORIENTED_EDGE ( 'NONE', *, *, #17739, .F. ) ;
#35333 = CARTESIAN_POINT ( 'NONE',  ( -2.500000000000000000, 16.00000000000000000, -10.00000000000000178 ) ) ;
#35334 = ORIENTED_EDGE ( 'NONE', *, *, #21441, .T. ) ;
#35335 = DIRECTION ( 'NONE',  ( -1.000000000000000000, 0.000000000000000000, -0.000000000000000000 ) ) ;
#35336 = VECTOR ( 'NONE', #24719, 1000.000000000000000 ) ;
#35337 = LINE ( 'NONE', #43654, #21324 ) ;
#35338 = AXIS2_PLACEMENT_3D ( 'NONE', #3534, #22132, #33399 ) ;
#35339 = VERTEX_POINT ( 'NONE', #25748 ) ;
#35340 = ADVANCED_FACE ( 'NONE', ( #22342 ), #26493, .T. ) ;
#35341 = AXIS2_PLACEMENT_3D ( 'NONE', #33727, #18568, #41575 ) ;
#35342 = CARTESIAN_POINT ( 'NONE',  ( 0.000000000000000000, 8.688484142253939169, 21.88630264137371029 ) ) ;
#35343 = VERTEX_POINT ( 'NONE', #44844 ) ;
#35344 = ORIENTED_EDGE ( 'NONE', *, *, #23362, .F. ) ;
#35345 = CARTESIAN_POINT ( 'NONE',  ( 15.00000000000000000, 8.688484142253932063, -21.88630264137371029 ) ) ;
#35346 = ADVANCED_FACE ( 'NONE', ( #45322 ), #14516, .F. ) ;
#35347 = CARTESIAN_POINT ( 'NONE',  ( 6.000000000000000000, -10.30890764327323161, -81.34940948281348483 ) ) ;
#35348 = DIRECTION ( 'NONE',  ( 0.000000000000000000, -0.4539904997395541875, 0.8910065241883642351 ) ) ;
#35349 = ORIENTED_EDGE ( 'NONE', *, *, #30978, .T. ) ;
#35350 = EDGE_CURVE ( 'NONE', #34700, #29866, #37501, .T. ) ;
#35351 = DIRECTION ( 'NONE',  ( 0.000000000000000000, 0.000000000000000000, 1.000000000000000000 ) ) ;
#35352 = ORIENTED_EDGE ( 'NONE', *, *, #27913, .T. ) ;
#35353 = EDGE_CURVE ( 'NONE', #37286, #46628, #40690, .T. ) ;
#35354 = CARTESIAN_POINT ( 'NONE',  ( 6.000000000000000000, 80.28980883073781172, -16.65972982744850128 ) ) ;
#35355 = DIRECTION ( 'NONE',  ( 0.000000000000000000, -0.3090169943749349057, -0.9510565162951577500 ) ) ;
#35356 = DIRECTION ( 'NONE',  ( -0.000000000000000000, -0.000000000000000000, -1.000000000000000000 ) ) ;
#35357 = CIRCLE ( 'NONE', #42428, 31.99999999999999289 ) ;
#35358 = VERTEX_POINT ( 'NONE', #29670 ) ;
#35359 = AXIS2_PLACEMENT_3D ( 'NONE', #43858, #22556, #17905 ) ;
#35360 = ORIENTED_EDGE ( 'NONE', *, *, #37768, .F. ) ;
#35361 = VERTEX_POINT ( 'NONE', #30408 ) ;
#35362 = CARTESIAN_POINT ( 'NONE',  ( 10.00000000000000000, 0.000000000000000000, 0.000000000000000000 ) ) ;
#35363 = ORIENTED_EDGE ( 'NONE', *, *, #43280, .F. ) ;
#35364 = ADVANCED_FACE ( 'NONE', ( #3977 ), #26731, .T. ) ;
#35365 = CIRCLE ( 'NONE', #33778, 42.00000000000000000 ) ;
#35366 = DIRECTION ( 'NONE',  ( -1.000000000000000000, 0.000000000000000000, -0.000000000000000000 ) ) ;
#35367 = CARTESIAN_POINT ( 'NONE',  ( 0.000000000000000000, 0.000000000000000000, 0.000000000000000000 ) ) ;
#35368 = PLANE ( 'NONE',  #31469 ) ;
#35369 = CARTESIAN_POINT ( 'NONE',  ( 0.000000000000000000, -71.87247863392386193, -39.47590169984923136 ) ) ;
#35370 = CARTESIAN_POINT ( 'NONE',  ( 10.00000000000000000, 37.22597642581158084, -5.202137450156524068 ) ) ;
#35371 = DIRECTION ( 'NONE',  ( 0.000000000000000000, 0.000000000000000000, 1.000000000000000000 ) ) ;
#35372 = CARTESIAN_POINT ( 'NONE',  ( 11.99999999999999822, -24.73286445877757345, 73.44644590900053061 ) ) ;
#35373 = ORIENTED_EDGE ( 'NONE', *, *, #24315, .T. ) ;
#35374 = CARTESIAN_POINT ( 'NONE',  ( 11.99999999999999822, -76.69515212745996280, -29.01471420065643869 ) ) ;
#35375 = CARTESIAN_POINT ( 'NONE',  ( 0.000000000000000000, -70.52718814184240159, -26.02418014898383802 ) ) ;
#35376 = DIRECTION ( 'NONE',  ( -1.000000000000000000, -0.000000000000000000, 0.000000000000000000 ) ) ;
#35377 = DIRECTION ( 'NONE',  ( 1.000000000000000000, -0.000000000000000000, -0.000000000000000000 ) ) ;
#35378 = ORIENTED_EDGE ( 'NONE', *, *, #9895, .F. ) ;
#35379 = DIRECTION ( 'NONE',  ( -1.000000000000000000, 0.000000000000000000, -0.000000000000000000 ) ) ;
#35380 = AXIS2_PLACEMENT_3D ( 'NONE', #3296, #44190, #33415 ) ;
#35381 = CARTESIAN_POINT ( 'NONE',  ( -10.00000000000000000, 0.000000000000000000, 0.000000000000000000 ) ) ;
#35382 = CARTESIAN_POINT ( 'NONE',  ( 0.000000000000000000, -1.278221433540145613, -26.51162292216073979 ) ) ;
#35383 = DIRECTION ( 'NONE',  ( -1.000000000000000000, 0.000000000000000000, 0.000000000000000000 ) ) ;
#35384 = DIRECTION ( 'NONE',  ( 0.000000000000000000, 0.000000000000000000, 1.000000000000000000 ) ) ;
#35385 = FACE_OUTER_BOUND ( 'NONE', #46571, .T. ) ;
#35386 = CARTESIAN_POINT ( 'NONE',  ( 0.000000000000000000, 0.000000000000000000, 0.000000000000000000 ) ) ;
#35387 = ORIENTED_EDGE ( 'NONE', *, *, #44273, .F. ) ;
#35388 = CARTESIAN_POINT ( 'NONE',  ( 4.999999999999999112, 40.98264845739763018, -9.188173127306860977 ) ) ;
#35389 = CIRCLE ( 'NONE', #42420, 77.49899999999999523 ) ;
#35390 = VERTEX_POINT ( 'NONE', #11333 ) ;
#35391 = AXIS2_PLACEMENT_3D ( 'NONE', #21625, #33112, #21365 ) ;
#35392 = DIRECTION ( 'NONE',  ( 1.000000000000000000, 0.000000000000000000, 0.000000000000000000 ) ) ;
#35393 = DIRECTION ( 'NONE',  ( -1.000000000000000000, -0.000000000000000000, 0.000000000000000000 ) ) ;
#35394 = EDGE_LOOP ( 'NONE', ( #14414, #25537, #26901, #11698 ) ) ;
#35395 = EDGE_LOOP ( 'NONE', ( #29819, #31755, #12616, #16691 ) ) ;
#35396 = AXIS2_PLACEMENT_3D ( 'NONE', #47256, #13478, #21549 ) ;
#35397 = VECTOR ( 'NONE', #35975, 1000.000000000000000 ) ;
#35398 = ORIENTED_EDGE ( 'NONE', *, *, #3435, .F. ) ;
#35399 = CIRCLE ( 'NONE', #15070, 42.00000000000000000 ) ;
#35400 = CARTESIAN_POINT ( 'NONE',  ( -26.29030328629083968, -123.6496510949466341, 5.500000000000000000 ) ) ;
#35401 = ORIENTED_EDGE ( 'NONE', *, *, #47834, .T. ) ;
#35402 = CIRCLE ( 'NONE', #43281, 82.00000000000000000 ) ;
#35403 = ORIENTED_EDGE ( 'NONE', *, *, #40362, .T. ) ;
#35404 = AXIS2_PLACEMENT_3D ( 'NONE', #10098, #20151, #25019 ) ;
#35405 = EDGE_CURVE ( 'NONE', #47865, #30860, #28744, .T. ) ;
#35406 = CARTESIAN_POINT ( 'NONE',  ( 11.99999999999999822, -69.42325613327415113, -34.44570377933671779 ) ) ;
#35407 = AXIS2_PLACEMENT_3D ( 'NONE', #30708, #45160, #30470 ) ;
#35408 = CYLINDRICAL_SURFACE ( 'NONE', #9728, 42.00000000000000000 ) ;
#35409 = ORIENTED_EDGE ( 'NONE', *, *, #40511, .F. ) ;
#35410 = VERTEX_POINT ( 'NONE', #18155 ) ;
#35411 = EDGE_CURVE ( 'NONE', #12792, #7732, #34064, .T. ) ;
#35412 = VERTEX_POINT ( 'NONE', #44 ) ;
#35413 = DIRECTION ( 'NONE',  ( -1.000000000000000000, 0.000000000000000000, 0.000000000000000000 ) ) ;
#35415 = VERTEX_POINT ( 'NONE', #21839 ) ;
#35414 = DIRECTION ( 'NONE',  ( 0.000000000000000000, -0.5877852522924789103, 0.8090169943749432324 ) ) ;
#35416 = DIRECTION ( 'NONE',  ( -0.000000000000000000, 0.9945218953682744001, 0.1045284632676437842 ) ) ;
#35417 = ORIENTED_EDGE ( 'NONE', *, *, #29218, .T. ) ;
#35418 = ORIENTED_EDGE ( 'NONE', *, *, #41122, .F. ) ;
#35419 = CARTESIAN_POINT ( 'NONE',  ( 12.00000000000000000, 5.835314593368777558, 22.81335362449846471 ) ) ;
#35420 = ORIENTED_EDGE ( 'NONE', *, *, #29501, .T. ) ;
#35421 = EDGE_LOOP ( 'NONE', ( #34996, #12679, #30975, #10113 ) ) ;
#35422 = EDGE_CURVE ( 'NONE', #15212, #28487, #41193, .T. ) ;
#35423 = CARTESIAN_POINT ( 'NONE',  ( -1.029419772574582836, -121.0910063848724718, 2.500000000000000000 ) ) ;
#35424 = CARTESIAN_POINT ( 'NONE',  ( 10.00000000000000000, 0.6853352020790449695, 37.58145647212454321 ) ) ;
#35425 = ADVANCED_FACE ( 'NONE', ( #29913 ), #37010, .F. ) ;
#35426 = CARTESIAN_POINT ( 'NONE',  ( 11.99999999999999822, 0.000000000000000000, 0.000000000000000000 ) ) ;
#35427 = DIRECTION ( 'NONE',  ( -1.000000000000000000, -0.000000000000000000, -0.000000000000000000 ) ) ;
#35428 = AXIS2_PLACEMENT_3D ( 'NONE', #25454, #14210, #24505 ) ;
#35429 = CARTESIAN_POINT ( 'NONE',  ( 11.99999999999999822, 79.10210256391367523, 21.60688246758614284 ) ) ;
#35430 = ORIENTED_EDGE ( 'NONE', *, *, #21099, .T. ) ;
#35431 = ORIENTED_EDGE ( 'NONE', *, *, #24978, .T. ) ;
#35432 = CIRCLE ( 'NONE', #44833, 31.99999999999998579 ) ;
#35433 = LINE ( 'NONE', #1924, #31348 ) ;
#35434 = FACE_OUTER_BOUND ( 'NONE', #20487, .T. ) ;
#35435 = ORIENTED_EDGE ( 'NONE', *, *, #47916, .F. ) ;
#35436 = CARTESIAN_POINT ( 'NONE',  ( 0.000000000000000000, -76.41127070299262414, -12.93880638057396304 ) ) ;
#35437 = ORIENTED_EDGE ( 'NONE', *, *, #34719, .F. ) ;
#35438 = VECTOR ( 'NONE', #11662, 1000.000000000000000 ) ;
#35439 = VECTOR ( 'NONE', #25963, 1000.000000000000114 ) ;
#35440 = AXIS2_PLACEMENT_3D ( 'NONE', #8597, #37269, #3733 ) ;
#35441 = DIRECTION ( 'NONE',  ( 0.000000000000000000, 0.000000000000000000, 1.000000000000000000 ) ) ;
#35442 = AXIS2_PLACEMENT_3D ( 'NONE', #41050, #45668, #33674 ) ;
#35443 = DIRECTION ( 'NONE',  ( 0.000000000000000000, 0.000000000000000000, 1.000000000000000000 ) ) ;
#35444 = CARTESIAN_POINT ( 'NONE',  ( 11.99999999999999822, -74.18225833017913828, 34.94270380257611208 ) ) ;
#35445 = VERTEX_POINT ( 'NONE', #33349 ) ;
#35446 = CARTESIAN_POINT ( 'NONE',  ( 0.000000000000000000, -26.01480285779885904, 70.53064760720306481 ) ) ;
#35447 = CARTESIAN_POINT ( 'NONE',  ( 5.000000000000002665, 74.18225833017888249, 34.94270380257665209 ) ) ;
#35448 = DIRECTION ( 'NONE',  ( -1.000000000000000000, -0.000000000000000000, -0.000000000000000000 ) ) ;
#35449 = VERTEX_POINT ( 'NONE', #36766 ) ;
#35450 = VECTOR ( 'NONE', #3186, 1000.000000000000000 ) ;
#35451 = VECTOR ( 'NONE', #40280, 1000.000000000000227 ) ;
#35452 = CARTESIAN_POINT ( 'NONE',  ( -8.826826895187510402, -94.96827758698185562, 2.500000000000000000 ) ) ;
#35453 = CARTESIAN_POINT ( 'NONE',  ( -35.50000000000000711, -120.0000000000000000, 2.500000000000000000 ) ) ;
#35454 = CYLINDRICAL_SURFACE ( 'NONE', #27024, 16.00000000000000000 ) ;
#35455 = VECTOR ( 'NONE', #3961, 1000.000000000000000 ) ;
#35456 = VECTOR ( 'NONE', #1520, 1000.000000000000114 ) ;
#35457 = DIRECTION ( 'NONE',  ( -0.000000000000000000, -0.000000000000000000, -1.000000000000000000 ) ) ;
#35458 = VECTOR ( 'NONE', #11992, 1000.000000000000000 ) ;
#35459 = ORIENTED_EDGE ( 'NONE', *, *, #33230, .T. ) ;
#35460 = EDGE_CURVE ( 'NONE', #5074, #17824, #7408, .T. ) ;
#35461 = EDGE_CURVE ( 'NONE', #23089, #46110, #19369, .T. ) ;
#35462 = CARTESIAN_POINT ( 'NONE',  ( 0.000000000000000000, 0.000000000000000000, 0.000000000000000000 ) ) ;
#35463 = CYLINDRICAL_SURFACE ( 'NONE', #5844, 31.99999999999999289 ) ;
#35464 = EDGE_CURVE ( 'NONE', #40215, #11148, #14754, .T. ) ;
#35465 = VERTEX_POINT ( 'NONE', #40941 ) ;
#35466 = CYLINDRICAL_SURFACE ( 'NONE', #38210, 82.00000000000000000 ) ;
#35467 = VECTOR ( 'NONE', #46885, 1000.000000000000000 ) ;
#35468 = AXIS2_PLACEMENT_3D ( 'NONE', #18983, #4074, #22907 ) ;
#35470 = EDGE_LOOP ( 'NONE', ( #32182, #5031, #128, #45232 ) ) ;
#35469 = VECTOR ( 'NONE', #10165, 1000.000000000000000 ) ;
#35471 = ORIENTED_EDGE ( 'NONE', *, *, #40599, .F. ) ;
#35472 = EDGE_LOOP ( 'NONE', ( #15027, #40997, #46754, #35047 ) ) ;
#35473 = VERTEX_POINT ( 'NONE', #3729 ) ;
#35474 = PRODUCT_DEFINITION_SHAPE ( 'NONE', 'NONE',  #46888 ) ;
#35475 = EDGE_CURVE ( 'NONE', #41750, #2177, #24860, .T. ) ;
#35476 = EDGE_CURVE ( 'NONE', #34754, #28089, #30899, .T. ) ;
#35477 = ADVANCED_FACE ( 'NONE', ( #38728 ), #37992, .T. ) ;
#35478 = LINE ( 'NONE', #31100, #25096 ) ;
#35479 = ORIENTED_EDGE ( 'NONE', *, *, #43667, .T. ) ;
#35480 = CIRCLE ( 'NONE', #26125, 82.00000000000000000 ) ;
#35481 = VECTOR ( 'NONE', #33100, 1000.000000000000000 ) ;
#35482 = ORIENTED_EDGE ( 'NONE', *, *, #30195, .F. ) ;
#35483 = CARTESIAN_POINT ( 'NONE',  ( 10.00000000000000000, 35.53030884539102630, -12.26510123303222599 ) ) ;
#35484 = EDGE_LOOP ( 'NONE', ( #13696, #9938, #45993, #12441 ) ) ;
#35485 = CIRCLE ( 'NONE', #4233, 77.49900000000000944 ) ;
#35486 = FACE_OUTER_BOUND ( 'NONE', #9845, .T. ) ;
#35487 = AXIS2_PLACEMENT_3D ( 'NONE', #29860, #26681, #4642 ) ;
#35488 = VECTOR ( 'NONE', #35856, 1000.000000000000000 ) ;
#35489 = CYLINDRICAL_SURFACE ( 'NONE', #41866, 77.49899999999999523 ) ;
#35490 = DIRECTION ( 'NONE',  ( 0.000000000000000000, -0.8910065241883722287, 0.4539904997395383113 ) ) ;
#35492 = ORIENTED_EDGE ( 'NONE', *, *, #39582, .T. ) ;
#35491 = AXIS2_PLACEMENT_3D ( 'NONE', #38488, #4954, #35287 ) ;
#35493 = DIRECTION ( 'NONE',  ( -1.000000000000000000, -0.000000000000000000, -0.000000000000000000 ) ) ;
#35494 = EDGE_LOOP ( 'NONE', ( #36620, #24282, #12688, #19894 ) ) ;
#35495 = CARTESIAN_POINT ( 'NONE',  ( 10.00000000000000000, -33.80338159004296017, 16.23288003029484727 ) ) ;
#35496 = CARTESIAN_POINT ( 'NONE',  ( 10.00000000000000000, 35.53030884539084866, 12.26510123303271982 ) ) ;
#35497 = CARTESIAN_POINT ( 'NONE',  ( 11.99999999999999822, -77.49459641780886443, -0.8261519478439277586 ) ) ;
#35498 = ORIENTED_EDGE ( 'NONE', *, *, #2414, .F. ) ;
#35499 = EDGE_LOOP ( 'NONE', ( #42321, #30474, #29053, #20863 ) ) ;
#35500 = CARTESIAN_POINT ( 'NONE',  ( 89.17737905728634473, -39.70432723693593857, 5.500000000000000000 ) ) ;
#35501 = CYLINDRICAL_SURFACE ( 'NONE', #47272, 16.00000000000000000 ) ;
#35502 = ORIENTED_EDGE ( 'NONE', *, *, #9596, .T. ) ;
#35503 = DIRECTION ( 'NONE',  ( 0.000000000000000000, 0.000000000000000000, 1.000000000000000000 ) ) ;
#35504 = DIRECTION ( 'NONE',  ( 0.000000000000000000, -0.4067366430758010409, 0.9135454576426005335 ) ) ;
#35505 = CYLINDRICAL_SURFACE ( 'NONE', #38610, 82.00000000000000000 ) ;
#35506 = DIRECTION ( 'NONE',  ( -1.000000000000000000, 0.000000000000000000, -0.000000000000000000 ) ) ;
#35507 = DIRECTION ( 'NONE',  ( 0.000000000000000000, 0.6494480483301793283, 0.7604059656000345946 ) ) ;
#35508 = DIRECTION ( 'NONE',  ( 0.000000000000000000, 0.2079116908177543743, 0.9781476007338066880 ) ) ;
#35509 = VECTOR ( 'NONE', #47700, 1000.000000000000114 ) ;
#35510 = FACE_OUTER_BOUND ( 'NONE', #39334, .T. ) ;
#35511 = DIRECTION ( 'NONE',  ( -1.000000000000000000, 0.000000000000000000, 0.000000000000000000 ) ) ;
#35512 = CIRCLE ( 'NONE', #6576, 12.49999999999999645 ) ;
#35513 = AXIS2_PLACEMENT_3D ( 'NONE', #2767, #25266, #18425 ) ;
#35514 = DIRECTION ( 'NONE',  ( -1.000000000000000000, -0.000000000000000000, 0.000000000000000000 ) ) ;
#35516 = VECTOR ( 'NONE', #2252, 1000.000000000000000 ) ;
#35515 = DIRECTION ( 'NONE',  ( -1.000000000000000000, -0.000000000000000000, 0.000000000000000000 ) ) ;
#35517 = SURFACE_STYLE_FILL_AREA ( #27954 ) ;
#35518 = CARTESIAN_POINT ( 'NONE',  ( 10.00000000000000000, 21.53537804866081373, 30.80686688397018358 ) ) ;
#35519 = CARTESIAN_POINT ( 'NONE',  ( 11.99999999999999822, -30.41916302227164337, 71.27951684758015460 ) ) ;
#35520 = ORIENTED_EDGE ( 'NONE', *, *, #48116, .T. ) ;
#35521 = EDGE_CURVE ( 'NONE', #26069, #16291, #23296, .T. ) ;
#35522 = ORIENTED_EDGE ( 'NONE', *, *, #30008, .F. ) ;
#35523 = EDGE_CURVE ( 'NONE', #41773, #25899, #41917, .T. ) ;
#35525 = CYLINDRICAL_SURFACE ( 'NONE', #27654, 37.49900000000000233 ) ;
#35524 = CIRCLE ( 'NONE', #12090, 77.49899999999999523 ) ;
#35526 = AXIS2_PLACEMENT_3D ( 'NONE', #15105, #33221, #413 ) ;
#35527 = CYLINDRICAL_SURFACE ( 'NONE', #14289, 31.99999999999999289 ) ;
#35528 = AXIS2_PLACEMENT_3D ( 'NONE', #35217, #5137, #42824 ) ;
#35529 = EDGE_CURVE ( 'NONE', #21026, #13144, #29546, .T. ) ;
#35530 = ITEM_DEFINED_TRANSFORMATION ( 'NONE', 'NONE', #22534,  #11636 ) ;
#35531 = DIRECTION ( 'NONE',  ( 0.000000000000000000, 0.6494480483301849905, -0.7604059656000298206 ) ) ;
#35532 = EDGE_CURVE ( 'NONE', #44403, #37347, #23776, .T. ) ;
#35533 = AXIS2_PLACEMENT_3D ( 'NONE', #48378, #4561, #14856 ) ;
#35534 = EDGE_LOOP ( 'NONE', ( #16476, #9832, #21623, #1358 ) ) ;
#35535 = DIRECTION ( 'NONE',  ( 0.000000000000000000, 0.000000000000000000, -1.000000000000000000 ) ) ;
#35536 = ORIENTED_EDGE ( 'NONE', *, *, #7361, .T. ) ;
#35537 = DIRECTION ( 'NONE',  ( 0.000000000000000000, 0.000000000000000000, 1.000000000000000000 ) ) ;
#35538 = VERTEX_POINT ( 'NONE', #30643 ) ;
#35539 = CARTESIAN_POINT ( 'NONE',  ( -7.670864526094549163, -97.73662565058241114, 5.500000000000000000 ) ) ;
#35541 = EDGE_CURVE ( 'NONE', #19547, #22184, #31627, .T. ) ;
#35540 = MANIFOLD_SOLID_BREP ( 'InnerRace', #48144 ) ;
#35542 = ADVANCED_FACE ( 'NONE', ( #31385 ), #38963, .T. ) ;
#35543 = CIRCLE ( 'NONE', #14443, 77.49900000000000944 ) ;
#35544 = DIRECTION ( 'NONE',  ( 0.000000000000000000, 0.000000000000000000, -1.000000000000000000 ) ) ;
#35545 = CARTESIAN_POINT ( 'NONE',  ( -23.97194136764370498, -131.3950000906648938, -2.500000000000000444 ) ) ;
#35546 = ORIENTED_EDGE ( 'NONE', *, *, #13372, .T. ) ;
#35547 = AXIS2_PLACEMENT_3D ( 'NONE', #24122, #31477, #46882 ) ;
#35548 = LINE ( 'NONE', #12550, #19966 ) ;
#35549 = AXIS2_PLACEMENT_3D ( 'NONE', #44850, #15716, #38000 ) ;
#35550 = ORIENTED_EDGE ( 'NONE', *, *, #25502, .F. ) ;
#35551 = ORIENTED_EDGE ( 'NONE', *, *, #4104, .F. ) ;
#35552 = LINE ( 'NONE', #5447, #11865 ) ;
#35553 = LINE ( 'NONE', #24777, #35516 ) ;
#35554 = CARTESIAN_POINT ( 'NONE',  ( 0.000000000000000000, -59.03961581697432592, 46.53671651293927880 ) ) ;
#35555 = EDGE_CURVE ( 'NONE', #2082, #42556, #15474, .T. ) ;
#35557 = VERTEX_POINT ( 'NONE', #38467 ) ;
#35556 = DIRECTION ( 'NONE',  ( 0.000000000000000000, 0.000000000000000000, 1.000000000000000000 ) ) ;
#35558 = VECTOR ( 'NONE', #42950, 1000.000000000000000 ) ;
#35559 = ORIENTED_EDGE ( 'NONE', *, *, #47722, .T. ) ;
#35560 = DIRECTION ( 'NONE',  ( 0.000000000000000000, -0.8090169943749531134, 0.5877852522924653655 ) ) ;
#35561 = ORIENTED_EDGE ( 'NONE', *, *, #35778, .T. ) ;
#35562 = CIRCLE ( 'NONE', #14458, 16.00000000000000000 ) ;
#35563 = DIRECTION ( 'NONE',  ( -1.000000000000000000, 0.000000000000000000, 0.000000000000000000 ) ) ;
#35564 = CARTESIAN_POINT ( 'NONE',  ( 10.00000000000000000, -33.00180498840060039, 17.80606268964528027 ) ) ;
#35565 = AXIS2_PLACEMENT_3D ( 'NONE', #23281, #7860, #30393 ) ;
#35566 = LINE ( 'NONE', #35314, #41496 ) ;
#35567 = DIRECTION ( 'NONE',  ( 0.000000000000000000, -0.3090169943749349057, -0.9510565162951576390 ) ) ;
#35568 = ORIENTED_EDGE ( 'NONE', *, *, #9884, .F. ) ;
#35569 = DIRECTION ( 'NONE',  ( 0.7585478161175723821, 0.6516173805718057377, -0.000000000000000000 ) ) ;
#35570 = AXIS2_PLACEMENT_3D ( 'NONE', #35375, #8695, #12164 ) ;
#35571 = DIRECTION ( 'NONE',  ( 0.000000000000000000, 0.000000000000000000, 1.000000000000000000 ) ) ;
#35572 = AXIS2_PLACEMENT_3D ( 'NONE', #4898, #1241, #34031 ) ;
#35573 = DIRECTION ( 'NONE',  ( 0.000000000000000000, 0.000000000000000000, 1.000000000000000000 ) ) ;
#35574 = CYLINDRICAL_SURFACE ( 'NONE', #980, 31.99999999999998579 ) ;
#35575 = FACE_OUTER_BOUND ( 'NONE', #37609, .T. ) ;
#35576 = CARTESIAN_POINT ( 'NONE',  ( 10.00000000000000000, -74.74816331893404708, -33.71516098798818462 ) ) ;
#35577 = DIRECTION ( 'NONE',  ( 0.08130631524009970801, -0.9966891607226786576, 0.000000000000000000 ) ) ;
#35578 = DIRECTION ( 'NONE',  ( -1.000000000000000000, -0.000000000000000000, 0.000000000000000000 ) ) ;
#35579 = CYLINDRICAL_SURFACE ( 'NONE', #8794, 12.50000000000000000 ) ;
#35580 = CARTESIAN_POINT ( 'NONE',  ( 15.00000000000000000, 0.000000000000000000, 0.000000000000000000 ) ) ;
#35581 = ORIENTED_EDGE ( 'NONE', *, *, #9828, .F. ) ;
#35582 = ORIENTED_EDGE ( 'NONE', *, *, #13970, .T. ) ;
#35583 = AXIS2_PLACEMENT_3D ( 'NONE', #21107, #31437, #43638 ) ;
#35584 = FACE_OUTER_BOUND ( 'NONE', #44099, .T. ) ;
#35585 = ORIENTED_EDGE ( 'NONE', *, *, #34252, .F. ) ;
#35586 = DIRECTION ( 'NONE',  ( 0.000000000000000000, 0.9510565162951523099, 0.3090169943749516146 ) ) ;
#35587 = AXIS2_PLACEMENT_3D ( 'NONE', #16248, #11374, #22609 ) ;
#35588 = EDGE_CURVE ( 'NONE', #39158, #2161, #8122, .T. ) ;
#35589 = CYLINDRICAL_SURFACE ( 'NONE', #3331, 82.00000000000000000 ) ;
#35590 = EDGE_CURVE ( 'NONE', #18992, #25663, #45205, .T. ) ;
#35591 = ORIENTED_EDGE ( 'NONE', *, *, #26269, .F. ) ;
#35592 = CIRCLE ( 'NONE', #36355, 31.99999999999998934 ) ;
#35593 = VECTOR ( 'NONE', #14048, 1000.000000000000000 ) ;
#35594 = EDGE_CURVE ( 'NONE', #19983, #42640, #4568, .T. ) ;
#35595 = CARTESIAN_POINT ( 'NONE',  ( 10.00000000000000000, 0.000000000000000000, 0.000000000000000000 ) ) ;
#35596 = CIRCLE ( 'NONE', #12933, 42.00000000000000000 ) ;
#35597 = ORIENTED_EDGE ( 'NONE', *, *, #3557, .T. ) ;
#35598 = VERTEX_POINT ( 'NONE', #38231 ) ;
#35599 = AXIS2_PLACEMENT_3D ( 'NONE', #42730, #38090, #12386 ) ;
#35600 = AXIS2_PLACEMENT_3D ( 'NONE', #34266, #23023, #26700 ) ;
#35601 = EDGE_CURVE ( 'NONE', #17031, #14290, #19599, .T. ) ;
#35602 = LINE ( 'NONE', #39030, #8091 ) ;
#35603 = EDGE_CURVE ( 'NONE', #13811, #17121, #39689, .T. ) ;
#35604 = CARTESIAN_POINT ( 'NONE',  ( 0.000000000000000000, 14.60985201121729737, -18.46759930825688301 ) ) ;
#35605 = CARTESIAN_POINT ( 'NONE',  ( 11.99999999999999822, 29.01471420065563933, 76.69515212746024702 ) ) ;
#35606 = ORIENTED_EDGE ( 'NONE', *, *, #33436, .F. ) ;
#35607 = DIRECTION ( 'NONE',  ( -1.000000000000000000, -0.000000000000000000, -0.000000000000000000 ) ) ;
#35608 = CIRCLE ( 'NONE', #24678, 77.49900000000000944 ) ;
#35609 = ORIENTED_EDGE ( 'NONE', *, *, #39937, .T. ) ;
#35610 = ORIENTED_EDGE ( 'NONE', *, *, #45996, .F. ) ;
#35611 = DIRECTION ( 'NONE',  ( -1.000000000000000000, -0.000000000000000000, -0.000000000000000000 ) ) ;
#35612 = LINE ( 'NONE', #34622, #3560 ) ;
#35613 = DIRECTION ( 'NONE',  ( -1.000000000000000000, -0.000000000000000000, -0.000000000000000000 ) ) ;
#35614 = EDGE_CURVE ( 'NONE', #19505, #19471, #17627, .T. ) ;
#35615 = ORIENTED_EDGE ( 'NONE', *, *, #9770, .F. ) ;
#35616 = ORIENTED_EDGE ( 'NONE', *, *, #6147, .T. ) ;
#35617 = EDGE_LOOP ( 'NONE', ( #6151, #37961, #34729, #27379 ) ) ;
#35618 = DIRECTION ( 'NONE',  ( 0.000000000000000000, 0.000000000000000000, 1.000000000000000000 ) ) ;
#35619 = ORIENTED_EDGE ( 'NONE', *, *, #25172, .F. ) ;
#35620 = FACE_BOUND ( 'NONE', #18318, .T. ) ;
#35621 = DIRECTION ( 'NONE',  ( 1.000000000000000000, 0.000000000000000000, -0.000000000000000000 ) ) ;
#35622 = FACE_OUTER_BOUND ( 'NONE', #44676, .T. ) ;
#35623 = CARTESIAN_POINT ( 'NONE',  ( 0.000000000000000000, 2.956366410620650420, 75.11725578898469280 ) ) ;
#35624 = DIRECTION ( 'NONE',  ( 0.000000000000000000, 0.000000000000000000, 1.000000000000000000 ) ) ;
#35625 = CARTESIAN_POINT ( 'NONE',  ( 11.99999999999999822, 58.39081064771822582, -50.95692526931267707 ) ) ;
#35626 = MANIFOLD_SOLID_BREP ( 'Cut-Extrude1', #22360 ) ;
#35627 = CARTESIAN_POINT ( 'NONE',  ( 0.000000000000000000, 0.000000000000000000, 0.000000000000000000 ) ) ;
#35628 = CARTESIAN_POINT ( 'NONE',  ( 0.000000000000000000, 0.000000000000000000, 0.000000000000000000 ) ) ;
#35629 = LINE ( 'NONE', #2102, #11093 ) ;
#35630 = FACE_OUTER_BOUND ( 'NONE', #8576, .T. ) ;
#35631 = AXIS2_PLACEMENT_3D ( 'NONE', #17115, #28851, #13453 ) ;
#35632 = ORIENTED_EDGE ( 'NONE', *, *, #4706, .F. ) ;
#35633 = DIRECTION ( 'NONE',  ( 0.000000000000000000, -0.9781476007338070211, 0.2079116908177525425 ) ) ;
#35634 = VECTOR ( 'NONE', #42978, 1000.000000000000000 ) ;
#35635 = PLANE ( 'NONE',  #15041 ) ;
#35636 = DIRECTION ( 'NONE',  ( -1.000000000000000000, -0.000000000000000000, 0.000000000000000000 ) ) ;
#35637 = CIRCLE ( 'NONE', #12198, 16.00000000000000000 ) ;
#35638 = DIRECTION ( 'NONE',  ( 0.000000000000000000, 0.000000000000000000, 1.000000000000000000 ) ) ;
#35639 = LINE ( 'NONE', #17027, #38920 ) ;
#35640 = LINE ( 'NONE', #5536, #19316 ) ;
#35641 = CARTESIAN_POINT ( 'NONE',  ( -3.000000000000000000, 23.59884966291538078, -12.14883922797231541 ) ) ;
#35642 = AXIS2_PLACEMENT_3D ( 'NONE', #18482, #4523, #15307 ) ;
#35643 = VERTEX_POINT ( 'NONE', #24968 ) ;
#35644 = EDGE_CURVE ( 'NONE', #41084, #23915, #47489, .T. ) ;
#35645 = DIRECTION ( 'NONE',  ( -1.000000000000000000, -0.000000000000000000, -0.000000000000000000 ) ) ;
#35646 = EDGE_CURVE ( 'NONE', #5501, #31423, #47015, .T. ) ;
#35647 = EDGE_LOOP ( 'NONE', ( #3362, #36980 ) ) ;
#35648 = CIRCLE ( 'NONE', #20795, 82.00000000000000000 ) ;
#35649 = CARTESIAN_POINT ( 'NONE',  ( -10.00000000000000000, 0.000000000000000000, 0.000000000000000000 ) ) ;
#35650 = VERTEX_POINT ( 'NONE', #28405 ) ;
#35651 = EDGE_CURVE ( 'NONE', #25478, #7237, #31872, .T. ) ;
#35652 = ORIENTED_EDGE ( 'NONE', *, *, #29619, .F. ) ;
#35653 = ORIENTED_EDGE ( 'NONE', *, *, #10550, .F. ) ;
#35654 = AXIS2_PLACEMENT_3D ( 'NONE', #539, #26247, #11562 ) ;
#35655 = EDGE_CURVE ( 'NONE', #2889, #4582, #20982, .T. ) ;
#35656 = EDGE_CURVE ( 'NONE', #14155, #19851, #29572, .T. ) ;
#35657 = CARTESIAN_POINT ( 'NONE',  ( -10.00000000000000000, 0.000000000000000000, 0.000000000000000000 ) ) ;
#35658 = PRESENTATION_LAYER_ASSIGNMENT (  '', '', ( #9872 ) ) ;
#35659 = ORIENTED_EDGE ( 'NONE', *, *, #8499, .F. ) ;
#35660 = VERTEX_POINT ( 'NONE', #28659 ) ;
#35661 = AXIS2_PLACEMENT_3D ( 'NONE', #25416, #10747, #10979 ) ;
#35662 = DIRECTION ( 'NONE',  ( -1.000000000000000000, -0.000000000000000000, -0.000000000000000000 ) ) ;
#35663 = DIRECTION ( 'NONE',  ( 0.000000000000000000, -0.4067366430757899942, 0.9135454576426055295 ) ) ;
#35664 = EDGE_LOOP ( 'NONE', ( #41950, #32826, #38851, #29136 ) ) ;
#35665 = CIRCLE ( 'NONE', #23152, 15.99999999999999822 ) ;
#35666 = ORIENTED_EDGE ( 'NONE', *, *, #26877, .F. ) ;
#35667 = ORIENTED_EDGE ( 'NONE', *, *, #15197, .F. ) ;
#35668 = CARTESIAN_POINT ( 'NONE',  ( 10.00000000000000000, 0.000000000000000000, 0.000000000000000000 ) ) ;
#35670 = VERTEX_POINT ( 'NONE', #32328 ) ;
#35669 = CYLINDRICAL_SURFACE ( 'NONE', #46201, 82.00000000000000000 ) ;
#35671 = EDGE_CURVE ( 'NONE', #2158, #42271, #24253, .T. ) ;
#35672 = DIRECTION ( 'NONE',  ( -1.000000000000000000, -0.000000000000000000, -0.000000000000000000 ) ) ;
#35673 = VERTEX_POINT ( 'NONE', #39193 ) ;
#35674 = VERTEX_POINT ( 'NONE', #13246 ) ;
#35675 = CARTESIAN_POINT ( 'NONE',  ( 11.99999999999999822, 59.03961581697399907, 46.53671651293969802 ) ) ;
#35676 = EDGE_LOOP ( 'NONE', ( #11110, #47982, #32500, #27355 ) ) ;
#35677 = DIRECTION ( 'NONE',  ( 0.000000000000000000, 0.5224985647159440250, 0.8526401643540951758 ) ) ;
#35678 = CYLINDRICAL_SURFACE ( 'NONE', #13955, 32.50000000000000000 ) ;
#35679 = AXIS2_PLACEMENT_3D ( 'NONE', #27093, #8706, #5055 ) ;
#35680 = FACE_OUTER_BOUND ( 'NONE', #41348, .T. ) ;
#35681 = DIRECTION ( 'NONE',  ( 0.000000000000000000, 0.000000000000000000, -1.000000000000000000 ) ) ;
#35682 = CARTESIAN_POINT ( 'NONE',  ( -18.24502636017238899, -100.7225776329765665, -5.500000000000000000 ) ) ;
#35683 = EDGE_CURVE ( 'NONE', #4413, #913, #20575, .T. ) ;
#35684 = AXIS2_PLACEMENT_3D ( 'NONE', #47291, #13768, #2729 ) ;
#35685 = ORIENTED_EDGE ( 'NONE', *, *, #16813, .F. ) ;
#35686 = ORIENTED_EDGE ( 'NONE', *, *, #25728, .F. ) ;
#35687 = LINE ( 'NONE', #42552, #51 ) ;
#35688 = AXIS2_PLACEMENT_3D ( 'NONE', #23766, #6137, #1998 ) ;
#35689 = FACE_OUTER_BOUND ( 'NONE', #20077, .T. ) ;
#35690 = ORIENTED_EDGE ( 'NONE', *, *, #45630, .F. ) ;
#35691 = DIRECTION ( 'NONE',  ( -1.000000000000000000, 0.000000000000000000, 0.000000000000000000 ) ) ;
#35692 = EDGE_LOOP ( 'NONE', ( #35430, #20791, #45102, #16073 ) ) ;
#35693 = CARTESIAN_POINT ( 'NONE',  ( 0.000000000000000000, 0.000000000000000000, 40.00000000000000000 ) ) ;
#35694 = FACE_OUTER_BOUND ( 'NONE', #25707, .T. ) ;
#35695 = CARTESIAN_POINT ( 'NONE',  ( -18.12185313557660038, -104.9634299478706794, 5.500000000000000000 ) ) ;
#35696 = EDGE_LOOP ( 'NONE', ( #25283, #31286, #7049, #26866 ) ) ;
#35697 = CARTESIAN_POINT ( 'NONE',  ( 0.000000000000000000, -16.45098606841149902, 33.79645857604508308 ) ) ;
#35698 = CARTESIAN_POINT ( 'NONE',  ( -16.07206065793331007, -141.0698568150738197, 2.500000000000000000 ) ) ;
#35699 = CARTESIAN_POINT ( 'NONE',  ( 15.00000000000000000, 26.49999999999999645, 1.499999999999995781 ) ) ;
#35700 = ORIENTED_EDGE ( 'NONE', *, *, #41549, .T. ) ;
#35701 = DIRECTION ( 'NONE',  ( -1.000000000000000000, 0.000000000000000000, -0.000000000000000000 ) ) ;
#35702 = CARTESIAN_POINT ( 'NONE',  ( 0.000000000000000000, -120.0000000000000000, -2.500000000000000000 ) ) ;
#35703 = DIRECTION ( 'NONE',  ( -1.000000000000000000, 0.000000000000000000, -0.000000000000000000 ) ) ;
#35704 = EDGE_CURVE ( 'NONE', #30959, #22184, #28168, .T. ) ;
#35705 = AXIS2_PLACEMENT_3D ( 'NONE', #16426, #5181, #12043 ) ;
#35706 = CARTESIAN_POINT ( 'NONE',  ( 10.00000000000000000, 0.000000000000000000, 0.000000000000000000 ) ) ;
#35707 = ADVANCED_FACE ( 'NONE', ( #9003 ), #16351, .T. ) ;
#35708 = ORIENTED_EDGE ( 'NONE', *, *, #38177, .T. ) ;
#35709 = ORIENTED_EDGE ( 'NONE', *, *, #18290, .T. ) ;
#35710 = CIRCLE ( 'NONE', #47409, 42.00000000000000000 ) ;
#35711 = EDGE_CURVE ( 'NONE', #6288, #5501, #27368, .T. ) ;
#35712 = CARTESIAN_POINT ( 'NONE',  ( 10.00000000000000000, -33.79645857604525361, 16.45098606841114730 ) ) ;
#35713 = CIRCLE ( 'NONE', #2864, 82.00000000000000000 ) ;
#35714 = CARTESIAN_POINT ( 'NONE',  ( 0.000000000000000000, 0.000000000000000000, 0.000000000000000000 ) ) ;
#35715 = VERTEX_POINT ( 'NONE', #46456 ) ;
#35716 = CIRCLE ( 'NONE', #34133, 16.00000000000000355 ) ;
#35717 = DIRECTION ( 'NONE',  ( -1.000000000000000000, -0.000000000000000000, -0.000000000000000000 ) ) ;
#35718 = VERTEX_POINT ( 'NONE', #46703 ) ;
#35719 = ORIENTED_EDGE ( 'NONE', *, *, #48028, .F. ) ;
#35720 = VERTEX_POINT ( 'NONE', #16124 ) ;
#35721 = CIRCLE ( 'NONE', #41989, 82.00000000000000000 ) ;
#35722 = CARTESIAN_POINT ( 'NONE',  ( 11.99999999999999822, 0.000000000000000000, 0.000000000000000000 ) ) ;
#35723 = ORIENTED_EDGE ( 'NONE', *, *, #45776, .F. ) ;
#35724 = ORIENTED_EDGE ( 'NONE', *, *, #38407, .T. ) ;
#35725 = CARTESIAN_POINT ( 'NONE',  ( -11.68233973192911535, 0.000000000000000000, 0.000000000000000000 ) ) ;
#35726 = ORIENTED_EDGE ( 'NONE', *, *, #15487, .F. ) ;
#35727 = DIRECTION ( 'NONE',  ( -1.000000000000000000, 0.000000000000000000, 0.000000000000000000 ) ) ;
#35728 = AXIS2_PLACEMENT_3D ( 'NONE', #19529, #46482, #1687 ) ;
#35729 = DIRECTION ( 'NONE',  ( -1.000000000000000000, -0.000000000000000000, -0.000000000000000000 ) ) ;
#35730 = CARTESIAN_POINT ( 'NONE',  ( 25.81725066941077529, -113.8380548628854854, -5.500000000000000000 ) ) ;
#35731 = EDGE_LOOP ( 'NONE', ( #46322, #2344, #31631, #21789 ) ) ;
#35732 = LINE ( 'NONE', #13937, #28243 ) ;
#35733 = ORIENTED_EDGE ( 'NONE', *, *, #8783, .T. ) ;
#35734 = FACE_OUTER_BOUND ( 'NONE', #9730, .T. ) ;
#35735 = CYLINDRICAL_SURFACE ( 'NONE', #5584, 31.99999999999998579 ) ;
#35736 = CIRCLE ( 'NONE', #14646, 31.99999999999998934 ) ;
#35737 = CARTESIAN_POINT ( 'NONE',  ( 10.00000000000000000, 21.40280677340421533, -36.13751322684397138 ) ) ;
#35738 = ORIENTED_EDGE ( 'NONE', *, *, #29606, .F. ) ;
#35739 = VERTEX_POINT ( 'NONE', #45732 ) ;
#35740 = DIRECTION ( 'NONE',  ( 0.000000000000000000, -0.8090169943749504489, -0.5877852522924689183 ) ) ;
#35741 = DIRECTION ( 'NONE',  ( -1.000000000000000000, 0.000000000000000000, -0.000000000000000000 ) ) ;
#35742 = ORIENTED_EDGE ( 'NONE', *, *, #25757, .F. ) ;
#35743 = ORIENTED_EDGE ( 'NONE', *, *, #19943, .T. ) ;
#35744 = ADVANCED_FACE ( 'NONE', ( #8750 ), #12209, .T. ) ;
#35745 = DIRECTION ( 'NONE',  ( 0.000000000000000000, 0.000000000000000000, 1.000000000000000000 ) ) ;
#35746 = DIRECTION ( 'NONE',  ( 0.000000000000000000, 0.000000000000000000, 1.000000000000000000 ) ) ;
#35747 = DIRECTION ( 'NONE',  ( 0.000000000000000000, 0.000000000000000000, 1.000000000000000000 ) ) ;
#35748 = DIRECTION ( 'NONE',  ( 0.000000000000000000, 0.9510565162951521989, 0.3090169943749515591 ) ) ;
#35749 = VECTOR ( 'NONE', #26551, 1000.000000000000000 ) ;
#35750 = CARTESIAN_POINT ( 'NONE',  ( 11.99999999999999822, 74.65374052328660071, -8.840884882374309583 ) ) ;
#35751 = ORIENTED_EDGE ( 'NONE', *, *, #1830, .F. ) ;
#35752 = DIRECTION ( 'NONE',  ( 0.000000000000000000, 0.000000000000000000, 1.000000000000000000 ) ) ;
#35753 = CARTESIAN_POINT ( 'NONE',  ( 12.69589495141918611, -96.69089767102708777, 5.500000000000000000 ) ) ;
#35754 = DIRECTION ( 'NONE',  ( -1.000000000000000000, -0.000000000000000000, 0.000000000000000000 ) ) ;
#35755 = DIRECTION ( 'NONE',  ( 0.000000000000000000, 0.000000000000000000, 1.000000000000000000 ) ) ;
#35756 = EDGE_CURVE ( 'NONE', #47844, #34450, #15501, .T. ) ;
#35757 = CARTESIAN_POINT ( 'NONE',  ( 0.000000000000000000, -12.42422080174614862, -35.38097989696524337 ) ) ;
#35758 = DIRECTION ( 'NONE',  ( -1.000000000000000000, -0.000000000000000000, 0.000000000000000000 ) ) ;
#35759 = EDGE_CURVE ( 'NONE', #33903, #21863, #2979, .T. ) ;
#35760 = ORIENTED_EDGE ( 'NONE', *, *, #6812, .T. ) ;
#35761 = ADVANCED_FACE ( 'NONE', ( #23440 ), #42059, .T. ) ;
#35762 = ORIENTED_EDGE ( 'NONE', *, *, #15039, .F. ) ;
#35763 = VECTOR ( 'NONE', #40665, 1000.000000000000000 ) ;
#35764 = DIRECTION ( 'NONE',  ( 1.000000000000000000, 0.000000000000000000, 0.000000000000000000 ) ) ;
#35765 = DIRECTION ( 'NONE',  ( 0.000000000000000000, -0.9876883405951394357, 0.1564344650402205716 ) ) ;
#35766 = ADVANCED_FACE ( 'NONE', ( #27607 ), #38142, .T. ) ;
#35767 = CIRCLE ( 'NONE', #14666, 16.00000000000000355 ) ;
#35768 = EDGE_CURVE ( 'NONE', #33272, #28804, #22559, .T. ) ;
#35769 = CARTESIAN_POINT ( 'NONE',  ( 0.000000000000000000, -73.44644590900077219, 24.73286445877675632 ) ) ;
#35770 = VERTEX_POINT ( 'NONE', #19753 ) ;
#35771 = ORIENTED_EDGE ( 'NONE', *, *, #24458, .T. ) ;
#35772 = AXIS2_PLACEMENT_3D ( 'NONE', #3971, #37734, #29664 ) ;
#35773 = DIRECTION ( 'NONE',  ( 0.000000000000000000, 0.000000000000000000, 1.000000000000000000 ) ) ;
#35774 = ORIENTED_EDGE ( 'NONE', *, *, #39302, .F. ) ;
#35775 = DIRECTION ( 'NONE',  ( 0.000000000000000000, -0.5000000000000028866, -0.8660254037844369313 ) ) ;
#35776 = ORIENTED_EDGE ( 'NONE', *, *, #14034, .T. ) ;
#35777 = DIRECTION ( 'NONE',  ( -1.000000000000000000, 0.000000000000000000, 0.000000000000000000 ) ) ;
#35778 = EDGE_CURVE ( 'NONE', #17554, #15896, #35179, .T. ) ;
#35779 = AXIS2_PLACEMENT_3D ( 'NONE', #16021, #8426, #20578 ) ;
#35780 = CARTESIAN_POINT ( 'NONE',  ( 11.99999999999999822, 11.30684508768450769, -76.66974797899825944 ) ) ;
#35781 = CARTESIAN_POINT ( 'NONE',  ( -25.50183398199384754, -112.6408924756582053, -5.500000000000000000 ) ) ;
#35782 = VERTEX_POINT ( 'NONE', #31056 ) ;
#35784 = ORIENTED_EDGE ( 'NONE', *, *, #37128, .T. ) ;
#35783 = CARTESIAN_POINT ( 'NONE',  ( 10.00000000000000000, 36.72794159290241822, 65.59268652807223532 ) ) ;
#35785 = ORIENTED_EDGE ( 'NONE', *, *, #10893, .T. ) ;
#35786 = DIRECTION ( 'NONE',  ( -1.000000000000000000, 0.000000000000000000, 0.000000000000000000 ) ) ;
#35787 = DIRECTION ( 'NONE',  ( -1.000000000000000000, -0.000000000000000000, 0.000000000000000000 ) ) ;
#35788 = DIRECTION ( 'NONE',  ( -1.000000000000000000, -0.000000000000000000, -0.000000000000000000 ) ) ;
#35790 = CARTESIAN_POINT ( 'NONE',  ( 11.99999999999999822, 59.03961581697465277, -46.53671651293886669 ) ) ;
#35789 = AXIS2_PLACEMENT_3D ( 'NONE', #26354, #29538, #18266 ) ;
#35791 = EDGE_CURVE ( 'NONE', #20853, #43486, #45975, .T. ) ;
#35792 = CARTESIAN_POINT ( 'NONE',  ( -7.670864526094549163, -97.73662565058241114, -5.500000000000000000 ) ) ;
#35793 = VERTEX_POINT ( 'NONE', #31292 ) ;
#35794 = CYLINDRICAL_SURFACE ( 'NONE', #2943, 82.00000000000000000 ) ;
#35795 = ORIENTED_EDGE ( 'NONE', *, *, #27612, .F. ) ;
#35796 = LINE ( 'NONE', #39487, #39566 ) ;
#35797 = ORIENTED_EDGE ( 'NONE', *, *, #38053, .T. ) ;
#35798 = EDGE_CURVE ( 'NONE', #13193, #19386, #10820, .T. ) ;
#35799 = COLOUR_RGB ( '', 0.40784314, 0.44705882, 0.49803922) ;
#35800 = CARTESIAN_POINT ( 'NONE',  ( 10.00000000000000000, 8.840884882376133902, -74.65374052328640175 ) ) ;
#35801 = CARTESIAN_POINT ( 'NONE',  ( 10.00000000000000000, 2.543863470249530856, -81.96053171279901051 ) ) ;
#35802 = DIRECTION ( 'NONE',  ( -1.000000000000000000, 0.000000000000000000, 0.000000000000000000 ) ) ;
#35803 = ORIENTED_EDGE ( 'NONE', *, *, #41648, .F. ) ;
#35804 = CARTESIAN_POINT ( 'NONE',  ( -0.9774260708577104939, -118.8621782758236378, 2.500000000000000000 ) ) ;
#35805 = CIRCLE ( 'NONE', #12367, 82.00000000000000000 ) ;
#35806 = ADVANCED_FACE ( 'NONE', ( #13161 ), #46210, .F. ) ;
#35807 = CARTESIAN_POINT ( 'NONE',  ( 10.00000000000000000, 10.74501242461282757, 35.92658777277515014 ) ) ;
#35808 = CARTESIAN_POINT ( 'NONE',  ( 11.99999999999999822, -58.39081064771786345, 50.95692526931308919 ) ) ;
#35809 = CYLINDRICAL_SURFACE ( 'NONE', #26005, 31.99999999999998579 ) ;
#35810 = FACE_BOUND ( 'NONE', #41083, .T. ) ;
#35811 = ORIENTED_EDGE ( 'NONE', *, *, #6626, .F. ) ;
#35812 = DIRECTION ( 'NONE',  ( -0.9435911131814395114, 0.3311129884571304971, 0.000000000000000000 ) ) ;
#35813 =( NAMED_UNIT ( * ) SI_UNIT ( $, .STERADIAN. ) SOLID_ANGLE_UNIT ( ) );
#35814 = DIRECTION ( 'NONE',  ( -1.000000000000000000, 0.000000000000000000, 0.000000000000000000 ) ) ;
#35815 = DIRECTION ( 'NONE',  ( -1.000000000000000000, 0.000000000000000000, 0.000000000000000000 ) ) ;
#35816 = LINE ( 'NONE', #13796, #43193 ) ;
#35817 = CARTESIAN_POINT ( 'NONE',  ( 26.09152095774781799, -124.8716048804687375, 5.500000000000000000 ) ) ;
#35818 = PRODUCT_DEFINITION_FORMATION_WITH_SPECIFIED_SOURCE ( 'ANY', '', #13210, .NOT_KNOWN. ) ;
#35819 = EDGE_CURVE ( 'NONE', #22174, #35557, #7703, .T. ) ;
#35820 = EDGE_CURVE ( 'NONE', #1310, #45334, #28093, .T. ) ;
#35821 = CIRCLE ( 'NONE', #31932, 16.00000000000000000 ) ;
#35822 = ORIENTED_EDGE ( 'NONE', *, *, #2062, .F. ) ;
#35823 = DIRECTION ( 'NONE',  ( -1.000000000000000000, 0.000000000000000000, 0.000000000000000000 ) ) ;
#35824 = ORIENTED_EDGE ( 'NONE', *, *, #4572, .F. ) ;
#35825 = CARTESIAN_POINT ( 'NONE',  ( -3.000000000000000000, 18.84667830672579925, 18.68964196561269020 ) ) ;
#35826 = DIRECTION ( 'NONE',  ( -1.000000000000000000, -0.000000000000000000, 0.000000000000000000 ) ) ;
#35827 = ORIENTED_EDGE ( 'NONE', *, *, #6394, .T. ) ;
#35828 = EDGE_CURVE ( 'NONE', #2924, #39337, #35056, .T. ) ;
#35829 = CARTESIAN_POINT ( 'NONE',  ( 10.00000000000000000, 36.13751322684419165, 21.40280677340384230 ) ) ;
#35830 = AXIS2_PLACEMENT_3D ( 'NONE', #34299, #4693, #767 ) ;
#35831 = VERTEX_POINT ( 'NONE', #15866 ) ;
#35832 = AXIS2_PLACEMENT_3D ( 'NONE', #6235, #48066, #17229 ) ;
#35833 = ORIENTED_EDGE ( 'NONE', *, *, #6149, .T. ) ;
#35834 = DIRECTION ( 'NONE',  ( -1.000000000000000000, -0.000000000000000000, -0.000000000000000000 ) ) ;
#35835 = VERTEX_POINT ( 'NONE', #14121 ) ;
#35836 = CARTESIAN_POINT ( 'NONE',  ( -20.30386590532152979, -102.9045904027214959, 5.500000000000000000 ) ) ;
#35837 = CARTESIAN_POINT ( 'NONE',  ( -7.670864526094549163, -97.73662565058241114, 2.500000000000000000 ) ) ;
#35838 = ORIENTED_EDGE ( 'NONE', *, *, #14700, .F. ) ;
#35839 = CARTESIAN_POINT ( 'NONE',  ( 10.00000000000000000, -27.05870788708250885, 26.08949754953014022 ) ) ;
#35840 = ORIENTED_EDGE ( 'NONE', *, *, #22524, .F. ) ;
#35841 = CYLINDRICAL_SURFACE ( 'NONE', #10826, 77.49899999999999523 ) ;
#35842 = CARTESIAN_POINT ( 'NONE',  ( 10.00000000000000000, -41.91543099594816368, -2.663952781846588014 ) ) ;
#35843 = DIRECTION ( 'NONE',  ( -1.000000000000000000, -0.000000000000000000, -0.000000000000000000 ) ) ;
#35844 = AXIS2_PLACEMENT_3D ( 'NONE', #37994, #27460, #19139 ) ;
#35845 = ADVANCED_FACE ( 'NONE', ( #43261 ), #46934, .T. ) ;
#35846 = EDGE_LOOP ( 'NONE', ( #19676, #7141, #23553, #34928 ) ) ;
#35847 = DIRECTION ( 'NONE',  ( 0.000000000000000000, 0.8910065241883657894, 0.4539904997395509678 ) ) ;
#35848 = EDGE_LOOP ( 'NONE', ( #46927, #21818, #5503, #20735 ) ) ;
#35849 = FACE_BOUND ( 'NONE', #5733, .T. ) ;
#35850 = ADVANCED_FACE ( 'NONE', ( #13887 ), #18016, .T. ) ;
#35851 = CARTESIAN_POINT ( 'NONE',  ( 0.000000000000000000, -22.32062822937469804, -14.36278369418829826 ) ) ;
#35852 = DIRECTION ( 'NONE',  ( 0.000000000000000000, 0.000000000000000000, 1.000000000000000000 ) ) ;
#35853 = CARTESIAN_POINT ( 'NONE',  ( 0.000000000000000000, 0.000000000000000000, 0.000000000000000000 ) ) ;
#35854 = DIRECTION ( 'NONE',  ( -1.000000000000000000, 0.000000000000000000, -0.000000000000000000 ) ) ;
#35855 = EDGE_CURVE ( 'NONE', #41683, #352, #13162, .T. ) ;
#35856 = DIRECTION ( 'NONE',  ( -1.000000000000000000, 0.000000000000000000, -0.000000000000000000 ) ) ;
#35857 = DIRECTION ( 'NONE',  ( 0.000000000000000000, 0.000000000000000000, 1.000000000000000000 ) ) ;
#35858 = DIRECTION ( 'NONE',  ( -0.9227826878668540234, -0.3853207896976546531, 0.000000000000000000 ) ) ;
#35859 = LINE ( 'NONE', #36101, #34550 ) ;
#35860 = DIRECTION ( 'NONE',  ( 0.000000000000000000, 0.8090169943749445647, 0.5877852522924770229 ) ) ;
#35861 = ORIENTED_EDGE ( 'NONE', *, *, #27008, .F. ) ;
#35862 = AXIS2_PLACEMENT_3D ( 'NONE', #48229, #40886, #36954 ) ;
#35863 = CYLINDRICAL_SURFACE ( 'NONE', #30186, 31.99999999999998579 ) ;
#35864 = CIRCLE ( 'NONE', #24134, 31.99999999999998579 ) ;
#35865 = VECTOR ( 'NONE', #34398, 1000.000000000000114 ) ;
#35866 = DIRECTION ( 'NONE',  ( 0.000000000000000000, -0.000000000000000000, 1.000000000000000000 ) ) ;
#35867 = DIRECTION ( 'NONE',  ( -0.2306669878475648139, -0.9730327541852491491, 0.000000000000000000 ) ) ;
#35868 = EDGE_CURVE ( 'NONE', #45324, #15496, #19394, .T. ) ;
#35869 = ADVANCED_FACE ( 'NONE', ( #24662 ), #39609, .T. ) ;
#35870 = FACE_OUTER_BOUND ( 'NONE', #266, .T. ) ;
#35871 = VERTEX_POINT ( 'NONE', #32712 ) ;
#35872 = CARTESIAN_POINT ( 'NONE',  ( 0.000000000000000000, -0.8299999999999999600, 0.000000000000000000 ) ) ;
#35873 = LINE ( 'NONE', #43222, #38637 ) ;
#35874 = EDGE_CURVE ( 'NONE', #33652, #29574, #36145, .T. ) ;
#35875 = EDGE_LOOP ( 'NONE', ( #25853, #22231, #35615, #44984 ) ) ;
#35876 = DIRECTION ( 'NONE',  ( -1.000000000000000000, -0.000000000000000000, -0.000000000000000000 ) ) ;
#35877 = VERTEX_POINT ( 'NONE', #9475 ) ;
#35878 = CARTESIAN_POINT ( 'NONE',  ( 0.000000000000000000, 25.88420570971438650, -27.13269053701069566 ) ) ;
#35879 = ORIENTED_EDGE ( 'NONE', *, *, #2159, .T. ) ;
#35880 = ORIENTED_EDGE ( 'NONE', *, *, #1863, .T. ) ;
#35881 =( GEOMETRIC_REPRESENTATION_CONTEXT ( 3 ) GLOBAL_UNCERTAINTY_ASSIGNED_CONTEXT ( ( #23244 ) ) GLOBAL_UNIT_ASSIGNED_CONTEXT ( ( #33518, #48447, #28882 ) ) REPRESENTATION_CONTEXT ( 'NONE', 'WORKASPACE' ) );
#35882 = EDGE_CURVE ( 'NONE', #41559, #29480, #10202, .T. ) ;
#35883 = CARTESIAN_POINT ( 'NONE',  ( 0.000000000000000000, 0.000000000000000000, 0.000000000000000000 ) ) ;
#35884 = ORIENTED_EDGE ( 'NONE', *, *, #19347, .F. ) ;
#35885 = ORIENTED_EDGE ( 'NONE', *, *, #17642, .F. ) ;
#35886 = AXIS2_PLACEMENT_3D ( 'NONE', #29, #37249, #2749 ) ;
#35887 = VECTOR ( 'NONE', #2645, 1000.000000000000000 ) ;
#35888 = CARTESIAN_POINT ( 'NONE',  ( 0.000000000000000000, 46.21855187248719687, -62.20884554313968806 ) ) ;
#35890 = ORIENTED_EDGE ( 'NONE', *, *, #3756, .F. ) ;
#35889 = LINE ( 'NONE', #24877, #33178 ) ;
#35891 = CIRCLE ( 'NONE', #3860, 31.99999999999998934 ) ;
#35892 = VERTEX_POINT ( 'NONE', #28809 ) ;
#35893 = ORIENTED_EDGE ( 'NONE', *, *, #29169, .T. ) ;
#35894 = ORIENTED_EDGE ( 'NONE', *, *, #40944, .F. ) ;
#35895 = DIRECTION ( 'NONE',  ( -1.000000000000000000, -0.000000000000000000, -0.000000000000000000 ) ) ;
#35896 = CARTESIAN_POINT ( 'NONE',  ( 11.99999999999999822, 75.11764819372142199, 2.946379043147685728 ) ) ;
#35897 = DIRECTION ( 'NONE',  ( 1.000000000000000000, 0.000000000000000000, 0.000000000000000000 ) ) ;
#35898 = ORIENTED_EDGE ( 'NONE', *, *, #46665, .F. ) ;
#35899 = ORIENTED_EDGE ( 'NONE', *, *, #18890, .T. ) ;
#35900 = CIRCLE ( 'NONE', #21851, 31.99999999999998934 ) ;
#35901 = DIRECTION ( 'NONE',  ( 0.000000000000000000, 0.000000000000000000, 1.000000000000000000 ) ) ;
#35902 = ORIENTED_EDGE ( 'NONE', *, *, #8542, .T. ) ;
#35903 = CARTESIAN_POINT ( 'NONE',  ( -3.000000000000000000, 0.000000000000000000, 0.000000000000000000 ) ) ;
#35904 = DIRECTION ( 'NONE',  ( 1.000000000000000000, 0.000000000000000000, -0.000000000000000000 ) ) ;
#35905 = EDGE_CURVE ( 'NONE', #15072, #15224, #33515, .T. ) ;
#35906 = DIRECTION ( 'NONE',  ( -1.000000000000000000, 0.000000000000000000, 0.000000000000000000 ) ) ;
#35907 = DIRECTION ( 'NONE',  ( -1.000000000000000000, 0.000000000000000000, 0.000000000000000000 ) ) ;
#35908 = DIRECTION ( 'NONE',  ( -1.000000000000000000, -0.000000000000000000, -0.000000000000000000 ) ) ;
#35909 = EDGE_CURVE ( 'NONE', #17390, #39882, #13987, .T. ) ;
#35910 = EDGE_CURVE ( 'NONE', #16057, #29685, #6071, .T. ) ;
#35911 = DIRECTION ( 'NONE',  ( 0.000000000000000000, 0.000000000000000000, 1.000000000000000000 ) ) ;
#35912 = EDGE_CURVE ( 'NONE', #43484, #25704, #2368, .T. ) ;
#35913 = CARTESIAN_POINT ( 'NONE',  ( 10.00000000000000000, -16.23288003029473359, -33.80338159004301701 ) ) ;
#35914 = ORIENTED_EDGE ( 'NONE', *, *, #5531, .F. ) ;
#35915 = EDGE_CURVE ( 'NONE', #894, #15085, #23356, .T. ) ;
#35916 = CARTESIAN_POINT ( 'NONE',  ( 0.000000000000000000, 16.45098606841126454, 33.79645857604518966 ) ) ;
#35917 = EDGE_LOOP ( 'NONE', ( #26673, #2836, #16023, #7844 ) ) ;
#35918 = DIRECTION ( 'NONE',  ( 0.000000000000000000, 0.000000000000000000, 1.000000000000000000 ) ) ;
#35919 = CARTESIAN_POINT ( 'NONE',  ( -24.50849501662245800, -109.8101191361138831, 5.500000000000000000 ) ) ;
#35920 = CARTESIAN_POINT ( 'NONE',  ( 11.99999999999999822, 26.02418014898310261, 70.52718814184268581 ) ) ;
#35921 = DIRECTION ( 'NONE',  ( -1.000000000000000000, 0.000000000000000000, -0.000000000000000000 ) ) ;
#35922 = EDGE_CURVE ( 'NONE', #26066, #48059, #10853, .T. ) ;
#35923 = DIRECTION ( 'NONE',  ( 0.9227826878668540234, 0.3853207896976547087, 0.000000000000000000 ) ) ;
#35924 = DIRECTION ( 'NONE',  ( 1.000000000000000000, 0.000000000000000000, 0.000000000000000000 ) ) ;
#35925 = VECTOR ( 'NONE', #11254, 1000.000000000000000 ) ;
#35926 = ORIENTED_EDGE ( 'NONE', *, *, #41494, .F. ) ;
#35927 = DIRECTION ( 'NONE',  ( -1.000000000000000000, 0.000000000000000000, 0.000000000000000000 ) ) ;
#35928 = LINE ( 'NONE', #35453, #7312 ) ;
#35929 = CIRCLE ( 'NONE', #14831, 31.99999999999999645 ) ;
#35930 = CARTESIAN_POINT ( 'NONE',  ( 10.00000000000000000, 0.000000000000000000, 0.000000000000000000 ) ) ;
#35931 = EDGE_CURVE ( 'NONE', #1317, #16336, #5370, .T. ) ;
#35932 = VERTEX_POINT ( 'NONE', #24407 ) ;
#35933 = AXIS2_PLACEMENT_3D ( 'NONE', #21568, #10293, #29134 ) ;
#35934 = CARTESIAN_POINT ( 'NONE',  ( 0.000000000000000000, 60.67117009219215618, -55.16347631942977614 ) ) ;
#35935 = VERTEX_POINT ( 'NONE', #47413 ) ;
#35936 = ORIENTED_EDGE ( 'NONE', *, *, #33838, .T. ) ;
#35937 = EDGE_LOOP ( 'NONE', ( #31039, #34091, #45016, #41879 ) ) ;
#35938 = EDGE_CURVE ( 'NONE', #43255, #6361, #37439, .T. ) ;
#35939 = AXIS2_PLACEMENT_3D ( 'NONE', #42906, #48252, #10811 ) ;
#35940 = ORIENTED_EDGE ( 'NONE', *, *, #11997, .F. ) ;
#35941 = VERTEX_POINT ( 'NONE', #17784 ) ;
#35942 = CYLINDRICAL_SURFACE ( 'NONE', #14807, 16.00000000000000000 ) ;
#35943 = CARTESIAN_POINT ( 'NONE',  ( 15.00000000000000000, -3.948201729842032215, 23.21447184625297666 ) ) ;
#35944 = ORIENTED_EDGE ( 'NONE', *, *, #12888, .T. ) ;
#35945 = ADVANCED_FACE ( 'NONE', ( #47637 ), #35678, .F. ) ;
#35946 = DIRECTION ( 'NONE',  ( 1.000000000000000000, 0.000000000000000000, 0.000000000000000000 ) ) ;
#35947 = VERTEX_POINT ( 'NONE', #17062 ) ;
#35948 = EDGE_LOOP ( 'NONE', ( #41855, #519, #32469, #47404 ) ) ;
#35949 = ORIENTED_EDGE ( 'NONE', *, *, #10622, .F. ) ;
#35950 = EDGE_LOOP ( 'NONE', ( #42910, #10846, #23265, #38254 ) ) ;
#35951 = ORIENTED_EDGE ( 'NONE', *, *, #43551, .F. ) ;
#35952 = AXIS2_PLACEMENT_3D ( 'NONE', #29112, #10272, #6610 ) ;
#35953 = CARTESIAN_POINT ( 'NONE',  ( 0.000000000000000000, 0.000000000000000000, 0.000000000000000000 ) ) ;
#35955 = ORIENTED_EDGE ( 'NONE', *, *, #36120, .T. ) ;
#35954 = AXIS2_PLACEMENT_3D ( 'NONE', #38305, #5742, #16281 ) ;
#35956 = CARTESIAN_POINT ( 'NONE',  ( 0.000000000000000000, 35.53030884539084866, 12.26510123303271982 ) ) ;
#35957 = ORIENTED_EDGE ( 'NONE', *, *, #27421, .T. ) ;
#35958 = EDGE_CURVE ( 'NONE', #29152, #17248, #29605, .T. ) ;
#35959 = CARTESIAN_POINT ( 'NONE',  ( 0.000000000000000000, -74.65491531819111515, -8.830959090343204920 ) ) ;
#35960 = CIRCLE ( 'NONE', #779, 82.00000000000000000 ) ;
#35961 = DIRECTION ( 'NONE',  ( -1.000000000000000000, 0.000000000000000000, -0.000000000000000000 ) ) ;
#35962 = CARTESIAN_POINT ( 'NONE',  ( 0.000000000000000000, 75.11725578898472122, -2.956366410619845730 ) ) ;
#35963 = ORIENTED_EDGE ( 'NONE', *, *, #34019, .T. ) ;
#35964 = ADVANCED_FACE ( 'NONE', ( #1699 ), #17102, .T. ) ;
#35965 = CIRCLE ( 'NONE', #9407, 15.99999999999999822 ) ;
#35966 = DIRECTION ( 'NONE',  ( 1.000000000000000000, 0.000000000000000000, 0.000000000000000000 ) ) ;
#35967 = ORIENTED_EDGE ( 'NONE', *, *, #37072, .T. ) ;
#35968 = AXIS2_PLACEMENT_3D ( 'NONE', #18689, #7450, #11843 ) ;
#35969 = DIRECTION ( 'NONE',  ( -1.000000000000000000, 0.000000000000000000, 0.000000000000000000 ) ) ;
#35970 = DIRECTION ( 'NONE',  ( -1.000000000000000000, 0.000000000000000000, -0.000000000000000000 ) ) ;
#35971 = ORIENTED_EDGE ( 'NONE', *, *, #48121, .F. ) ;
#35972 = VECTOR ( 'NONE', #18075, 1000.000000000000000 ) ;
#35973 = VERTEX_POINT ( 'NONE', #43301 ) ;
#35974 = ADVANCED_FACE ( 'NONE', ( #23979 ), #1217, .T. ) ;
#35975 = DIRECTION ( 'NONE',  ( -0.000000000000000000, -0.000000000000000000, -1.000000000000000000 ) ) ;
#35976 = DIRECTION ( 'NONE',  ( -1.000000000000000000, 0.000000000000000000, -0.000000000000000000 ) ) ;
#35977 = ORIENTED_EDGE ( 'NONE', *, *, #26275, .F. ) ;
#35978 = CARTESIAN_POINT ( 'NONE',  ( 0.000000000000000000, 68.55367621811205936, -44.99326035065983120 ) ) ;
#35979 = LINE ( 'NONE', #24735, #47728 ) ;
#35980 = CARTESIAN_POINT ( 'NONE',  ( -10.00000000000000000, 0.000000000000000000, 0.000000000000000000 ) ) ;
#35981 = CARTESIAN_POINT ( 'NONE',  ( 12.00000000000000000, -0.9646360437372099028, 23.52805723605590771 ) ) ;
#35982 = DIRECTION ( 'NONE',  ( -1.000000000000000000, -0.000000000000000000, 0.000000000000000000 ) ) ;
#35983 = DIRECTION ( 'NONE',  ( -1.000000000000000000, 0.000000000000000000, 0.000000000000000000 ) ) ;
#35984 = DIRECTION ( 'NONE',  ( 0.000000000000000000, 0.000000000000000000, -1.000000000000000000 ) ) ;
#35985 = DIRECTION ( 'NONE',  ( -0.000000000000000000, -0.6691306063588569053, -0.7431448254773954654 ) ) ;
#35986 = CARTESIAN_POINT ( 'NONE',  ( 15.00000000000000000, -10.45096189432344502, -21.10159698893425784 ) ) ;
#35987 = CARTESIAN_POINT ( 'NONE',  ( -19.90058851926621131, -132.5883508287165853, -5.500000000000000000 ) ) ;
#35988 = DIRECTION ( 'NONE',  ( -0.000000000000000000, -0.6691306063588569053, -0.7431448254773954654 ) ) ;
#35989 = LINE ( 'NONE', #829, #34200 ) ;
#35990 = VERTEX_POINT ( 'NONE', #43054 ) ;
#35991 = CIRCLE ( 'NONE', #14090, 31.99999999999999289 ) ;
#35992 = CIRCLE ( 'NONE', #18788, 82.00000000000000000 ) ;
#35993 = CARTESIAN_POINT ( 'NONE',  ( 0.000000000000000000, 0.000000000000000000, 0.000000000000000000 ) ) ;
#35994 = VECTOR ( 'NONE', #35802, 1000.000000000000000 ) ;
#35995 = AXIS2_PLACEMENT_3D ( 'NONE', #36726, #6167, #36253 ) ;
#35996 = CONTEXT_DEPENDENT_SHAPE_REPRESENTATION ( #38525, #12517 ) ;
#35997 = DIRECTION ( 'NONE',  ( -1.000000000000000000, -0.000000000000000000, -0.000000000000000000 ) ) ;
#35998 = EDGE_LOOP ( 'NONE', ( #39324, #15877, #33267, #26647 ) ) ;
#35999 = AXIS2_PLACEMENT_3D ( 'NONE', #19824, #34763, #31114 ) ;
#36000 = VECTOR ( 'NONE', #6191, 1000.000000000000000 ) ;
#36001 = CIRCLE ( 'NONE', #17269, 82.00000000000000000 ) ;
#36002 = FACE_OUTER_BOUND ( 'NONE', #16093, .T. ) ;
#36003 = DIRECTION ( 'NONE',  ( 0.000000000000000000, -0.4539904997395541320, 0.8910065241883640130 ) ) ;
#36004 = VERTEX_POINT ( 'NONE', #31825 ) ;
#36005 = DIRECTION ( 'NONE',  ( 1.000000000000000000, 0.000000000000000000, 0.000000000000000000 ) ) ;
#36006 = EDGE_CURVE ( 'NONE', #10618, #5001, #16335, .T. ) ;
#36007 = ORIENTED_EDGE ( 'NONE', *, *, #7021, .T. ) ;
#36008 = CARTESIAN_POINT ( 'NONE',  ( 10.00000000000000000, 15.48615015657638239, -39.04073710021328480 ) ) ;
#36009 = DIRECTION ( 'NONE',  ( -1.000000000000000000, 0.000000000000000000, 0.000000000000000000 ) ) ;
#36010 = EDGE_LOOP ( 'NONE', ( #8516, #16618, #4649, #5761 ) ) ;
#36011 = ADVANCED_FACE ( 'NONE', ( #31327 ), #38912, .T. ) ;
#36012 = DIRECTION ( 'NONE',  ( 0.000000000000000000, 0.000000000000000000, 1.000000000000000000 ) ) ;
#36013 = ORIENTED_EDGE ( 'NONE', *, *, #160, .F. ) ;
#36014 = ORIENTED_EDGE ( 'NONE', *, *, #30718, .T. ) ;
#36015 = EDGE_CURVE ( 'NONE', #42769, #28690, #19427, .T. ) ;
#36016 = LINE ( 'NONE', #47288, #45458 ) ;
#36017 = CARTESIAN_POINT ( 'NONE',  ( 0.000000000000000000, -74.74816331893454446, 33.71516098798714722 ) ) ;
#36018 = DIRECTION ( 'NONE',  ( -1.000000000000000000, -0.000000000000000000, -0.000000000000000000 ) ) ;
#36019 = AXIS2_PLACEMENT_3D ( 'NONE', #4508, #16729, #46105 ) ;
#36021 = VERTEX_POINT ( 'NONE', #13435 ) ;
#36020 = CARTESIAN_POINT ( 'NONE',  ( 10.00000000000000000, -65.64334221924939072, 41.19522573413710376 ) ) ;
#36022 = DIRECTION ( 'NONE',  ( -1.000000000000000000, 0.000000000000000000, 0.000000000000000000 ) ) ;
#36023 = ORIENTED_EDGE ( 'NONE', *, *, #40682, .F. ) ;
#36024 = CIRCLE ( 'NONE', #7868, 82.00000000000000000 ) ;
#36025 = FACE_OUTER_BOUND ( 'NONE', #29521, .T. ) ;
#36026 = ORIENTED_EDGE ( 'NONE', *, *, #27163, .T. ) ;
#36027 = VERTEX_POINT ( 'NONE', #9274 ) ;
#36028 = EDGE_CURVE ( 'NONE', #12206, #59, #35864, .T. ) ;
#36029 = DIRECTION ( 'NONE',  ( 0.000000000000000000, 0.7431448254773954654, 0.6691306063588569053 ) ) ;
#36030 = AXIS2_PLACEMENT_3D ( 'NONE', #40449, #39490, #32835 ) ;
#36031 = EDGE_LOOP ( 'NONE', ( #42036, #19802, #46586, #27065 ) ) ;
#36032 = AXIS2_PLACEMENT_3D ( 'NONE', #40836, #44742, #4121 ) ;
#36033 = CARTESIAN_POINT ( 'NONE',  ( 10.00000000000000000, 0.000000000000000000, 0.000000000000000000 ) ) ;
#36034 = EDGE_CURVE ( 'NONE', #11188, #6193, #4593, .T. ) ;
#36035 = CARTESIAN_POINT ( 'NONE',  ( 10.00000000000000000, 36.73666225445894185, 65.58780272294090707 ) ) ;
#36036 = FACE_OUTER_BOUND ( 'NONE', #21066, .T. ) ;
#36037 = VERTEX_POINT ( 'NONE', #46012 ) ;
#36038 = LINE ( 'NONE', #33990, #33930 ) ;
#36039 = CARTESIAN_POINT ( 'NONE',  ( 0.000000000000000000, 71.87247863392414615, 39.47590169984871267 ) ) ;
#36040 = VECTOR ( 'NONE', #4395, 1000.000000000000000 ) ;
#36041 = DIRECTION ( 'NONE',  ( -0.6064928550163524168, -0.7950889364178789220, 0.000000000000000000 ) ) ;
#36042 = DIRECTION ( 'NONE',  ( -0.000000000000000000, 0.8660254037844432595, 0.4999999999999921729 ) ) ;
#36043 = EDGE_LOOP ( 'NONE', ( #27722, #14633, #46256, #3269 ) ) ;
#36044 = PRESENTATION_LAYER_ASSIGNMENT (  '', '', ( #5479 ) ) ;
#36045 = DIRECTION ( 'NONE',  ( 0.000000000000000000, -0.5224985647159380298, -0.8526401643540988395 ) ) ;
#36046 = LINE ( 'NONE', #2507, #12943 ) ;
#36047 = DIRECTION ( 'NONE',  ( 0.000000000000000000, 0.000000000000000000, 1.000000000000000000 ) ) ;
#36048 = CARTESIAN_POINT ( 'NONE',  ( 0.000000000000000000, -11.95096189432345390, 23.69967320028757385 ) ) ;
#36049 = EDGE_CURVE ( 'NONE', #40832, #12600, #46810, .T. ) ;
#36050 = ORIENTED_EDGE ( 'NONE', *, *, #13808, .F. ) ;
#36051 = DIRECTION ( 'NONE',  ( 0.000000000000000000, 0.000000000000000000, 1.000000000000000000 ) ) ;
#36052 = CARTESIAN_POINT ( 'NONE',  ( -43.60332556124591008, -123.0000000000000142, 2.500000000000000000 ) ) ;
#36053 = EDGE_LOOP ( 'NONE', ( #22894, #26702, #46363, #43066 ) ) ;
#36054 = ORIENTED_EDGE ( 'NONE', *, *, #42077, .F. ) ;
#36055 = FACE_OUTER_BOUND ( 'NONE', #44076, .T. ) ;
#36056 = ORIENTED_EDGE ( 'NONE', *, *, #4094, .T. ) ;
#36057 = DIRECTION ( 'NONE',  ( -1.000000000000000000, 0.000000000000000000, 0.000000000000000000 ) ) ;
#36058 = CARTESIAN_POINT ( 'NONE',  ( 0.000000000000000000, 76.66974797899835892, 11.30684508768366570 ) ) ;
#36059 = ORIENTED_EDGE ( 'NONE', *, *, #43448, .T. ) ;
#36060 = AXIS2_PLACEMENT_3D ( 'NONE', #30164, #37251, #48265 ) ;
#36061 = EDGE_CURVE ( 'NONE', #31833, #45052, #39386, .T. ) ;
#36062 = CIRCLE ( 'NONE', #12637, 31.99999999999998579 ) ;
#36063 = AXIS2_PLACEMENT_3D ( 'NONE', #20549, #35493, #33917 ) ;
#36064 = AXIS2_PLACEMENT_3D ( 'NONE', #27863, #42782, #20249 ) ;
#36065 = EDGE_CURVE ( 'NONE', #18356, #41330, #44458, .T. ) ;
#36066 = CYLINDRICAL_SURFACE ( 'NONE', #40137, 82.00000000000000000 ) ;
#36067 = VERTEX_POINT ( 'NONE', #5372 ) ;
#36068 = ORIENTED_EDGE ( 'NONE', *, *, #25439, .F. ) ;
#36069 = ORIENTED_EDGE ( 'NONE', *, *, #32268, .T. ) ;
#36070 = EDGE_CURVE ( 'NONE', #2611, #28645, #39794, .T. ) ;
#36071 = CIRCLE ( 'NONE', #1702, 77.49900000000000944 ) ;
#36072 = CARTESIAN_POINT ( 'NONE',  ( 0.000000000000000000, 74.65491531819118620, -8.830959090342659579 ) ) ;
#36073 = EDGE_LOOP ( 'NONE', ( #29091, #7821, #30717, #23536 ) ) ;
#36074 = AXIS2_PLACEMENT_3D ( 'NONE', #19181, #584, #26293 ) ;
#36075 = DIRECTION ( 'NONE',  ( -1.000000000000000000, 0.000000000000000000, 0.000000000000000000 ) ) ;
#36076 = DIRECTION ( 'NONE',  ( 0.000000000000000000, -6.938893903907228378E-15, 1.000000000000000000 ) ) ;
#36077 = CIRCLE ( 'NONE', #15750, 31.99999999999999289 ) ;
#36078 = VERTEX_POINT ( 'NONE', #27907 ) ;
#36079 = DIRECTION ( 'NONE',  ( 0.000000000000000000, 0.000000000000000000, 1.000000000000000000 ) ) ;
#36080 = EDGE_CURVE ( 'NONE', #47237, #41733, #5615, .T. ) ;
#36081 = ORIENTED_EDGE ( 'NONE', *, *, #46966, .F. ) ;
#36082 = ORIENTED_EDGE ( 'NONE', *, *, #42954, .T. ) ;
#36083 = EDGE_CURVE ( 'NONE', #35253, #7167, #28835, .T. ) ;
#36084 = EDGE_CURVE ( 'NONE', #5383, #29067, #27286, .T. ) ;
#36085 = CARTESIAN_POINT ( 'NONE',  ( 10.00000000000000000, 73.72996012237460661, -14.67089635893632504 ) ) ;
#36086 = PLANE ( 'NONE',  #37443 ) ;
#36087 = DIRECTION ( 'NONE',  ( 0.000000000000000000, 0.000000000000000000, 1.000000000000000000 ) ) ;
#36088 = ORIENTED_EDGE ( 'NONE', *, *, #42458, .F. ) ;
#36089 = DIRECTION ( 'NONE',  ( 0.000000000000000000, 0.000000000000000000, 1.000000000000000000 ) ) ;
#36090 = VERTEX_POINT ( 'NONE', #2180 ) ;
#36091 = ORIENTED_EDGE ( 'NONE', *, *, #4763, .T. ) ;
#36092 = FACE_BOUND ( 'NONE', #3618, .T. ) ;
#36093 = CARTESIAN_POINT ( 'NONE',  ( 0.000000000000000000, 0.000000000000000000, 0.000000000000000000 ) ) ;
#36094 = CARTESIAN_POINT ( 'NONE',  ( 11.99999999999999822, 41.76106447765489094, 62.50884508063442269 ) ) ;
#36095 = CARTESIAN_POINT ( 'NONE',  ( 0.000000000000000000, -120.0000000000000000, 125.0000000000000000 ) ) ;
#36096 = FACE_OUTER_BOUND ( 'NONE', #5727, .T. ) ;
#36097 = CARTESIAN_POINT ( 'NONE',  ( 10.00000000000000000, -31.52238457039619490, 27.75498641678731104 ) ) ;
#36098 = LINE ( 'NONE', #13588, #15666 ) ;
#36099 = CARTESIAN_POINT ( 'NONE',  ( 0.000000000000000000, 0.000000000000000000, 0.000000000000000000 ) ) ;
#36100 = CIRCLE ( 'NONE', #24357, 31.99999999999998934 ) ;
#36101 = CARTESIAN_POINT ( 'NONE',  ( 26.28306158492127764, -123.3838844133976522, -2.500000000000000000 ) ) ;
#36102 = CARTESIAN_POINT ( 'NONE',  ( -3.000000000000000000, -23.29833615347104825, -3.418703333116803744 ) ) ;
#36103 = ORIENTED_EDGE ( 'NONE', *, *, #48043, .T. ) ;
#36104 = AXIS2_PLACEMENT_3D ( 'NONE', #47573, #33135, #17722 ) ;
#36105 = DIRECTION ( 'NONE',  ( 0.000000000000000000, 0.000000000000000000, 1.000000000000000000 ) ) ;
#36106 = VECTOR ( 'NONE', #21929, 1000.000000000000000 ) ;
#36107 = CARTESIAN_POINT ( 'NONE',  ( 10.00000000000000000, 0.000000000000000000, 0.000000000000000000 ) ) ;
#36108 = CARTESIAN_POINT ( 'NONE',  ( 10.00000000000000000, -74.65374052328654386, 8.840884882374837161 ) ) ;
#36109 = CIRCLE ( 'NONE', #12671, 31.99999999999998934 ) ;
#36110 = CARTESIAN_POINT ( 'NONE',  ( 0.000000000000000000, 71.91182617369230456, -28.89263327155667938 ) ) ;
#36111 = EDGE_LOOP ( 'NONE', ( #28250, #33605, #13921, #25572 ) ) ;
#36112 = CARTESIAN_POINT ( 'NONE',  ( -10.00000000000000000, 0.000000000000000000, 0.000000000000000000 ) ) ;
#36113 = LINE ( 'NONE', #35144, #15186 ) ;
#36114 = VERTEX_POINT ( 'NONE', #28360 ) ;
#36115 = CARTESIAN_POINT ( 'NONE',  ( 0.000000000000000000, 0.000000000000000000, 0.000000000000000000 ) ) ;
#36116 = AXIS2_PLACEMENT_3D ( 'NONE', #43785, #3137, #44275 ) ;
#36117 = DIRECTION ( 'NONE',  ( -1.000000000000000000, -0.000000000000000000, 0.000000000000000000 ) ) ;
#36118 = ORIENTED_EDGE ( 'NONE', *, *, #1670, .T. ) ;
#36119 = VERTEX_POINT ( 'NONE', #38417 ) ;
#36120 = EDGE_CURVE ( 'NONE', #7668, #17290, #6174, .T. ) ;
#36121 = VERTEX_POINT ( 'NONE', #21502 ) ;
#36122 = ADVANCED_FACE ( 'NONE', ( #14649 ), #43540, .F. ) ;
#36123 = FACE_OUTER_BOUND ( 'NONE', #23414, .T. ) ;
#36124 = ORIENTED_EDGE ( 'NONE', *, *, #21495, .F. ) ;
#36125 = EDGE_CURVE ( 'NONE', #43252, #5777, #28613, .T. ) ;
#36126 = ORIENTED_EDGE ( 'NONE', *, *, #24210, .T. ) ;
#36127 = AXIS2_PLACEMENT_3D ( 'NONE', #40743, #45376, #37319 ) ;
#36128 = DIRECTION ( 'NONE',  ( -1.000000000000000000, 0.000000000000000000, 0.000000000000000000 ) ) ;
#36129 = AXIS2_PLACEMENT_3D ( 'NONE', #47932, #33004, #10752 ) ;
#36130 = DIRECTION ( 'NONE',  ( -1.000000000000000000, -0.000000000000000000, -0.000000000000000000 ) ) ;
#36131 = ORIENTED_EDGE ( 'NONE', *, *, #43649, .F. ) ;
#36132 = VERTEX_POINT ( 'NONE', #17579 ) ;
#36133 = ORIENTED_EDGE ( 'NONE', *, *, #31128, .F. ) ;
#36134 = AXIS2_PLACEMENT_3D ( 'NONE', #8175, #23107, #38274 ) ;
#36135 = EDGE_CURVE ( 'NONE', #29511, #8888, #3120, .T. ) ;
#36136 = ADVANCED_FACE ( 'NONE', ( #47667 ), #6569, .F. ) ;
#36137 = DIRECTION ( 'NONE',  ( 0.000000000000000000, 0.9723699203976773342, -0.2334453638559024213 ) ) ;
#36138 = LINE ( 'NONE', #2596, #45387 ) ;
#36139 = CARTESIAN_POINT ( 'NONE',  ( 10.00000000000000000, 55.38113227695782115, 54.21277698773695164 ) ) ;
#36140 = ORIENTED_EDGE ( 'NONE', *, *, #7897, .T. ) ;
#36141 = ORIENTED_EDGE ( 'NONE', *, *, #35909, .F. ) ;
#36142 = ORIENTED_EDGE ( 'NONE', *, *, #8243, .F. ) ;
#36143 = DIRECTION ( 'NONE',  ( 1.000000000000000000, 0.000000000000000000, 0.000000000000000000 ) ) ;
#36144 = VERTEX_POINT ( 'NONE', #40582 ) ;
#36145 = LINE ( 'NONE', #47877, #2221 ) ;
#36146 = AXIS2_PLACEMENT_3D ( 'NONE', #46181, #27580, #45701 ) ;
#36147 = FACE_BOUND ( 'NONE', #27822, .T. ) ;
#36148 = DIRECTION ( 'NONE',  ( 1.000000000000000000, 0.000000000000000000, 0.000000000000000000 ) ) ;
#36149 = CARTESIAN_POINT ( 'NONE',  ( 15.00000000000000000, -19.89357724625003598, -12.59942793731059041 ) ) ;
#36150 = LINE ( 'NONE', #21943, #39087 ) ;
#36151 = EDGE_CURVE ( 'NONE', #45717, #30959, #7041, .T. ) ;
#36152 = DIRECTION ( 'NONE',  ( 0.000000000000000000, -6.982962677686267499E-15, 1.000000000000000000 ) ) ;
#36153 = ORIENTED_EDGE ( 'NONE', *, *, #38405, .T. ) ;
#36154 = DIRECTION ( 'NONE',  ( -1.000000000000000000, 0.000000000000000000, -0.000000000000000000 ) ) ;
#36155 = VERTEX_POINT ( 'NONE', #36892 ) ;
#36156 = VECTOR ( 'NONE', #3393, 1000.000000000000000 ) ;
#36157 = FACE_OUTER_BOUND ( 'NONE', #45594, .T. ) ;
#36158 = CARTESIAN_POINT ( 'NONE',  ( 10.00000000000000000, 0.000000000000000000, 0.000000000000000000 ) ) ;
#36159 = DIRECTION ( 'NONE',  ( -1.000000000000000000, 0.000000000000000000, -0.000000000000000000 ) ) ;
#36160 = AXIS2_PLACEMENT_3D ( 'NONE', #6217, #36057, #6447 ) ;
#36161 = DIRECTION ( 'NONE',  ( 0.000000000000000000, 0.000000000000000000, -1.000000000000000000 ) ) ;
#36162 = DIRECTION ( 'NONE',  ( -0.7950889364178796992, 0.6064928550163511956, 0.000000000000000000 ) ) ;
#36164 = CIRCLE ( 'NONE', #24432, 37.49900000000000233 ) ;
#36163 = CARTESIAN_POINT ( 'NONE',  ( 5.000000000000000000, 33.71516098798849015, -74.74816331893393340 ) ) ;
#36165 = ORIENTED_EDGE ( 'NONE', *, *, #2758, .F. ) ;
#36166 = DIRECTION ( 'NONE',  ( -1.000000000000000000, 0.000000000000000000, -0.000000000000000000 ) ) ;
#36167 = LINE ( 'NONE', #47194, #1063 ) ;
#36168 = DIRECTION ( 'NONE',  ( -1.000000000000000000, -0.000000000000000000, -0.000000000000000000 ) ) ;
#36169 = CIRCLE ( 'NONE', #207, 11.59999999999999787 ) ;
#36170 = AXIS2_PLACEMENT_3D ( 'NONE', #27873, #1179, #13403 ) ;
#36171 = CYLINDRICAL_SURFACE ( 'NONE', #43268, 37.49900000000000233 ) ;
#36172 = CIRCLE ( 'NONE', #27590, 82.00000000000000000 ) ;
#36173 = ORIENTED_EDGE ( 'NONE', *, *, #15009, .F. ) ;
#36174 = ORIENTED_EDGE ( 'NONE', *, *, #23662, .T. ) ;
#36175 = AXIS2_PLACEMENT_3D ( 'NONE', #38517, #23104, #4981 ) ;
#36176 = ORIENTED_EDGE ( 'NONE', *, *, #33312, .T. ) ;
#36177 = CIRCLE ( 'NONE', #10403, 31.99999999999998579 ) ;
#36178 = ADVANCED_FACE ( 'NONE', ( #43770 ), #36658, .T. ) ;
#36179 = CARTESIAN_POINT ( 'NONE',  ( 15.00000000000000000, 20.85821328998741109, -10.92862929874522671 ) ) ;
#36180 = CARTESIAN_POINT ( 'NONE',  ( 0.000000000000000000, 37.48860685352291000, -0.8828120875901940279 ) ) ;
#36181 = ORIENTED_EDGE ( 'NONE', *, *, #6957, .T. ) ;
#36182 = EDGE_CURVE ( 'NONE', #25081, #20359, #26474, .T. ) ;
#36183 = ORIENTED_EDGE ( 'NONE', *, *, #42497, .T. ) ;
#36184 = EDGE_CURVE ( 'NONE', #33159, #42195, #17859, .T. ) ;
#36185 = CARTESIAN_POINT ( 'NONE',  ( 19.12409105625795291, -101.5943176906707919, -5.500000000000000000 ) ) ;
#36186 = ORIENTED_EDGE ( 'NONE', *, *, #281, .F. ) ;
#36187 = ORIENTED_EDGE ( 'NONE', *, *, #10984, .F. ) ;
#36188 = ORIENTED_EDGE ( 'NONE', *, *, #12074, .F. ) ;
#36189 = VECTOR ( 'NONE', #29384, 1000.000000000000000 ) ;
#36190 = EDGE_CURVE ( 'NONE', #35058, #36090, #44495, .T. ) ;
#36191 = AXIS2_PLACEMENT_3D ( 'NONE', #3485, #29668, #40939 ) ;
#36192 = CARTESIAN_POINT ( 'NONE',  ( 10.00000000000000000, -77.32052557432845674, 5.256550761632577284 ) ) ;
#36193 = VERTEX_POINT ( 'NONE', #32522 ) ;
#36194 = DIRECTION ( 'NONE',  ( 0.000000000000000000, -0.3826834323650772363, -0.9238795325112919565 ) ) ;
#36195 = EDGE_CURVE ( 'NONE', #24721, #13159, #18049, .T. ) ;
#36196 = ORIENTED_EDGE ( 'NONE', *, *, #18050, .F. ) ;
#36197 = CARTESIAN_POINT ( 'NONE',  ( 0.000000000000000000, 38.55633173627034438, -16.65560815589369881 ) ) ;
#36198 = CIRCLE ( 'NONE', #11970, 16.00000000000000000 ) ;
#36199 = CIRCLE ( 'NONE', #47143, 37.49900000000000944 ) ;
#36200 = AXIS2_PLACEMENT_3D ( 'NONE', #3333, #6300, #40073 ) ;
#36201 = DIRECTION ( 'NONE',  ( -1.000000000000000000, 0.000000000000000000, 0.000000000000000000 ) ) ;
#36202 = LINE ( 'NONE', #25421, #40054 ) ;
#36203 = AXIS2_PLACEMENT_3D ( 'NONE', #14384, #29315, #44243 ) ;
#36204 = ORIENTED_EDGE ( 'NONE', *, *, #12118, .F. ) ;
#36205 = CARTESIAN_POINT ( 'NONE',  ( 0.000000000000000000, 0.000000000000000000, 0.000000000000000000 ) ) ;
#36206 = ORIENTED_EDGE ( 'NONE', *, *, #44137, .F. ) ;
#36207 = DIRECTION ( 'NONE',  ( 0.000000000000000000, 0.000000000000000000, -1.000000000000000000 ) ) ;
#36208 = ADVANCED_FACE ( 'NONE', ( #17815 ), #32744, .T. ) ;
#36209 = CARTESIAN_POINT ( 'NONE',  ( 15.00000000000000000, -13.04903810567646971, 19.60159698893442481 ) ) ;
#36210 = AXIS2_PLACEMENT_3D ( 'NONE', #11349, #40957, #29205 ) ;
#36211 = ORIENTED_EDGE ( 'NONE', *, *, #28133, .F. ) ;
#36212 = EDGE_LOOP ( 'NONE', ( #25202, #13385, #11159, #36406 ) ) ;
#36213 = CARTESIAN_POINT ( 'NONE',  ( 10.00000000000000000, 27.74655509720778568, -77.16300072079631889 ) ) ;
#36214 = CYLINDRICAL_SURFACE ( 'NONE', #44189, 31.99999999999998579 ) ;
#36215 = ORIENTED_EDGE ( 'NONE', *, *, #46664, .T. ) ;
#36216 = ORIENTED_EDGE ( 'NONE', *, *, #8542, .F. ) ;
#36217 = AXIS2_PLACEMENT_3D ( 'NONE', #46559, #35997, #9818 ) ;
#36218 = CARTESIAN_POINT ( 'NONE',  ( -6.880223345695647197, -142.5202692415819854, -5.500000000000000000 ) ) ;
#36219 = CARTESIAN_POINT ( 'NONE',  ( 10.00000000000000000, -35.38097989696520074, 12.42422080174625520 ) ) ;
#36220 = CARTESIAN_POINT ( 'NONE',  ( -23.97194136764370498, -131.3950000906648938, 5.500000000000000000 ) ) ;
#36221 = CARTESIAN_POINT ( 'NONE',  ( 0.000000000000000000, 46.53671651294032330, -59.03961581697353012 ) ) ;
#36222 = AXIS2_PLACEMENT_3D ( 'NONE', #25768, #7176, #10365 ) ;
#36223 = DIRECTION ( 'NONE',  ( 0.000000000000000000, 0.000000000000000000, 1.000000000000000000 ) ) ;
#36224 = ADVANCED_FACE ( 'NONE', ( #21966 ), #6104, .T. ) ;
#36225 = CARTESIAN_POINT ( 'NONE',  ( 5.000000000000000000, -71.21200624218768382, -40.65526001592689909 ) ) ;
#36226 = DIRECTION ( 'NONE',  ( 0.000000000000000000, 0.000000000000000000, 1.000000000000000000 ) ) ;
#36227 = DIRECTION ( 'NONE',  ( -1.000000000000000000, -0.000000000000000000, -0.000000000000000000 ) ) ;
#36228 = CARTESIAN_POINT ( 'NONE',  ( 30.50000000000000000, -120.0000000000000000, 2.500000000000000000 ) ) ;
#36229 = FILL_AREA_STYLE_COLOUR ( '', #33479 ) ;
#36230 =( NAMED_UNIT ( * ) PLANE_ANGLE_UNIT ( ) SI_UNIT ( $, .RADIAN. ) );
#36231 = DIRECTION ( 'NONE',  ( -1.000000000000000000, -0.000000000000000000, 0.000000000000000000 ) ) ;
#36232 = CIRCLE ( 'NONE', #14331, 16.00000000000000000 ) ;
#36233 = ORIENTED_EDGE ( 'NONE', *, *, #8697, .T. ) ;
#36234 = EDGE_CURVE ( 'NONE', #24923, #25899, #36625, .T. ) ;
#36235 = DIRECTION ( 'NONE',  ( 0.000000000000000000, -0.8526401643540970632, 0.5224985647159409163 ) ) ;
#36236 = AXIS2_PLACEMENT_3D ( 'NONE', #2321, #17241, #28525 ) ;
#36237 = AXIS2_PLACEMENT_3D ( 'NONE', #40553, #36399, #22188 ) ;
#36238 = CIRCLE ( 'NONE', #287, 10.00000000000000178 ) ;
#36239 = ADVANCED_FACE ( 'NONE', ( #21012 ), #35942, .T. ) ;
#36240 = CARTESIAN_POINT ( 'NONE',  ( 10.00000000000000000, 66.50666863322055633, -39.78640506895536078 ) ) ;
#36241 = ORIENTED_EDGE ( 'NONE', *, *, #19751, .F. ) ;
#36242 = EDGE_CURVE ( 'NONE', #18377, #44907, #40580, .T. ) ;
#36243 = VERTEX_POINT ( 'NONE', #21243 ) ;
#36244 = CIRCLE ( 'NONE', #15159, 77.49899999999999523 ) ;
#36245 = AXIS2_PLACEMENT_3D ( 'NONE', #1570, #34847, #1329 ) ;
#36246 = EDGE_CURVE ( 'NONE', #23602, #32725, #30422, .T. ) ;
#36247 = DIRECTION ( 'NONE',  ( 0.000000000000000000, 0.000000000000000000, 1.000000000000000000 ) ) ;
#36248 = VERTEX_POINT ( 'NONE', #30055 ) ;
#36249 = DIRECTION ( 'NONE',  ( -1.000000000000000000, -0.000000000000000000, -0.000000000000000000 ) ) ;
#36250 = VERTEX_POINT ( 'NONE', #22943 ) ;
#36251 = CARTESIAN_POINT ( 'NONE',  ( -12.50000000000000000, -107.5000000000000000, 40.00000000000000000 ) ) ;
#36252 = ORIENTED_EDGE ( 'NONE', *, *, #38416, .F. ) ;
#36253 = DIRECTION ( 'NONE',  ( 0.000000000000000000, 0.000000000000000000, -1.000000000000000000 ) ) ;
#36254 = DIRECTION ( 'NONE',  ( -1.000000000000000000, -0.000000000000000000, 0.000000000000000000 ) ) ;
#36255 = ORIENTED_EDGE ( 'NONE', *, *, #520, .T. ) ;
#36256 = FACE_OUTER_BOUND ( 'NONE', #1347, .T. ) ;
#36257 = VERTEX_POINT ( 'NONE', #30532 ) ;
#36258 = CARTESIAN_POINT ( 'NONE',  ( 10.00000000000000000, 0.000000000000000000, -2.500000000000000000 ) ) ;
#36259 = ORIENTED_EDGE ( 'NONE', *, *, #4046, .T. ) ;
#36260 = FACE_OUTER_BOUND ( 'NONE', #38794, .T. ) ;
#36261 = LINE ( 'NONE', #28912, #8150 ) ;
#36262 = DIRECTION ( 'NONE',  ( 0.000000000000000000, 0.000000000000000000, 1.000000000000000000 ) ) ;
#36263 = AXIS2_PLACEMENT_3D ( 'NONE', #5607, #9503, #39381 ) ;
#36265 = ORIENTED_EDGE ( 'NONE', *, *, #13319, .T. ) ;
#36264 = CARTESIAN_POINT ( 'NONE',  ( 11.99999999999999822, -65.64334221924882229, -41.19522573413803457 ) ) ;
#36266 = ADVANCED_FACE ( 'NONE', ( #41085 ), #41317, .T. ) ;
#36267 = AXIS2_PLACEMENT_3D ( 'NONE', #37974, #12038, #26716 ) ;
#36268 = DIRECTION ( 'NONE',  ( -1.000000000000000000, 0.000000000000000000, -0.000000000000000000 ) ) ;
#36269 = VERTEX_POINT ( 'NONE', #19022 ) ;
#36270 = CARTESIAN_POINT ( 'NONE',  ( 6.509281303079589520, -14.89695620656361008, -1.199999999999999956 ) ) ;
#36271 = ORIENTED_EDGE ( 'NONE', *, *, #13211, .F. ) ;
#36272 = ORIENTED_EDGE ( 'NONE', *, *, #43560, .F. ) ;
#36273 = DIRECTION ( 'NONE',  ( 0.000000000000000000, 0.000000000000000000, 1.000000000000000000 ) ) ;
#36274 = AXIS2_PLACEMENT_3D ( 'NONE', #34575, #1058, #30947 ) ;
#36275 = CARTESIAN_POINT ( 'NONE',  ( 11.99999999999999822, 75.54627589209970040, -17.28742895386005785 ) ) ;
#36276 = ORIENTED_EDGE ( 'NONE', *, *, #19375, .T. ) ;
#36277 = CIRCLE ( 'NONE', #41735, 37.49900000000000233 ) ;
#36278 = CARTESIAN_POINT ( 'NONE',  ( 11.99999999999999822, 0.000000000000000000, 0.000000000000000000 ) ) ;
#36279 = CARTESIAN_POINT ( 'NONE',  ( 11.99999999999999822, -71.87247863392441616, 39.47590169984818687 ) ) ;
#36280 = DIRECTION ( 'NONE',  ( -1.000000000000000000, -0.000000000000000000, 0.000000000000000000 ) ) ;
#36281 = ORIENTED_EDGE ( 'NONE', *, *, #22761, .T. ) ;
#36282 = CARTESIAN_POINT ( 'NONE',  ( 0.000000000000000000, -64.81221759200379040, 50.23322058963324110 ) ) ;
#36283 = PRODUCT ( 'Input Shaft', 'Input Shaft', '', ( #38737 ) ) ;
#36284 = EDGE_CURVE ( 'NONE', #47549, #18104, #19491, .T. ) ;
#36285 = DIRECTION ( 'NONE',  ( -0.000000000000000000, -0.000000000000000000, -1.000000000000000000 ) ) ;
#36286 = LINE ( 'NONE', #46833, #45428 ) ;
#36287 = CARTESIAN_POINT ( 'NONE',  ( 10.00000000000000178, 0.000000000000000000, 12.50000000000000000 ) ) ;
#36288 = ADVANCED_FACE ( 'NONE', ( #41803 ), #18775, .F. ) ;
#36289 = EDGE_LOOP ( 'NONE', ( #40703, #6762, #44806, #43499 ) ) ;
#36290 = AXIS2_PLACEMENT_3D ( 'NONE', #29322, #26128, #22464 ) ;
#36291 = CIRCLE ( 'NONE', #15965, 82.00000000000000000 ) ;
#36292 = CARTESIAN_POINT ( 'NONE',  ( 12.00000000000000000, -4.261787119644964150, 26.19803753235780164 ) ) ;
#36293 = FACE_OUTER_BOUND ( 'NONE', #21277, .T. ) ;
#36294 = DIRECTION ( 'NONE',  ( 0.000000000000000000, 0.6691306063588675634, -0.7431448254773856954 ) ) ;
#36296 = VECTOR ( 'NONE', #38659, 1000.000000000000000 ) ;
#36295 = DIRECTION ( 'NONE',  ( 0.000000000000000000, 0.000000000000000000, 1.000000000000000000 ) ) ;
#36297 = AXIS2_PLACEMENT_3D ( 'NONE', #19267, #19492, #46362 ) ;
#36298 = CARTESIAN_POINT ( 'NONE',  ( 10.00000000000000000, -39.04073710021333454, -15.48615015657624738 ) ) ;
#36299 = DIRECTION ( 'NONE',  ( 0.000000000000000000, -0.1564344650402382242, 0.9876883405951366601 ) ) ;
#36300 = ORIENTED_EDGE ( 'NONE', *, *, #1397, .T. ) ;
#36301 = CARTESIAN_POINT ( 'NONE',  ( 11.99999999999999822, -74.65374052328654386, 8.840884882374837161 ) ) ;
#36302 = ORIENTED_EDGE ( 'NONE', *, *, #31452, .F. ) ;
#36303 = ADVANCED_FACE ( 'NONE', ( #15378 ), #23187, .T. ) ;
#36304 = CARTESIAN_POINT ( 'NONE',  ( 11.99999999999999822, -22.90783923731575200, -78.73519480814978522 ) ) ;
#36305 = CIRCLE ( 'NONE', #41001, 42.00000000000000000 ) ;
#36306 = EDGE_CURVE ( 'NONE', #28615, #10023, #26864, .T. ) ;
#36307 = PLANE ( 'NONE',  #19738 ) ;
#36308 = ORIENTED_EDGE ( 'NONE', *, *, #40951, .F. ) ;
#36309 = VECTOR ( 'NONE', #45079, 1000.000000000000000 ) ;
#36310 = ADVANCED_FACE ( 'NONE', ( #33710 ), #26620, .T. ) ;
#36311 = VECTOR ( 'NONE', #38073, 1000.000000000000000 ) ;
#36312 = AXIS2_PLACEMENT_3D ( 'NONE', #5482, #24321, #1573 ) ;
#36313 = FACE_OUTER_BOUND ( 'NONE', #6906, .T. ) ;
#36315 = EDGE_CURVE ( 'NONE', #29561, #10410, #29637, .T. ) ;
#36314 = EDGE_LOOP ( 'NONE', ( #2739, #4660, #42065, #37910 ) ) ;
#36316 = EDGE_LOOP ( 'NONE', ( #33565, #26999, #24786, #42929 ) ) ;
#36317 = VECTOR ( 'NONE', #25592, 1000.000000000000000 ) ;
#36318 = AXIS2_PLACEMENT_3D ( 'NONE', #8590, #38466, #19137 ) ;
#36319 = CARTESIAN_POINT ( 'NONE',  ( -12.00000000000000000, 0.000000000000000000, 0.000000000000000000 ) ) ;
#36320 = CYLINDRICAL_SURFACE ( 'NONE', #17193, 31.99999999999998579 ) ;
#36321 = VECTOR ( 'NONE', #25764, 1000.000000000000000 ) ;
#36322 = LINE ( 'NONE', #17716, #3505 ) ;
#36323 = ORIENTED_EDGE ( 'NONE', *, *, #16844, .F. ) ;
#36324 = CARTESIAN_POINT ( 'NONE',  ( 0.000000000000000000, -41.19522573413780009, 65.64334221924896440 ) ) ;
#36325 = CIRCLE ( 'NONE', #14460, 31.99999999999998579 ) ;
#36326 = EDGE_LOOP ( 'NONE', ( #18251, #28902, #40759, #19084 ) ) ;
#36327 = CIRCLE ( 'NONE', #46509, 77.49899999999999523 ) ;
#36328 = CARTESIAN_POINT ( 'NONE',  ( 1.233757462863572574, -119.1468631277289347, -2.500000000000000000 ) ) ;
#36329 = DIRECTION ( 'NONE',  ( 0.000000000000000000, 0.2079116908177532363, 0.9781476007338069101 ) ) ;
#36330 = CARTESIAN_POINT ( 'NONE',  ( 0.000000000000000000, -29.01471420065617224, 76.69515212746007649 ) ) ;
#36331 = ORIENTED_EDGE ( 'NONE', *, *, #3087, .T. ) ;
#36332 = LINE ( 'NONE', #11112, #45126 ) ;
#36333 = ORIENTED_EDGE ( 'NONE', *, *, #28185, .T. ) ;
#36334 = ORIENTED_EDGE ( 'NONE', *, *, #7305, .F. ) ;
#36335 = CARTESIAN_POINT ( 'NONE',  ( 0.000000000000000000, -23.16143007188376757, -73.95703589263997912 ) ) ;
#36336 = DIRECTION ( 'NONE',  ( -1.000000000000000000, 0.000000000000000000, 0.000000000000000000 ) ) ;
#36337 = DIRECTION ( 'NONE',  ( -1.000000000000000000, -0.000000000000000000, 0.000000000000000000 ) ) ;
#36338 = CARTESIAN_POINT ( 'NONE',  ( 10.00000000000000000, 71.27951684758069462, -30.41916302227035729 ) ) ;
#36339 = LINE ( 'NONE', #47371, #12003 ) ;
#36340 = CARTESIAN_POINT ( 'NONE',  ( 10.00000000000000000, -21.32104025579091910, -30.84782396557241313 ) ) ;
#36341 = DIRECTION ( 'NONE',  ( 0.000000000000000000, 0.000000000000000000, 1.000000000000000000 ) ) ;
#36342 = CYLINDRICAL_SURFACE ( 'NONE', #8203, 37.49900000000000233 ) ;
#36343 = DIRECTION ( 'NONE',  ( 0.000000000000000000, 1.000000000000000000, -9.787530781167598712E-16 ) ) ;
#36344 = VECTOR ( 'NONE', #48432, 1000.000000000000114 ) ;
#36345 = DIRECTION ( 'NONE',  ( 1.000000000000000000, 0.000000000000000000, 0.000000000000000000 ) ) ;
#36346 = ORIENTED_EDGE ( 'NONE', *, *, #33526, .T. ) ;
#36347 = ORIENTED_EDGE ( 'NONE', *, *, #25674, .T. ) ;
#36348 = PLANE ( 'NONE',  #26370 ) ;
#36349 = CIRCLE ( 'NONE', #42617, 31.99999999999999645 ) ;
#36350 = ADVANCED_FACE ( 'NONE', ( #41551 ), #8262, .F. ) ;
#36351 = DIRECTION ( 'NONE',  ( -1.000000000000000000, 0.000000000000000000, -0.000000000000000000 ) ) ;
#36352 = DIRECTION ( 'NONE',  ( 0.6516173805718079581, -0.7585478161175704948, 0.000000000000000000 ) ) ;
#36353 = EDGE_CURVE ( 'NONE', #46432, #22825, #15129, .T. ) ;
#36354 = CARTESIAN_POINT ( 'NONE',  ( 0.000000000000000000, 0.000000000000000000, 0.000000000000000000 ) ) ;
#36355 = AXIS2_PLACEMENT_3D ( 'NONE', #41992, #34613, #1097 ) ;
#36356 = VECTOR ( 'NONE', #10666, 1000.000000000000000 ) ;
#36357 = DIRECTION ( 'NONE',  ( -1.000000000000000000, 0.000000000000000000, -0.000000000000000000 ) ) ;
#36358 = LINE ( 'NONE', #106, #35469 ) ;
#36359 = VERTEX_POINT ( 'NONE', #25880 ) ;
#36360 = FACE_OUTER_BOUND ( 'NONE', #33726, .T. ) ;
#36361 = AXIS2_PLACEMENT_3D ( 'NONE', #38584, #5050, #42019 ) ;
#36362 = EDGE_CURVE ( 'NONE', #20992, #39592, #10119, .T. ) ;
#36363 = CARTESIAN_POINT ( 'NONE',  ( 0.000000000000000000, 31.47745569255140552, 68.26794271651274926 ) ) ;
#36364 = AXIS2_PLACEMENT_3D ( 'NONE', #16059, #46393, #20429 ) ;
#36365 = EDGE_CURVE ( 'NONE', #26919, #25452, #1526, .T. ) ;
#36366 = CIRCLE ( 'NONE', #34820, 42.00000000000000000 ) ;
#36367 = EDGE_CURVE ( 'NONE', #925, #5623, #4362, .T. ) ;
#36368 = ORIENTED_EDGE ( 'NONE', *, *, #18767, .F. ) ;
#36369 = ORIENTED_EDGE ( 'NONE', *, *, #20476, .F. ) ;
#36370 = EDGE_CURVE ( 'NONE', #22230, #27073, #41390, .T. ) ;
#36371 = ORIENTED_EDGE ( 'NONE', *, *, #10370, .F. ) ;
#36372 = AXIS2_PLACEMENT_3D ( 'NONE', #11258, #41596, #48442 ) ;
#36373 = EDGE_CURVE ( 'NONE', #15803, #9234, #46847, .T. ) ;
#36374 = CARTESIAN_POINT ( 'NONE',  ( 10.00000000000000000, 44.88180994100376608, 63.18004540533043922 ) ) ;
#36375 = ORIENTED_EDGE ( 'NONE', *, *, #2062, .T. ) ;
#36376 = ORIENTED_EDGE ( 'NONE', *, *, #47506, .F. ) ;
#36377 = AXIS2_PLACEMENT_3D ( 'NONE', #24080, #10104, #39244 ) ;
#36378 = CARTESIAN_POINT ( 'NONE',  ( 0.000000000000000000, 79.10210256391368944, 21.60688246758614994 ) ) ;
#36379 = DIRECTION ( 'NONE',  ( -1.000000000000000000, 0.000000000000000000, 0.000000000000000000 ) ) ;
#36380 = DIRECTION ( 'NONE',  ( 0.000000000000000000, 0.000000000000000000, 1.000000000000000000 ) ) ;
#36381 = EDGE_CURVE ( 'NONE', #40628, #29274, #7770, .T. ) ;
#36382 = ORIENTED_EDGE ( 'NONE', *, *, #43324, .F. ) ;
#36383 = DIRECTION ( 'NONE',  ( 0.000000000000000000, 0.000000000000000000, 1.000000000000000000 ) ) ;
#36384 = VERTEX_POINT ( 'NONE', #26138 ) ;
#36385 = VERTEX_POINT ( 'NONE', #1895 ) ;
#36386 = DIRECTION ( 'NONE',  ( 0.000000000000000000, 0.000000000000000000, 1.000000000000000000 ) ) ;
#36388 = ORIENTED_EDGE ( 'NONE', *, *, #27757, .F. ) ;
#36387 = DIRECTION ( 'NONE',  ( -1.000000000000000000, -0.000000000000000000, 0.000000000000000000 ) ) ;
#36389 = DIRECTION ( 'NONE',  ( 0.000000000000000000, -0.9876883405951358830, -0.1564344650402421932 ) ) ;
#36390 = ORIENTED_EDGE ( 'NONE', *, *, #28562, .F. ) ;
#36391 = AXIS2_PLACEMENT_3D ( 'NONE', #29463, #6946, #25538 ) ;
#36392 = VERTEX_POINT ( 'NONE', #39323 ) ;
#36393 = EDGE_LOOP ( 'NONE', ( #6912, #1078, #45125, #18355 ) ) ;
#36394 = DIRECTION ( 'NONE',  ( -0.9827303690289279636, -0.1850432970638682117, 0.000000000000000000 ) ) ;
#36395 = EDGE_LOOP ( 'NONE', ( #21194, #2736, #17358, #29089 ) ) ;
#36396 = DIRECTION ( 'NONE',  ( 0.000000000000000000, -0.3090169943749548898, 0.9510565162951511997 ) ) ;
#36397 = FACE_OUTER_BOUND ( 'NONE', #4678, .T. ) ;
#36398 = ORIENTED_EDGE ( 'NONE', *, *, #17748, .T. ) ;
#36399 = DIRECTION ( 'NONE',  ( -1.000000000000000000, 0.000000000000000000, 0.000000000000000000 ) ) ;
#36400 = CARTESIAN_POINT ( 'NONE',  ( 10.00000000000000000, 21.53537804866126137, -30.80686688396986028 ) ) ;
#36401 = ADVANCED_FACE ( 'NONE', ( #39085 ), #23421, .T. ) ;
#36402 = PLANE ( 'NONE',  #13439 ) ;
#36403 = ADVANCED_FACE ( 'NONE', ( #8728 ), #34670, .F. ) ;
#36404 = VERTEX_POINT ( 'NONE', #23666 ) ;
#36405 = CARTESIAN_POINT ( 'NONE',  ( 6.000000000000000000, 81.90746397400393164, -3.894527615416979671 ) ) ;
#36406 = ORIENTED_EDGE ( 'NONE', *, *, #7800, .T. ) ;
#36407 = EDGE_CURVE ( 'NONE', #40883, #38585, #5319, .T. ) ;
#36408 = FACE_BOUND ( 'NONE', #6815, .T. ) ;
#36409 = CIRCLE ( 'NONE', #45784, 16.00000000000000355 ) ;
#36410 = DIRECTION ( 'NONE',  ( -1.000000000000000000, -0.000000000000000000, 0.000000000000000000 ) ) ;
#36411 = CARTESIAN_POINT ( 'NONE',  ( 11.99999999999999822, 54.21277698773752007, -55.38113227695726692 ) ) ;
#36412 = CIRCLE ( 'NONE', #1274, 77.49900000000000944 ) ;
#36413 = EDGE_CURVE ( 'NONE', #22374, #36155, #12910, .T. ) ;
#36414 = DIRECTION ( 'NONE',  ( -1.000000000000000000, -0.000000000000000000, 0.000000000000000000 ) ) ;
#36415 = LINE ( 'NONE', #47652, #20114 ) ;
#36416 = AXIS2_PLACEMENT_3D ( 'NONE', #12758, #39434, #42629 ) ;
#36417 = DIRECTION ( 'NONE',  ( 0.000000000000000000, 0.000000000000000000, 1.000000000000000000 ) ) ;
#36418 = LINE ( 'NONE', #25631, #8127 ) ;
#36419 = DIRECTION ( 'NONE',  ( 0.000000000000000000, 0.000000000000000000, 1.000000000000000000 ) ) ;
#36420 = DIRECTION ( 'NONE',  ( -0.02332147558787823691, -0.9997280174009349762, 0.000000000000000000 ) ) ;
#36421 = AXIS2_PLACEMENT_3D ( 'NONE', #24617, #42247, #20445 ) ;
#36422 = VERTEX_POINT ( 'NONE', #27848 ) ;
#36423 = EDGE_CURVE ( 'NONE', #37836, #47237, #1639, .T. ) ;
#36424 = EDGE_CURVE ( 'NONE', #15559, #41267, #9221, .T. ) ;
#36425 = ORIENTED_EDGE ( 'NONE', *, *, #18537, .T. ) ;
#36426 = ORIENTED_EDGE ( 'NONE', *, *, #10160, .F. ) ;
#36427 = AXIS2_PLACEMENT_3D ( 'NONE', #24714, #40124, #37167 ) ;
#36428 = VECTOR ( 'NONE', #7866, 1000.000000000000000 ) ;
#36429 = DIRECTION ( 'NONE',  ( -0.000000000000000000, 0.5000000000000038858, 0.8660254037844363761 ) ) ;
#36430 = CARTESIAN_POINT ( 'NONE',  ( 10.00000000000000000, 16.45098606841126454, 33.79645857604518966 ) ) ;
#36431 = AXIS2_PLACEMENT_3D ( 'NONE', #4203, #12513, #19117 ) ;
#36432 = VERTEX_POINT ( 'NONE', #34924 ) ;
#36433 = EDGE_CURVE ( 'NONE', #32597, #13263, #27117, .T. ) ;
#36434 = DIRECTION ( 'NONE',  ( 0.000000000000000000, 0.000000000000000000, 1.000000000000000000 ) ) ;
#36435 = ORIENTED_EDGE ( 'NONE', *, *, #37189, .T. ) ;
#36436 = ORIENTED_EDGE ( 'NONE', *, *, #18765, .T. ) ;
#36437 = VECTOR ( 'NONE', #43877, 1000.000000000000000 ) ;
#36438 = ORIENTED_EDGE ( 'NONE', *, *, #32926, .T. ) ;
#36439 = AXIS2_PLACEMENT_3D ( 'NONE', #47050, #20867, #17896 ) ;
#36440 = VECTOR ( 'NONE', #36934, 1000.000000000000000 ) ;
#36441 = CARTESIAN_POINT ( 'NONE',  ( 10.00000000000000000, -33.00180498840060039, 17.80606268964528027 ) ) ;
#36442 = EDGE_LOOP ( 'NONE', ( #11336, #12687, #7629, #43730 ) ) ;
#36443 = CARTESIAN_POINT ( 'NONE',  ( 11.99999999999999822, -35.91791733033525702, 68.67312586194982771 ) ) ;
#36444 = VERTEX_POINT ( 'NONE', #24384 ) ;
#36445 = DIRECTION ( 'NONE',  ( 1.000000000000000000, 0.000000000000000000, 0.000000000000000000 ) ) ;
#36446 = DIRECTION ( 'NONE',  ( -1.000000000000000000, -0.000000000000000000, 0.000000000000000000 ) ) ;
#36447 = CYLINDRICAL_SURFACE ( 'NONE', #16643, 16.00000000000000000 ) ;
#36448 = ORIENTED_EDGE ( 'NONE', *, *, #2005, .T. ) ;
#36449 = DIRECTION ( 'NONE',  ( -1.000000000000000000, 0.000000000000000000, -0.000000000000000000 ) ) ;
#36450 = VERTEX_POINT ( 'NONE', #1407 ) ;
#36451 = DIRECTION ( 'NONE',  ( 0.000000000000000000, 0.000000000000000000, -1.000000000000000000 ) ) ;
#36452 = DIRECTION ( 'NONE',  ( -1.000000000000000000, 0.000000000000000000, -0.000000000000000000 ) ) ;
#36453 = CIRCLE ( 'NONE', #2064, 31.99999999999999289 ) ;
#36454 = EDGE_CURVE ( 'NONE', #21714, #17599, #16818, .T. ) ;
#36455 = VERTEX_POINT ( 'NONE', #12659 ) ;
#36456 = VERTEX_POINT ( 'NONE', #31768 ) ;
#36457 = DIRECTION ( 'NONE',  ( 0.000000000000000000, 0.000000000000000000, 1.000000000000000000 ) ) ;
#36458 = DIRECTION ( 'NONE',  ( -1.000000000000000000, -9.814797785686868941E-17, 0.000000000000000000 ) ) ;
#36459 = VERTEX_POINT ( 'NONE', #46685 ) ;
#36460 = ORIENTED_EDGE ( 'NONE', *, *, #19790, .T. ) ;
#36461 = EDGE_CURVE ( 'NONE', #43803, #35290, #48400, .T. ) ;
#36462 = CARTESIAN_POINT ( 'NONE',  ( 11.99999999999999822, -63.18004540533059554, 44.88180994100355292 ) ) ;
#36463 = CARTESIAN_POINT ( 'NONE',  ( 23.41451323550360186, -132.5004227906269989, 5.500000000000000000 ) ) ;
#36464 = DIRECTION ( 'NONE',  ( 0.000000000000000000, -0.9238795325112906243, 0.3826834323650804004 ) ) ;
#36465 = CARTESIAN_POINT ( 'NONE',  ( 5.377855484467702900E-15, 4.693886760319831848E-15, 52.00000000000002132 ) ) ;
#36466 = ADVANCED_FACE ( 'NONE', ( #45709 ), #12468, .T. ) ;
#36467 = PLANE ( 'NONE',  #37224 ) ;
#36468 = VECTOR ( 'NONE', #10888, 1000.000000000000000 ) ;
#36469 = DIRECTION ( 'NONE',  ( 0.000000000000000000, 0.000000000000000000, -1.000000000000000000 ) ) ;
#36470 = DIRECTION ( 'NONE',  ( 0.000000000000000000, 0.000000000000000000, 1.000000000000000000 ) ) ;
#36471 = CARTESIAN_POINT ( 'NONE',  ( 10.00000000000000000, 74.65491531819118620, 23.16904090965733332 ) ) ;
#36472 = CARTESIAN_POINT ( 'NONE',  ( 10.00000000000000000, 37.58145647212455032, -0.6853352020786441789 ) ) ;
#36473 = AXIS2_PLACEMENT_3D ( 'NONE', #19717, #16083, #26371 ) ;
#36474 = CARTESIAN_POINT ( 'NONE',  ( -16.06301359042743115, -102.7814171781257357, 5.500000000000000000 ) ) ;
#36475 = ORIENTED_EDGE ( 'NONE', *, *, #16813, .T. ) ;
#36476 = EDGE_CURVE ( 'NONE', #23651, #25704, #12190, .T. ) ;
#36477 = EDGE_CURVE ( 'NONE', #9793, #29613, #4827, .T. ) ;
#36478 = ORIENTED_EDGE ( 'NONE', *, *, #720, .T. ) ;
#36479 = AXIS2_PLACEMENT_3D ( 'NONE', #4578, #30766, #33940 ) ;
#36480 = EDGE_CURVE ( 'NONE', #13485, #18192, #46434, .T. ) ;
#36481 = LINE ( 'NONE', #43591, #46364 ) ;
#36482 = CARTESIAN_POINT ( 'NONE',  ( 11.99999999999999822, 0.000000000000000000, 0.000000000000000000 ) ) ;
#36483 = VERTEX_POINT ( 'NONE', #8490 ) ;
#36484 = EDGE_CURVE ( 'NONE', #5281, #26444, #15564, .T. ) ;
#36485 = ORIENTED_EDGE ( 'NONE', *, *, #18901, .F. ) ;
#36486 = CIRCLE ( 'NONE', #46681, 16.00000000000000000 ) ;
#36487 = DIRECTION ( 'NONE',  ( 0.000000000000000000, 0.000000000000000000, 1.000000000000000000 ) ) ;
#36488 = DIRECTION ( 'NONE',  ( -1.000000000000000000, 0.000000000000000000, 0.000000000000000000 ) ) ;
#36489 = AXIS2_PLACEMENT_3D ( 'NONE', #5601, #35448, #21231 ) ;
#36490 = ORIENTED_EDGE ( 'NONE', *, *, #507, .F. ) ;
#36491 = DIRECTION ( 'NONE',  ( 0.2867529058022035837, -0.9580045777625452175, 0.000000000000000000 ) ) ;
#36492 = PLANE ( 'NONE',  #46180 ) ;
#36493 = AXIS2_PLACEMENT_3D ( 'NONE', #5974, #27274, #42189 ) ;
#36494 = CARTESIAN_POINT ( 'NONE',  ( 0.000000000000000000, -26.79245525562690844, -32.34446384430000876 ) ) ;
#36495 = ORIENTED_EDGE ( 'NONE', *, *, #45697, .F. ) ;
#36496 = CARTESIAN_POINT ( 'NONE',  ( 35.50000000000000711, -120.0000000000000000, -5.500000000000000000 ) ) ;
#36497 = ORIENTED_EDGE ( 'NONE', *, *, #32760, .T. ) ;
#36498 = CARTESIAN_POINT ( 'NONE',  ( 0.000000000000000000, 29.81001611431009479, 22.74946021919143391 ) ) ;
#36499 = ORIENTED_EDGE ( 'NONE', *, *, #8151, .F. ) ;
#36500 = DIRECTION ( 'NONE',  ( -1.000000000000000000, 0.000000000000000000, -0.000000000000000000 ) ) ;
#36501 = ORIENTED_EDGE ( 'NONE', *, *, #12184, .F. ) ;
#36502 = DIRECTION ( 'NONE',  ( 0.000000000000000000, -0.7431448254773870277, -0.6691306063588662312 ) ) ;
#36503 = CARTESIAN_POINT ( 'NONE',  ( 10.00000000000000000, 73.44644590900094272, -24.73286445877628026 ) ) ;
#36504 = CIRCLE ( 'NONE', #21669, 42.00000000000000000 ) ;
#36506 = VERTEX_POINT ( 'NONE', #5076 ) ;
#36505 = CARTESIAN_POINT ( 'NONE',  ( 5.000000000000000000, 67.80270845531887858, 46.11716303203210998 ) ) ;
#36507 = CYLINDRICAL_SURFACE ( 'NONE', #28570, 16.00000000000000000 ) ;
#36508 = ORIENTED_EDGE ( 'NONE', *, *, #22634, .T. ) ;
#36509 = CARTESIAN_POINT ( 'NONE',  ( 6.000000000000000000, -78.73519480814971416, 22.90783923731599359 ) ) ;
#36510 = ORIENTED_EDGE ( 'NONE', *, *, #31936, .T. ) ;
#36511 = EDGE_LOOP ( 'NONE', ( #26884, #23182, #8372, #16582 ) ) ;
#36512 = CARTESIAN_POINT ( 'NONE',  ( 10.00000000000000000, -32.34446384429951138, -26.79245525562750530 ) ) ;
#36513 = FACE_OUTER_BOUND ( 'NONE', #23681, .T. ) ;
#36514 = ADVANCED_FACE ( 'NONE', ( #19991 ), #16329, .T. ) ;
#36515 = DIRECTION ( 'NONE',  ( -1.000000000000000000, 0.000000000000000000, 0.000000000000000000 ) ) ;
#36516 = LINE ( 'NONE', #28925, #36000 ) ;
#36517 = DIRECTION ( 'NONE',  ( 1.000000000000000000, 0.000000000000000000, 0.000000000000000000 ) ) ;
#36518 = VERTEX_POINT ( 'NONE', #6280 ) ;
#36519 = EDGE_CURVE ( 'NONE', #47062, #20918, #20963, .T. ) ;
#36520 = CARTESIAN_POINT ( 'NONE',  ( 0.000000000000000000, 0.000000000000000000, 0.000000000000000000 ) ) ;
#36521 = ADVANCED_FACE ( 'NONE', ( #10181 ), #14339, .T. ) ;
#36522 = DIRECTION ( 'NONE',  ( -1.000000000000000000, 0.000000000000000000, -0.000000000000000000 ) ) ;
#36523 = EDGE_CURVE ( 'NONE', #34646, #16565, #2287, .T. ) ;
#36524 = CARTESIAN_POINT ( 'NONE',  ( 11.59999999999999787, 1.420590287010929336E-15, -56.19999999999998863 ) ) ;
#36525 = CIRCLE ( 'NONE', #574, 31.99999999999998579 ) ;
#36526 = EDGE_LOOP ( 'NONE', ( #13318, #35069, #19046, #28733 ) ) ;
#36527 = EDGE_CURVE ( 'NONE', #4758, #14404, #24957, .T. ) ;
#36528 = DIRECTION ( 'NONE',  ( -1.000000000000000000, -0.000000000000000000, -0.000000000000000000 ) ) ;
#36530 = EDGE_CURVE ( 'NONE', #45738, #461, #35891, .T. ) ;
#36529 = CARTESIAN_POINT ( 'NONE',  ( 12.00000000000000000, -22.32062822937469093, 14.36278369418830181 ) ) ;
#36531 = CARTESIAN_POINT ( 'NONE',  ( 0.000000000000000000, 16.83928648764945279, -16.46020748918028076 ) ) ;
#36532 = CARTESIAN_POINT ( 'NONE',  ( -35.37301231164799731, -117.0000000000000000, 2.500000000000000000 ) ) ;
#36533 = CIRCLE ( 'NONE', #30295, 82.00000000000000000 ) ;
#36534 = CARTESIAN_POINT ( 'NONE',  ( 11.99999999999999822, -68.55367621811110723, -44.99326035066126650 ) ) ;
#36535 = CARTESIAN_POINT ( 'NONE',  ( 15.00000000000000000, -25.60904388321916159, 6.976881207771517879 ) ) ;
#36536 = FACE_OUTER_BOUND ( 'NONE', #24997, .T. ) ;
#36537 = CARTESIAN_POINT ( 'NONE',  ( 0.000000000000000000, 72.35432306680455383, 20.40083707023012494 ) ) ;
#36538 = ORIENTED_EDGE ( 'NONE', *, *, #4644, .F. ) ;
#36539 = ORIENTED_EDGE ( 'NONE', *, *, #30432, .F. ) ;
#36540 = CARTESIAN_POINT ( 'NONE',  ( -10.00000000000000000, 0.000000000000000000, 0.000000000000000000 ) ) ;
#36541 = VECTOR ( 'NONE', #8587, 999.9999999999998863 ) ;
#36542 = ORIENTED_EDGE ( 'NONE', *, *, #18718, .F. ) ;
#36543 = EDGE_CURVE ( 'NONE', #7024, #29160, #37471, .T. ) ;
#36544 = CARTESIAN_POINT ( 'NONE',  ( -10.90473778262209414, 0.000000000000000000, 0.000000000000000000 ) ) ;
#36545 = DIRECTION ( 'NONE',  ( 0.9937460003578419965, -0.1116641696014989971, 2.775557561562891351E-17 ) ) ;
#36546 = CARTESIAN_POINT ( 'NONE',  ( 0.000000000000000000, -55.38113227695743745, -54.21277698773734244 ) ) ;
#36547 = EDGE_LOOP ( 'NONE', ( #31665, #30822, #10545, #46526 ) ) ;
#36548 = CIRCLE ( 'NONE', #15452, 82.00000000000000000 ) ;
#36549 = EDGE_CURVE ( 'NONE', #20800, #22705, #47851, .T. ) ;
#36550 = FACE_OUTER_BOUND ( 'NONE', #38310, .T. ) ;
#36551 = ORIENTED_EDGE ( 'NONE', *, *, #22343, .T. ) ;
#36552 = ORIENTED_EDGE ( 'NONE', *, *, #32056, .T. ) ;
#36553 = DIRECTION ( 'NONE',  ( 1.000000000000000000, 0.000000000000000000, 0.000000000000000000 ) ) ;
#36554 = VERTEX_POINT ( 'NONE', #17763 ) ;
#36555 = DIRECTION ( 'NONE',  ( -0.9827303690289279636, -0.1850432970638682117, 0.000000000000000000 ) ) ;
#36556 = DIRECTION ( 'NONE',  ( -0.3853207896976523772, 0.9227826878668550226, 0.000000000000000000 ) ) ;
#36557 = ORIENTED_EDGE ( 'NONE', *, *, #5021, .F. ) ;
#36559 = AXIS2_PLACEMENT_3D ( 'NONE', #32009, #28084, #16340 ) ;
#36558 = DIRECTION ( 'NONE',  ( -1.000000000000000000, 0.000000000000000000, -0.000000000000000000 ) ) ;
#36560 = ORIENTED_EDGE ( 'NONE', *, *, #23426, .T. ) ;
#36561 = LINE ( 'NONE', #33133, #678 ) ;
#36562 = DIRECTION ( 'NONE',  ( 0.000000000000000000, -0.1045284632676436454, -0.9945218953682744001 ) ) ;
#36563 = CARTESIAN_POINT ( 'NONE',  ( 10.00000000000000000, -17.67226234102849958, 33.17418723428301774 ) ) ;
#36564 = EDGE_CURVE ( 'NONE', #39485, #33288, #6512, .T. ) ;
#36565 = ORIENTED_EDGE ( 'NONE', *, *, #7779, .T. ) ;
#36566 = CARTESIAN_POINT ( 'NONE',  ( 10.00000000000000000, -44.88180994100421373, 63.18004540533011948 ) ) ;
#36567 = ORIENTED_EDGE ( 'NONE', *, *, #38632, .F. ) ;
#36568 = ORIENTED_EDGE ( 'NONE', *, *, #20944, .F. ) ;
#36569 = EDGE_CURVE ( 'NONE', #47625, #7708, #11655, .T. ) ;
#36570 = FACE_OUTER_BOUND ( 'NONE', #47054, .T. ) ;
#36571 = CARTESIAN_POINT ( 'NONE',  ( -10.00000000000000000, 0.000000000000000000, 0.000000000000000000 ) ) ;
#36572 = FACE_OUTER_BOUND ( 'NONE', #26141, .T. ) ;
#36573 = DIRECTION ( 'NONE',  ( -1.000000000000000000, -0.000000000000000000, 0.000000000000000000 ) ) ;
#36574 = VERTEX_POINT ( 'NONE', #36374 ) ;
#36575 = EDGE_CURVE ( 'NONE', #37777, #18965, #30458, .T. ) ;
#36577 = PLANE ( 'NONE',  #40936 ) ;
#36576 = PRESENTATION_LAYER_ASSIGNMENT (  '', '', ( #13251 ) ) ;
#36578 = DIRECTION ( 'NONE',  ( -1.000000000000000000, 0.000000000000000000, 0.000000000000000000 ) ) ;
#36579 = EDGE_CURVE ( 'NONE', #2845, #26639, #4661, .T. ) ;
#36580 = CYLINDRICAL_SURFACE ( 'NONE', #31678, 37.49900000000000233 ) ;
#36581 = AXIS2_PLACEMENT_3D ( 'NONE', #5037, #862, #15809 ) ;
#36582 = LINE ( 'NONE', #37313, #17333 ) ;
#36583 = CARTESIAN_POINT ( 'NONE',  ( 0.000000000000000000, 75.11764819372149304, 29.05362095685338986 ) ) ;
#36584 = ORIENTED_EDGE ( 'NONE', *, *, #27250, .F. ) ;
#36586 = EDGE_CURVE ( 'NONE', #3154, #22090, #21681, .T. ) ;
#36585 = DIRECTION ( 'NONE',  ( 1.000000000000000000, 0.000000000000000000, 0.000000000000000000 ) ) ;
#36587 = CARTESIAN_POINT ( 'NONE',  ( 0.000000000000000000, 71.27951684758068041, -30.41916302227036439 ) ) ;
#36588 = CARTESIAN_POINT ( 'NONE',  ( 11.99999999999999822, 50.95692526931329525, 58.39081064771768581 ) ) ;
#36589 = CARTESIAN_POINT ( 'NONE',  ( 0.000000000000000000, 0.000000000000000000, 0.000000000000000000 ) ) ;
#36590 = AXIS2_PLACEMENT_3D ( 'NONE', #42360, #5894, #46039 ) ;
#36591 = CARTESIAN_POINT ( 'NONE',  ( 10.00000000000000000, -34.94270380257693631, 74.18225833017875459 ) ) ;
#36592 = DIRECTION ( 'NONE',  ( -1.000000000000000000, 0.000000000000000000, -0.000000000000000000 ) ) ;
#36593 = ORIENTED_EDGE ( 'NONE', *, *, #23476, .T. ) ;
#36594 = CYLINDRICAL_SURFACE ( 'NONE', #17584, 77.49899999999999523 ) ;
#36595 = VECTOR ( 'NONE', #43584, 1000.000000000000000 ) ;
#36596 = AXIS2_PLACEMENT_3D ( 'NONE', #20480, #9464, #46444 ) ;
#36597 = CYLINDRICAL_SURFACE ( 'NONE', #38493, 77.49899999999999523 ) ;
#36598 = ORIENTED_EDGE ( 'NONE', *, *, #46431, .F. ) ;
#36599 = VERTEX_POINT ( 'NONE', #32689 ) ;
#36600 = DIRECTION ( 'NONE',  ( -1.000000000000000000, -0.000000000000000000, -0.000000000000000000 ) ) ;
#36601 = AXIS2_PLACEMENT_3D ( 'NONE', #26265, #45104, #33828 ) ;
#36602 = VERTEX_POINT ( 'NONE', #47614 ) ;
#36603 = CIRCLE ( 'NONE', #46798, 82.00000000000000000 ) ;
#36604 = ORIENTED_EDGE ( 'NONE', *, *, #25728, .T. ) ;
#36605 = DIRECTION ( 'NONE',  ( 0.000000000000000000, 0.000000000000000000, 1.000000000000000000 ) ) ;
#36606 = DIRECTION ( 'NONE',  ( 0.000000000000000000, 0.000000000000000000, 1.000000000000000000 ) ) ;
#36608 = ORIENTED_EDGE ( 'NONE', *, *, #7463, .T. ) ;
#36607 = FACE_OUTER_BOUND ( 'NONE', #6400, .T. ) ;
#36609 = ORIENTED_EDGE ( 'NONE', *, *, #27886, .T. ) ;
#36610 = CARTESIAN_POINT ( 'NONE',  ( 11.99999999999999822, -29.01471420065616513, 76.69515212746006227 ) ) ;
#36611 = ORIENTED_EDGE ( 'NONE', *, *, #1548, .T. ) ;
#36612 = ORIENTED_EDGE ( 'NONE', *, *, #8493, .F. ) ;
#36613 = ORIENTED_EDGE ( 'NONE', *, *, #17949, .F. ) ;
#36614 = CARTESIAN_POINT ( 'NONE',  ( 11.99999999999999822, 8.840884882375075193, 74.65374052328651544 ) ) ;
#36615 = DIRECTION ( 'NONE',  ( 0.000000000000000000, -0.4539904997395540764, 0.8910065241883642351 ) ) ;
#36616 = EDGE_CURVE ( 'NONE', #47158, #18503, #32044, .T. ) ;
#36617 = CARTESIAN_POINT ( 'NONE',  ( 12.00000000000000000, -14.54903810567676636, -22.19967320028756674 ) ) ;
#36618 = ORIENTED_EDGE ( 'NONE', *, *, #13912, .T. ) ;
#36619 = ORIENTED_EDGE ( 'NONE', *, *, #3871, .F. ) ;
#36620 = ORIENTED_EDGE ( 'NONE', *, *, #21698, .T. ) ;
#36621 = CARTESIAN_POINT ( 'NONE',  ( 0.000000000000000000, 33.17418723428307459, 17.67226234102837878 ) ) ;
#36622 = ORIENTED_EDGE ( 'NONE', *, *, #44583, .F. ) ;
#36623 = EDGE_CURVE ( 'NONE', #29380, #24346, #2584, .T. ) ;
#36624 = DIRECTION ( 'NONE',  ( 0.000000000000000000, -0.7604059656000369261, 0.6494480483301766638 ) ) ;
#36625 = CIRCLE ( 'NONE', #33550, 31.99999999999998579 ) ;
#36626 = CARTESIAN_POINT ( 'NONE',  ( -18.24502636017238899, -100.7225776329765665, 5.500000000000000000 ) ) ;
#36627 = FACE_BOUND ( 'NONE', #24602, .T. ) ;
#36628 = ORIENTED_EDGE ( 'NONE', *, *, #8655, .T. ) ;
#36629 = CARTESIAN_POINT ( 'NONE',  ( 10.00000000000000000, -37.58145647212455032, 0.6853352020789044152 ) ) ;
#36630 = EDGE_CURVE ( 'NONE', #16364, #25709, #1568, .T. ) ;
#36631 = DIRECTION ( 'NONE',  ( -1.000000000000000000, 0.000000000000000000, 0.000000000000000000 ) ) ;
#36632 = CIRCLE ( 'NONE', #10048, 12.49999999999999645 ) ;
#36633 = CARTESIAN_POINT ( 'NONE',  ( 0.000000000000000000, 23.50000000000000000, -1.500000000000001332 ) ) ;
#36635 = ADVANCED_FACE ( 'NONE', ( #36123 ), #24870, .F. ) ;
#36634 = DIRECTION ( 'NONE',  ( -0.000000000000000000, -0.000000000000000000, 1.000000000000000000 ) ) ;
#36636 = DIRECTION ( 'NONE',  ( -1.000000000000000000, -0.000000000000000000, -0.000000000000000000 ) ) ;
#36637 = ORIENTED_EDGE ( 'NONE', *, *, #187, .T. ) ;
#36639 = EDGE_CURVE ( 'NONE', #12152, #46530, #29019, .T. ) ;
#36638 = CARTESIAN_POINT ( 'NONE',  ( 1.384174031800307736, -119.4220188154534981, -2.500000000000000000 ) ) ;
#36640 = VERTEX_POINT ( 'NONE', #43238 ) ;
#36641 = CARTESIAN_POINT ( 'NONE',  ( 0.000000000000000000, 0.000000000000000000, 0.000000000000000000 ) ) ;
#36642 = ADVANCED_FACE ( 'NONE', ( #24637 ), #13869, .T. ) ;
#36643 = DIRECTION ( 'NONE',  ( 0.000000000000000000, 0.3090169943749412895, 0.9510565162951556406 ) ) ;
#36644 = DIRECTION ( 'NONE',  ( -1.000000000000000000, 0.000000000000000000, -0.000000000000000000 ) ) ;
#36645 = FACE_OUTER_BOUND ( 'NONE', #17594, .T. ) ;
#36646 = CARTESIAN_POINT ( 'NONE',  ( 0.000000000000000000, 0.000000000000000000, 0.000000000000000000 ) ) ;
#36647 = LINE ( 'NONE', #6324, #29457 ) ;
#36648 = DIRECTION ( 'NONE',  ( -1.000000000000000000, 0.000000000000000000, -0.000000000000000000 ) ) ;
#36649 =( REPRESENTATION_RELATIONSHIP ('NONE','NONE', #5957, #1226 ) REPRESENTATION_RELATIONSHIP_WITH_TRANSFORMATION ( #15721 )SHAPE_REPRESENTATION_RELATIONSHIP( ) );
#36650 = PLANE ( 'NONE',  #30794 ) ;
#36651 = DIRECTION ( 'NONE',  ( -1.000000000000000000, 0.000000000000000000, 0.000000000000000000 ) ) ;
#36652 = ORIENTED_EDGE ( 'NONE', *, *, #13036, .T. ) ;
#36653 = ORIENTED_EDGE ( 'NONE', *, *, #13978, .T. ) ;
#36654 = VECTOR ( 'NONE', #32054, 1000.000000000000000 ) ;
#36655 = ORIENTED_EDGE ( 'NONE', *, *, #39348, .F. ) ;
#36656 = VECTOR ( 'NONE', #20468, 1000.000000000000114 ) ;
#36657 = AXIS2_PLACEMENT_3D ( 'NONE', #23399, #37853, #11913 ) ;
#36658 = CYLINDRICAL_SURFACE ( 'NONE', #41323, 16.00000000000000000 ) ;
#36659 = DIRECTION ( 'NONE',  ( 0.000000000000000000, 0.000000000000000000, 1.000000000000000000 ) ) ;
#36660 = CIRCLE ( 'NONE', #19429, 15.99999999999999645 ) ;
#36661 = ORIENTED_EDGE ( 'NONE', *, *, #19379, .T. ) ;
#36662 = ADVANCED_FACE ( 'NONE', ( #37091 ), #15318, .F. ) ;
#36663 = CARTESIAN_POINT ( 'NONE',  ( 0.000000000000000000, 20.41045688087930898, -72.35160999960793049 ) ) ;
#36664 = EDGE_CURVE ( 'NONE', #22222, #9352, #737, .T. ) ;
#36665 = ORIENTED_EDGE ( 'NONE', *, *, #44154, .F. ) ;
#36666 = ORIENTED_EDGE ( 'NONE', *, *, #28074, .F. ) ;
#36667 = ADVANCED_FACE ( 'NONE', ( #41023 ), #22413, .T. ) ;
#36668 = PRESENTATION_LAYER_ASSIGNMENT (  '', '', ( #14013 ) ) ;
#36669 = CARTESIAN_POINT ( 'NONE',  ( 0.000000000000000000, 9.188173127307898369, -40.98264845739739570 ) ) ;
#36670 = ORIENTED_EDGE ( 'NONE', *, *, #32508, .T. ) ;
#36671 = DIRECTION ( 'NONE',  ( 1.000000000000000000, -0.000000000000000000, -0.000000000000000000 ) ) ;
#36672 = ORIENTED_EDGE ( 'NONE', *, *, #9565, .F. ) ;
#36673 = ORIENTED_EDGE ( 'NONE', *, *, #26139, .F. ) ;
#36674 = DIRECTION ( 'NONE',  ( 0.000000000000000000, 0.000000000000000000, 1.000000000000000000 ) ) ;
#36675 = CARTESIAN_POINT ( 'NONE',  ( 11.99999999999999822, 39.78640506895698792, -66.50666863321958999 ) ) ;
#36676 = EDGE_CURVE ( 'NONE', #5880, #12261, #7711, .T. ) ;
#36677 = FACE_OUTER_BOUND ( 'NONE', #44976, .T. ) ;
#36678 = ORIENTED_EDGE ( 'NONE', *, *, #46257, .F. ) ;
#36679 = EDGE_CURVE ( 'NONE', #32425, #38732, #42967, .T. ) ;
#36680 = ADVANCED_FACE ( 'NONE', ( #4050 ), #22881, .T. ) ;
#36681 = EDGE_LOOP ( 'NONE', ( #26396, #20535, #24402, #20478 ) ) ;
#36682 = CARTESIAN_POINT ( 'NONE',  ( 10.00000000000000000, 0.000000000000000000, 0.000000000000000000 ) ) ;
#36683 = CARTESIAN_POINT ( 'NONE',  ( 23.11608002360578240, -124.4885236261218182, 5.500000000000000000 ) ) ;
#36684 = EDGE_LOOP ( 'NONE', ( #47097, #40373, #5578, #12129 ) ) ;
#36685 = AXIS2_PLACEMENT_3D ( 'NONE', #44443, #39820, #17526 ) ;
#36686 = ORIENTED_EDGE ( 'NONE', *, *, #25464, .F. ) ;
#36687 = CARTESIAN_POINT ( 'NONE',  ( 12.69589495141918611, -96.69089767102708777, 5.500000000000000000 ) ) ;
#36688 = CARTESIAN_POINT ( 'NONE',  ( 11.99999999999999822, 68.67312586195046720, -35.91791733033404199 ) ) ;
#36689 = ORIENTED_EDGE ( 'NONE', *, *, #33534, .F. ) ;
#36690 = ORIENTED_EDGE ( 'NONE', *, *, #20213, .F. ) ;
#36691 = AXIS2_PLACEMENT_3D ( 'NONE', #18717, #10907, #33651 ) ;
#36692 = LINE ( 'NONE', #24732, #16792 ) ;
#36693 = CARTESIAN_POINT ( 'NONE',  ( 0.000000000000000000, -35.53030884539077050, -12.26510123303296851 ) ) ;
#36694 = DIRECTION ( 'NONE',  ( 0.000000000000000000, 0.000000000000000000, 1.000000000000000000 ) ) ;
#36695 = DIRECTION ( 'NONE',  ( 0.000000000000000000, 0.000000000000000000, 1.000000000000000000 ) ) ;
#36696 = DIRECTION ( 'NONE',  ( 0.000000000000000000, 0.000000000000000000, -1.000000000000000000 ) ) ;
#36697 = ADVANCED_FACE ( 'NONE', ( #11876 ), #18953, .T. ) ;
#36698 = CARTESIAN_POINT ( 'NONE',  ( 11.99999999999999822, 0.000000000000000000, 0.000000000000000000 ) ) ;
#36699 = CARTESIAN_POINT ( 'NONE',  ( 0.000000000000000000, 59.03961581697399907, 46.53671651293969802 ) ) ;
#36700 = AXIS2_PLACEMENT_3D ( 'NONE', #18914, #22603, #43259 ) ;
#36701 = DIRECTION ( 'NONE',  ( -1.000000000000000000, 0.000000000000000000, 0.000000000000000000 ) ) ;
#36702 = DIRECTION ( 'NONE',  ( -1.000000000000000000, -0.000000000000000000, -0.000000000000000000 ) ) ;
#36703 = DIRECTION ( 'NONE',  ( -1.000000000000000000, 0.000000000000000000, 0.000000000000000000 ) ) ;
#36704 =( NAMED_UNIT ( * ) SI_UNIT ( $, .STERADIAN. ) SOLID_ANGLE_UNIT ( ) );
#36705 = DIRECTION ( 'NONE',  ( -1.000000000000000000, 0.000000000000000000, 0.000000000000000000 ) ) ;
#36706 = VERTEX_POINT ( 'NONE', #29509 ) ;
#36707 = ORIENTED_EDGE ( 'NONE', *, *, #47304, .F. ) ;
#36708 = EDGE_LOOP ( 'NONE', ( #20855, #23005, #34428, #42220 ) ) ;
#36709 = CARTESIAN_POINT ( 'NONE',  ( 10.00000000000000000, 0.000000000000000000, 0.000000000000000000 ) ) ;
#36710 = VERTEX_POINT ( 'NONE', #370 ) ;
#36711 = CYLINDRICAL_SURFACE ( 'NONE', #14393, 82.00000000000000000 ) ;
#36712 = ORIENTED_EDGE ( 'NONE', *, *, #9064, .T. ) ;
#36713 = VECTOR ( 'NONE', #40311, 1000.000000000000114 ) ;
#36714 = EDGE_CURVE ( 'NONE', #20645, #7437, #48343, .T. ) ;
#36715 = AXIS2_PLACEMENT_3D ( 'NONE', #18903, #45117, #23078 ) ;
#36716 = DIRECTION ( 'NONE',  ( -0.000000000000000000, -0.000000000000000000, -1.000000000000000000 ) ) ;
#36717 = ORIENTED_EDGE ( 'NONE', *, *, #44541, .F. ) ;
#36718 = CARTESIAN_POINT ( 'NONE',  ( 0.000000000000000000, 0.000000000000000000, -56.19999999999998863 ) ) ;
#36720 = EDGE_CURVE ( 'NONE', #11808, #11292, #11634, .T. ) ;
#36719 = CIRCLE ( 'NONE', #43000, 31.99999999999999645 ) ;
#36721 = ORIENTED_EDGE ( 'NONE', *, *, #34982, .T. ) ;
#36722 = ORIENTED_EDGE ( 'NONE', *, *, #35555, .F. ) ;
#36723 = PLANE ( 'NONE',  #2349 ) ;
#36724 = ADVANCED_FACE ( 'NONE', ( #44675 ), #29991, .T. ) ;
#36725 = AXIS2_PLACEMENT_3D ( 'NONE', #16304, #5292, #46653 ) ;
#36726 = CARTESIAN_POINT ( 'NONE',  ( 0.000000000000000000, 72.35432306680455383, 20.40083707023012494 ) ) ;
#36727 = AXIS2_PLACEMENT_3D ( 'NONE', #42118, #37964, #19349 ) ;
#36728 = ORIENTED_EDGE ( 'NONE', *, *, #30793, .F. ) ;
#36729 = DIRECTION ( 'NONE',  ( -0.000000000000000000, -0.000000000000000000, -1.000000000000000000 ) ) ;
#36730 = ORIENTED_EDGE ( 'NONE', *, *, #32466, .T. ) ;
#36731 = DIRECTION ( 'NONE',  ( 0.000000000000000000, -0.9510565162951500895, -0.3090169943749583314 ) ) ;
#36732 = FACE_OUTER_BOUND ( 'NONE', #35472, .T. ) ;
#36733 = VERTEX_POINT ( 'NONE', #8201 ) ;
#36734 = EDGE_CURVE ( 'NONE', #43358, #16571, #5437, .T. ) ;
#36735 = FACE_OUTER_BOUND ( 'NONE', #23544, .T. ) ;
#36736 = DIRECTION ( 'NONE',  ( 0.000000000000000000, 0.000000000000000000, 1.000000000000000000 ) ) ;
#36737 = EDGE_CURVE ( 'NONE', #33784, #26631, #10914, .T. ) ;
#36738 = CARTESIAN_POINT ( 'NONE',  ( 11.99999999999999822, 0.000000000000000000, 0.000000000000000000 ) ) ;
#36739 = CARTESIAN_POINT ( 'NONE',  ( 11.99999999999999822, 0.000000000000000000, 0.000000000000000000 ) ) ;
#36740 = VERTEX_POINT ( 'NONE', #26073 ) ;
#36741 = DIRECTION ( 'NONE',  ( 0.000000000000000000, 0.000000000000000000, 1.000000000000000000 ) ) ;
#36742 = ORIENTED_EDGE ( 'NONE', *, *, #38291, .T. ) ;
#36743 = ORIENTED_EDGE ( 'NONE', *, *, #28280, .F. ) ;
#36744 = PLANE ( 'NONE',  #39277 ) ;
#36745 = DIRECTION ( 'NONE',  ( 0.000000000000000000, 0.000000000000000000, 1.000000000000000000 ) ) ;
#36746 = EDGE_LOOP ( 'NONE', ( #3635, #11464, #44352, #29633 ) ) ;
#36747 = CARTESIAN_POINT ( 'NONE',  ( 0.000000000000000000, 41.76106447765580043, -62.50884508063379741 ) ) ;
#36748 = CARTESIAN_POINT ( 'NONE',  ( 10.00000000000000000, 0.000000000000000000, 0.000000000000000000 ) ) ;
#36749 = PLANE ( 'NONE',  #33648 ) ;
#36750 = ORIENTED_EDGE ( 'NONE', *, *, #5543, .T. ) ;
#36751 = CARTESIAN_POINT ( 'NONE',  ( 0.000000000000000000, 0.000000000000000000, 125.0000000000000000 ) ) ;
#36752 = DIRECTION ( 'NONE',  ( -0.7585478161175716050, -0.6516173805718067369, 0.000000000000000000 ) ) ;
#36753 = ADVANCED_FACE ( 'NONE', ( #34139 ), #33182, .T. ) ;
#36755 = AXIS2_PLACEMENT_3D ( 'NONE', #380, #19938, #18963 ) ;
#36754 = CARTESIAN_POINT ( 'NONE',  ( 10.00000000000000000, 63.18004540533092239, -44.88180994100307686 ) ) ;
#36756 = VERTEX_POINT ( 'NONE', #37335 ) ;
#36757 = VECTOR ( 'NONE', #28686, 1000.000000000000000 ) ;
#36758 = CARTESIAN_POINT ( 'NONE',  ( 0.000000000000000000, -27.75498641678720446, -31.52238457039628727 ) ) ;
#36759 = CARTESIAN_POINT ( 'NONE',  ( 3.469446951953614189E-15, 12.79999999999999893, 0.000000000000000000 ) ) ;
#36760 = CYLINDRICAL_SURFACE ( 'NONE', #17745, 82.00000000000000000 ) ;
#36761 = CARTESIAN_POINT ( 'NONE',  ( 10.00000000000000000, 6.736453364083557105, 36.88895765772635826 ) ) ;
#36762 = AXIS2_PLACEMENT_3D ( 'NONE', #36095, #22126, #25073 ) ;
#36763 = AXIS2_PLACEMENT_3D ( 'NONE', #7606, #22536, #37465 ) ;
#36764 = FACE_OUTER_BOUND ( 'NONE', #21168, .T. ) ;
#36765 = CARTESIAN_POINT ( 'NONE',  ( -10.00000000000000000, 0.000000000000000000, 0.000000000000000000 ) ) ;
#36766 = CARTESIAN_POINT ( 'NONE',  ( 0.000000000000000000, 75.16055320797030959, 18.89407956138283851 ) ) ;
#36767 = LINE ( 'NONE', #22575, #47548 ) ;
#36768 = CIRCLE ( 'NONE', #45365, 31.99999999999999289 ) ;
#36769 = CIRCLE ( 'NONE', #25822, 77.49900000000000944 ) ;
#36770 = ORIENTED_EDGE ( 'NONE', *, *, #28674, .F. ) ;
#36771 = DIRECTION ( 'NONE',  ( 0.000000000000000000, 0.000000000000000000, -1.000000000000000000 ) ) ;
#36772 = AXIS2_PLACEMENT_3D ( 'NONE', #36915, #3147, #33008 ) ;
#36773 = ORIENTED_EDGE ( 'NONE', *, *, #42534, .T. ) ;
#36774 = CARTESIAN_POINT ( 'NONE',  ( 0.000000000000000000, 73.73191006444551476, 14.66109333815590254 ) ) ;
#36775 = CARTESIAN_POINT ( 'NONE',  ( 0.000000000000000000, -120.0000000000000000, 42.00000000000000000 ) ) ;
#36776 = LINE ( 'NONE', #14275, #12020 ) ;
#36777 = ORIENTED_EDGE ( 'NONE', *, *, #43004, .T. ) ;
#36778 = DIRECTION ( 'NONE',  ( 0.000000000000000000, 0.07845909572783793529, 0.9969173337331285190 ) ) ;
#36779 = EDGE_CURVE ( 'NONE', #22693, #39455, #26567, .T. ) ;
#36780 = ORIENTED_EDGE ( 'NONE', *, *, #36195, .T. ) ;
#36781 = ORIENTED_EDGE ( 'NONE', *, *, #2930, .F. ) ;
#36782 = EDGE_CURVE ( 'NONE', #47457, #3764, #15062, .T. ) ;
#36783 = VECTOR ( 'NONE', #44651, 1000.000000000000000 ) ;
#36784 = DIRECTION ( 'NONE',  ( 0.9781476007338069101, 0.000000000000000000, -0.2079116908177528755 ) ) ;
#36785 = CIRCLE ( 'NONE', #4764, 31.99999999999999289 ) ;
#36786 = EDGE_CURVE ( 'NONE', #15331, #22290, #47277, .T. ) ;
#36787 = CARTESIAN_POINT ( 'NONE',  ( 10.00000000000000000, -3.894527615418464705, 81.90746397400387480 ) ) ;
#36788 = CARTESIAN_POINT ( 'NONE',  ( 15.00000000000000000, -0.9646360437372099028, 23.52805723605590771 ) ) ;
#36789 = AXIS2_PLACEMENT_3D ( 'NONE', #22612, #26294, #37784 ) ;
#36790 = CIRCLE ( 'NONE', #15707, 77.49900000000002365 ) ;
#36791 = ORIENTED_EDGE ( 'NONE', *, *, #19661, .F. ) ;
#36792 = DIRECTION ( 'NONE',  ( 0.000000000000000000, 0.000000000000000000, 1.000000000000000000 ) ) ;
#36793 = ORIENTED_EDGE ( 'NONE', *, *, #4576, .T. ) ;
#36794 = AXIS2_PLACEMENT_3D ( 'NONE', #29646, #26227, #41169 ) ;
#36795 = CARTESIAN_POINT ( 'NONE',  ( 0.000000000000000000, 51.03279382321166224, -55.19960302592011914 ) ) ;
#36796 = CARTESIAN_POINT ( 'NONE',  ( 10.00000000000000000, -29.81001611430991360, -22.74946021919165418 ) ) ;
#36797 = ADVANCED_FACE ( 'NONE', ( #24515 ), #5435, .T. ) ;
#36798 = AXIS2_PLACEMENT_3D ( 'NONE', #46047, #31123, #12515 ) ;
#36799 = CARTESIAN_POINT ( 'NONE',  ( 10.00000000000000000, -35.92658777277502935, -10.74501242461320594 ) ) ;
#36800 = DIRECTION ( 'NONE',  ( -1.000000000000000000, 0.000000000000000000, 0.000000000000000000 ) ) ;
#36801 = ORIENTED_EDGE ( 'NONE', *, *, #35614, .T. ) ;
#36802 = VECTOR ( 'NONE', #42069, 1000.000000000000000 ) ;
#36803 = DIRECTION ( 'NONE',  ( -1.000000000000000000, 0.000000000000000000, 0.000000000000000000 ) ) ;
#36804 = ORIENTED_EDGE ( 'NONE', *, *, #11746, .T. ) ;
#36805 = VERTEX_POINT ( 'NONE', #46562 ) ;
#36806 = ADVANCED_FACE ( 'NONE', ( #19436 ), #17392, .T. ) ;
#36807 = CARTESIAN_POINT ( 'NONE',  ( 0.000000000000000000, 0.000000000000000000, 0.000000000000000000 ) ) ;
#36808 = LINE ( 'NONE', #21401, #19920 ) ;
#36809 = CARTESIAN_POINT ( 'NONE',  ( 10.00000000000000000, -68.67312586195023982, 35.91791733033450384 ) ) ;
#36810 = CARTESIAN_POINT ( 'NONE',  ( 11.99999999999999822, 36.73666225445988687, -65.58780272294035285 ) ) ;
#36811 = ORIENTED_EDGE ( 'NONE', *, *, #42708, .T. ) ;
#36812 = CARTESIAN_POINT ( 'NONE',  ( 0.000000000000000000, 0.000000000000000000, 0.000000000000000000 ) ) ;
#36813 = CARTESIAN_POINT ( 'NONE',  ( -12.50000000000000000, -107.5000000000000000, 40.00000000000000000 ) ) ;
#36814 = CARTESIAN_POINT ( 'NONE',  ( -23.97194136764370498, -131.3950000906648938, -5.500000000000000000 ) ) ;
#36815 = LINE ( 'NONE', #40738, #1738 ) ;
#36816 = ADVANCED_FACE ( 'NONE', ( #35282 ), #15787, .T. ) ;
#36817 = CARTESIAN_POINT ( 'NONE',  ( 0.000000000000000000, -77.32052557432845674, 5.256550761632577284 ) ) ;
#36818 = EDGE_LOOP ( 'NONE', ( #19883, #41527, #39547, #20309 ) ) ;
#36819 = CARTESIAN_POINT ( 'NONE',  ( 12.00000000000000000, 14.60985201121703980, -18.46759930825707841 ) ) ;
#36820 = DIRECTION ( 'NONE',  ( -0.6862798483830533369, -0.7273375899149812085, 0.000000000000000000 ) ) ;
#36821 = FACE_OUTER_BOUND ( 'NONE', #42327, .T. ) ;
#36822 = LINE ( 'NONE', #3288, #1232 ) ;
#36823 = CIRCLE ( 'NONE', #7894, 11.59999999999999787 ) ;
#36824 = EDGE_CURVE ( 'NONE', #33159, #18007, #17157, .T. ) ;
#36825 = LINE ( 'NONE', #44185, #32595 ) ;
#36826 = CARTESIAN_POINT ( 'NONE',  ( 0.000000000000000000, 0.000000000000000000, 0.000000000000000000 ) ) ;
#36827 = AXIS2_PLACEMENT_3D ( 'NONE', #9411, #1107, #2087 ) ;
#36828 = ORIENTED_EDGE ( 'NONE', *, *, #8243, .T. ) ;
#36829 = CARTESIAN_POINT ( 'NONE',  ( 0.000000000000000000, -120.0000000000000000, 2.500000000000000000 ) ) ;
#36830 = CIRCLE ( 'NONE', #4002, 82.00000000000000000 ) ;
#36831 = CIRCLE ( 'NONE', #46244, 15.99999999999999822 ) ;
#36832 = DIRECTION ( 'NONE',  ( 0.000000000000000000, 0.000000000000000000, 1.000000000000000000 ) ) ;
#36833 = VERTEX_POINT ( 'NONE', #43122 ) ;
#36834 = EDGE_LOOP ( 'NONE', ( #14251, #19062, #43646, #8367 ) ) ;
#36835 = VECTOR ( 'NONE', #15411, 1000.000000000000114 ) ;
#36836 = EDGE_CURVE ( 'NONE', #45945, #15085, #46881, .T. ) ;
#36837 = CIRCLE ( 'NONE', #2461, 16.00000000000000000 ) ;
#36838 = ADVANCED_FACE ( 'NONE', ( #31887 ), #27056, .T. ) ;
#36839 = DIRECTION ( 'NONE',  ( -1.000000000000000000, 0.000000000000000000, -0.000000000000000000 ) ) ;
#36840 = VERTEX_POINT ( 'NONE', #9822 ) ;
#36841 = ADVANCED_FACE ( 'NONE', ( #9106 ), #39457, .T. ) ;
#36842 = ORIENTED_EDGE ( 'NONE', *, *, #40404, .F. ) ;
#36843 = CARTESIAN_POINT ( 'NONE',  ( 11.99999999999999822, -72.35160999960831418, 20.41045688087797672 ) ) ;
#36844 = EDGE_CURVE ( 'NONE', #14848, #36901, #38281, .T. ) ;
#36845 = DIRECTION ( 'NONE',  ( 0.000000000000000000, 0.000000000000000000, 1.000000000000000000 ) ) ;
#36846 = DIRECTION ( 'NONE',  ( 1.000000000000000000, 0.000000000000000000, 0.000000000000000000 ) ) ;
#36847 = ORIENTED_EDGE ( 'NONE', *, *, #44378, .T. ) ;
#36848 = CARTESIAN_POINT ( 'NONE',  ( -10.00000000000000000, 0.000000000000000000, 0.000000000000000000 ) ) ;
#36849 = EDGE_LOOP ( 'NONE', ( #6330, #30471, #44163, #11492 ) ) ;
#36850 = EDGE_LOOP ( 'NONE', ( #36271, #10171, #4787, #30783 ) ) ;
#36851 = EDGE_LOOP ( 'NONE', ( #32498, #29879, #12263, #5890 ) ) ;
#36852 = CARTESIAN_POINT ( 'NONE',  ( 11.99999999999999822, 0.000000000000000000, 0.000000000000000000 ) ) ;
#36854 = VERTEX_POINT ( 'NONE', #1760 ) ;
#36853 = CARTESIAN_POINT ( 'NONE',  ( 11.99999999999999822, 17.28742895386084655, 75.54627589209950145 ) ) ;
#36855 = CIRCLE ( 'NONE', #11088, 77.49899999999998101 ) ;
#36856 = FACE_BOUND ( 'NONE', #2962, .T. ) ;
#36858 = VERTEX_POINT ( 'NONE', #10064 ) ;
#36857 = AXIS2_PLACEMENT_3D ( 'NONE', #45124, #30205, #40976 ) ;
#36859 = VERTEX_POINT ( 'NONE', #24761 ) ;
#36860 = DIRECTION ( 'NONE',  ( 0.000000000000000000, 0.5877852522924708056, -0.8090169943749491166 ) ) ;
#36861 = VERTEX_POINT ( 'NONE', #6160 ) ;
#36862 = VECTOR ( 'NONE', #13992, 1000.000000000000000 ) ;
#36863 = DIRECTION ( 'NONE',  ( 0.6575728627325955200, -0.7533909544171996098, -1.230411769795008318E-16 ) ) ;
#36864 = CARTESIAN_POINT ( 'NONE',  ( 10.00000000000000000, 0.000000000000000000, 0.000000000000000000 ) ) ;
#36865 = CARTESIAN_POINT ( 'NONE',  ( 11.99999999999999822, -35.91791733033428358, -68.67312586195033930 ) ) ;
#36866 = CARTESIAN_POINT ( 'NONE',  ( 11.99999999999999822, 74.74816331893428867, 33.71516098798767302 ) ) ;
#36867 = FACE_OUTER_BOUND ( 'NONE', #10133, .T. ) ;
#36868 = AXIS2_PLACEMENT_3D ( 'NONE', #20637, #12823, #38782 ) ;
#36869 = AXIS2_PLACEMENT_3D ( 'NONE', #32497, #17303, #13408 ) ;
#36870 = DIRECTION ( 'NONE',  ( -1.000000000000000000, 0.000000000000000000, -0.000000000000000000 ) ) ;
#36871 = CARTESIAN_POINT ( 'NONE',  ( 0.000000000000000000, 14.60985201121729737, -18.46759930825687945 ) ) ;
#36872 = DIRECTION ( 'NONE',  ( 0.000000000000000000, 0.000000000000000000, 1.000000000000000000 ) ) ;
#36873 = VERTEX_POINT ( 'NONE', #12137 ) ;
#36874 = CARTESIAN_POINT ( 'NONE',  ( 11.99999999999999822, 64.81221759200343513, 50.23322058963371006 ) ) ;
#36875 = CARTESIAN_POINT ( 'NONE',  ( 10.00000000000000000, 35.92658777277511462, 10.74501242461295014 ) ) ;
#36876 = ORIENTED_EDGE ( 'NONE', *, *, #9783, .F. ) ;
#36877 = DIRECTION ( 'NONE',  ( -1.000000000000000000, 0.000000000000000000, -0.000000000000000000 ) ) ;
#36878 = LINE ( 'NONE', #3346, #17442 ) ;
#36879 = CARTESIAN_POINT ( 'NONE',  ( 11.99999999999999822, 62.20884554314085335, -46.21855187248562657 ) ) ;
#36880 = DIRECTION ( 'NONE',  ( 1.000000000000000000, 0.000000000000000000, -0.000000000000000000 ) ) ;
#36881 = DIRECTION ( 'NONE',  ( -0.3311129884571281101, -0.9435911131814402886, 0.000000000000000000 ) ) ;
#36882 = DIRECTION ( 'NONE',  ( -0.000000000000000000, -0.3090169943749448977, -0.9510565162951543083 ) ) ;
#36883 = CARTESIAN_POINT ( 'NONE',  ( 0.000000000000000000, 2.543863470249527303, -81.96053171279901051 ) ) ;
#36884 =( NAMED_UNIT ( * ) PLANE_ANGLE_UNIT ( ) SI_UNIT ( $, .RADIAN. ) );
#36885 = DIRECTION ( 'NONE',  ( -1.000000000000000000, -0.000000000000000000, -0.000000000000000000 ) ) ;
#36886 = ORIENTED_EDGE ( 'NONE', *, *, #18885, .T. ) ;
#36887 = ORIENTED_EDGE ( 'NONE', *, *, #32053, .F. ) ;
#36888 = AXIS2_PLACEMENT_3D ( 'NONE', #7928, #33876, #45151 ) ;
#36889 = EDGE_CURVE ( 'NONE', #16167, #13391, #2235, .T. ) ;
#36890 = EDGE_LOOP ( 'NONE', ( #36460, #12210, #47861, #3906 ) ) ;
#36891 = CIRCLE ( 'NONE', #25187, 82.00000000000000000 ) ;
#36892 = CARTESIAN_POINT ( 'NONE',  ( -3.249999999999999556, -13.95926121303099343, 0.000000000000000000 ) ) ;
#36893 = EDGE_CURVE ( 'NONE', #25146, #4907, #39706, .T. ) ;
#36894 = DIRECTION ( 'NONE',  ( -1.000000000000000000, 0.000000000000000000, 0.000000000000000000 ) ) ;
#36895 = ORIENTED_EDGE ( 'NONE', *, *, #38639, .T. ) ;
#36896 = AXIS2_PLACEMENT_3D ( 'NONE', #21409, #33157, #93 ) ;
#36897 = ORIENTED_EDGE ( 'NONE', *, *, #47320, .T. ) ;
#36898 = ADVANCED_FACE ( 'NONE', ( #36002 ), #28675, .F. ) ;
#36899 = CARTESIAN_POINT ( 'NONE',  ( -42.50000000000000000, 2.571758278209441267E-15, 20.99999999999999645 ) ) ;
#36900 = AXIS2_PLACEMENT_3D ( 'NONE', #21182, #17513, #9446 ) ;
#36901 = VERTEX_POINT ( 'NONE', #34365 ) ;
#36902 = EDGE_CURVE ( 'NONE', #32256, #35410, #24043, .T. ) ;
#36903 = ORIENTED_EDGE ( 'NONE', *, *, #7345, .T. ) ;
#36904 = DIRECTION ( 'NONE',  ( -1.000000000000000000, -0.000000000000000000, -0.000000000000000000 ) ) ;
#36905 = VERTEX_POINT ( 'NONE', #5674 ) ;
#36906 = CARTESIAN_POINT ( 'NONE',  ( 0.000000000000000000, -51.03279382321125723, 55.19960302592048862 ) ) ;
#36907 = VERTEX_POINT ( 'NONE', #20593 ) ;
#36908 = EDGE_LOOP ( 'NONE', ( #27574, #44098, #17782, #3074 ) ) ;
#36909 = DIRECTION ( 'NONE',  ( -1.000000000000000000, -0.000000000000000000, -0.000000000000000000 ) ) ;
#36910 = DIRECTION ( 'NONE',  ( -1.000000000000000000, 0.000000000000000000, 0.000000000000000000 ) ) ;
#36911 = DIRECTION ( 'NONE',  ( -1.000000000000000000, -0.000000000000000000, -0.000000000000000000 ) ) ;
#36912 = VERTEX_POINT ( 'NONE', #16934 ) ;
#36913 = VERTEX_POINT ( 'NONE', #44552 ) ;
#36914 = AXIS2_PLACEMENT_3D ( 'NONE', #33580, #42, #288 ) ;
#36915 = CARTESIAN_POINT ( 'NONE',  ( 0.000000000000000000, -73.72996012237449293, 14.67089635893687571 ) ) ;
#36916 = DIRECTION ( 'NONE',  ( 0.000000000000000000, -0.4539904997395540764, 0.8910065241883642351 ) ) ;
#36917 = AXIS2_PLACEMENT_3D ( 'NONE', #46042, #8348, #45303 ) ;
#36918 = ORIENTED_EDGE ( 'NONE', *, *, #30966, .F. ) ;
#36919 = ORIENTED_EDGE ( 'NONE', *, *, #28149, .F. ) ;
#36920 = CARTESIAN_POINT ( 'NONE',  ( -3.000000000000000000, -0.9646360437372163421, -23.52805723605591126 ) ) ;
#36921 = DIRECTION ( 'NONE',  ( -1.000000000000000000, 0.000000000000000000, -0.000000000000000000 ) ) ;
#36922 = ORIENTED_EDGE ( 'NONE', *, *, #28616, .T. ) ;
#36923 = CIRCLE ( 'NONE', #31514, 31.99999999999999289 ) ;
#36924 = CARTESIAN_POINT ( 'NONE',  ( 0.000000000000000000, 20.85821328998741109, 10.92862929874522315 ) ) ;
#36925 = AXIS2_PLACEMENT_3D ( 'NONE', #22491, #38384, #34216 ) ;
#36926 = DIRECTION ( 'NONE',  ( 0.000000000000000000, -0.9969173337331287410, 0.07845909572783489605 ) ) ;
#36927 = CARTESIAN_POINT ( 'NONE',  ( 0.000000000000000000, 8.840884882375075193, 74.65374052328651544 ) ) ;
#36928 = LINE ( 'NONE', #3400, #1768 ) ;
#36929 = CARTESIAN_POINT ( 'NONE',  ( 0.000000000000000000, 63.97538442413498672, -51.29473840253155714 ) ) ;
#36930 = CIRCLE ( 'NONE', #33023, 30.50000000000000000 ) ;
#36931 = DIRECTION ( 'NONE',  ( -1.000000000000000000, 0.000000000000000000, -0.000000000000000000 ) ) ;
#36932 = EDGE_CURVE ( 'NONE', #1711, #27887, #29682, .T. ) ;
#36933 = VECTOR ( 'NONE', #34168, 1000.000000000000227 ) ;
#36934 = DIRECTION ( 'NONE',  ( -1.000000000000000000, 0.000000000000000000, 0.000000000000000000 ) ) ;
#36935 = DIRECTION ( 'NONE',  ( -1.000000000000000000, -0.000000000000000000, -0.000000000000000000 ) ) ;
#36936 = VERTEX_POINT ( 'NONE', #37211 ) ;
#36937 = AXIS2_PLACEMENT_3D ( 'NONE', #31447, #12837, #20649 ) ;
#36938 = EDGE_CURVE ( 'NONE', #40294, #28131, #24987, .T. ) ;
#36939 = DIRECTION ( 'NONE',  ( 0.000000000000000000, 0.9510565162951503115, -0.3090169943749573878 ) ) ;
#36940 = DIRECTION ( 'NONE',  ( 1.000000000000000000, -0.000000000000000000, -0.000000000000000000 ) ) ;
#36941 = ADVANCED_FACE ( 'NONE', ( #29863 ), #33299, .T. ) ;
#36942 = DIRECTION ( 'NONE',  ( 0.000000000000000000, 0.000000000000000000, 1.000000000000000000 ) ) ;
#36943 = ORIENTED_EDGE ( 'NONE', *, *, #18464, .T. ) ;
#36944 = UNCERTAINTY_MEASURE_WITH_UNIT (LENGTH_MEASURE( 1.000000000000000082E-05 ), #46490, 'distance_accuracy_value', 'NONE');
#36945 = CARTESIAN_POINT ( 'NONE',  ( 11.99999999999999822, -12.93880638057260946, -76.41127070299286572 ) ) ;
#36946 = CIRCLE ( 'NONE', #33817, 16.00000000000000355 ) ;
#36947 = ADVANCED_FACE ( 'NONE', ( #21791 ), #18366, .T. ) ;
#36948 = LINE ( 'NONE', #3425, #2627 ) ;
#36949 = VERTEX_POINT ( 'NONE', #44792 ) ;
#36950 = EDGE_CURVE ( 'NONE', #47647, #8291, #25697, .T. ) ;
#36951 = EDGE_CURVE ( 'NONE', #42762, #28234, #6639, .T. ) ;
#36952 = AXIS2_PLACEMENT_3D ( 'NONE', #43350, #9805, #40157 ) ;
#36953 = VECTOR ( 'NONE', #4451, 1000.000000000000000 ) ;
#36954 = DIRECTION ( 'NONE',  ( 0.000000000000000000, 0.000000000000000000, 1.000000000000000000 ) ) ;
#36955 = AXIS2_PLACEMENT_3D ( 'NONE', #45195, #640, #26590 ) ;
#36956 = AXIS2_PLACEMENT_3D ( 'NONE', #24060, #5448, #20361 ) ;
#36957 = ORIENTED_EDGE ( 'NONE', *, *, #10498, .F. ) ;
#36958 = DIRECTION ( 'NONE',  ( -1.000000000000000000, 0.000000000000000000, 0.000000000000000000 ) ) ;
#36959 = EDGE_LOOP ( 'NONE', ( #19941, #12421, #14651, #47326 ) ) ;
#36960 = ORIENTED_EDGE ( 'NONE', *, *, #23422, .T. ) ;
#36961 = ORIENTED_EDGE ( 'NONE', *, *, #1551, .T. ) ;
#36962 = EDGE_CURVE ( 'NONE', #17873, #30560, #35960, .T. ) ;
#36963 = EDGE_LOOP ( 'NONE', ( #29760, #6893, #6889, #4673 ) ) ;
#36964 = DIRECTION ( 'NONE',  ( 0.000000000000000000, -0.9510565162951502005, -0.3090169943749581094 ) ) ;
#36965 = VECTOR ( 'NONE', #9027, 1000.000000000000000 ) ;
#36966 = PRODUCT_DEFINITION ( 'UNKNOWN', '', #13934, #44784 ) ;
#36967 = CARTESIAN_POINT ( 'NONE',  ( -5.565113727472242644, 10.17789316117535137, 52.00000000000002132 ) ) ;
#36968 = CIRCLE ( 'NONE', #35404, 77.49899999999999523 ) ;
#36969 = ORIENTED_EDGE ( 'NONE', *, *, #33866, .T. ) ;
#36970 = ORIENTED_EDGE ( 'NONE', *, *, #26068, .F. ) ;
#36971 = CYLINDRICAL_SURFACE ( 'NONE', #18879, 82.00000000000000000 ) ;
#36972 = AXIS2_PLACEMENT_3D ( 'NONE', #10613, #7419, #44616 ) ;
#36973 = ORIENTED_EDGE ( 'NONE', *, *, #42156, .T. ) ;
#36974 = EDGE_CURVE ( 'NONE', #2823, #10347, #47979, .T. ) ;
#36975 = CYLINDRICAL_SURFACE ( 'NONE', #16038, 77.49899999999999523 ) ;
#36976 = DIRECTION ( 'NONE',  ( 0.000000000000000000, 0.000000000000000000, 1.000000000000000000 ) ) ;
#36977 = VERTEX_POINT ( 'NONE', #33050 ) ;
#36978 = DIRECTION ( 'NONE',  ( -1.000000000000000000, 0.000000000000000000, 0.000000000000000000 ) ) ;
#36979 = DIRECTION ( 'NONE',  ( 0.6516173805718078471, -0.7585478161175706058, 0.000000000000000000 ) ) ;
#36980 = ORIENTED_EDGE ( 'NONE', *, *, #251, .F. ) ;
#36982 = ORIENTED_EDGE ( 'NONE', *, *, #45996, .T. ) ;
#36981 = DIRECTION ( 'NONE',  ( -1.000000000000000000, -0.000000000000000000, -0.000000000000000000 ) ) ;
#36983 = DIRECTION ( 'NONE',  ( -1.000000000000000000, 0.000000000000000000, 0.000000000000000000 ) ) ;
#36984 = EDGE_LOOP ( 'NONE', ( #14270, #25469, #44682, #6430 ) ) ;
#36985 = PLANE ( 'NONE',  #14659 ) ;
#36986 = ORIENTED_EDGE ( 'NONE', *, *, #17681, .F. ) ;
#36987 = ORIENTED_EDGE ( 'NONE', *, *, #47138, .T. ) ;
#36988 = CYLINDRICAL_SURFACE ( 'NONE', #29920, 31.99999999999999289 ) ;
#36989 = CARTESIAN_POINT ( 'NONE',  ( 10.00000000000000000, 49.70050353004977239, -59.46389618801908483 ) ) ;
#36990 = CARTESIAN_POINT ( 'NONE',  ( 11.99999999999999822, -39.78640506895651896, 66.50666863321988842 ) ) ;
#36991 = CARTESIAN_POINT ( 'NONE',  ( 0.000000000000000000, 12.93880638057426502, -76.41127070299258150 ) ) ;
#36992 = CARTESIAN_POINT ( 'NONE',  ( 0.000000000000000000, 6.736453364084091788, -36.88895765772625879 ) ) ;
#36993 = VERTEX_POINT ( 'NONE', #10553 ) ;
#36994 = AXIS2_PLACEMENT_3D ( 'NONE', #48220, #11267, #7593 ) ;
#36995 = CARTESIAN_POINT ( 'NONE',  ( -8.637688417678527131, 13.69818742750669394, 52.00000000000002132 ) ) ;
#36997 = EDGE_CURVE ( 'NONE', #6193, #10782, #3680, .T. ) ;
#36996 = CARTESIAN_POINT ( 'NONE',  ( 10.00000000000000000, 74.65491531819118620, 23.16904090965733332 ) ) ;
#36998 = FACE_OUTER_BOUND ( 'NONE', #17225, .T. ) ;
#36999 = VERTEX_POINT ( 'NONE', #6877 ) ;
#37000 = EDGE_CURVE ( 'NONE', #2082, #35557, #25942, .T. ) ;
#37001 = DIRECTION ( 'NONE',  ( 0.000000000000000000, -0.9876883405951358830, -0.1564344650402420822 ) ) ;
#37002 = DIRECTION ( 'NONE',  ( -0.000000000000000000, 0.8090169943749503378, 0.5877852522924690293 ) ) ;
#37003 = CARTESIAN_POINT ( 'NONE',  ( 10.00000000000000000, -5.256550761632340141, -77.32052557432847095 ) ) ;
#37004 = DIRECTION ( 'NONE',  ( -1.000000000000000000, 0.000000000000000000, -0.000000000000000000 ) ) ;
#37005 = AXIS2_PLACEMENT_3D ( 'NONE', #17066, #24666, #17298 ) ;
#37006 = AXIS2_PLACEMENT_3D ( 'NONE', #19854, #38734, #5922 ) ;
#37007 = EDGE_CURVE ( 'NONE', #11522, #32747, #2948, .T. ) ;
#37008 = DIRECTION ( 'NONE',  ( -1.000000000000000000, -0.000000000000000000, 0.000000000000000000 ) ) ;
#37009 = CARTESIAN_POINT ( 'NONE',  ( 5.000000000000002665, -40.65526001592565564, -71.21200624218839437 ) ) ;
#37010 = PLANE ( 'NONE',  #31912 ) ;
#37011 = DIRECTION ( 'NONE',  ( -1.000000000000000000, 0.000000000000000000, 0.000000000000000000 ) ) ;
#37012 = EDGE_CURVE ( 'NONE', #43777, #26532, #6395, .T. ) ;
#37013 = AXIS2_PLACEMENT_3D ( 'NONE', #28056, #9432, #35867 ) ;
#37014 = ORIENTED_EDGE ( 'NONE', *, *, #36737, .T. ) ;
#37016 = FACE_OUTER_BOUND ( 'NONE', #24034, .T. ) ;
#37015 = AXIS2_PLACEMENT_3D ( 'NONE', #32116, #39211, #35537 ) ;
#37017 = AXIS2_PLACEMENT_3D ( 'NONE', #48092, #18219, #37071 ) ;
#37018 = ORIENTED_EDGE ( 'NONE', *, *, #11506, .T. ) ;
#37019 = AXIS2_PLACEMENT_3D ( 'NONE', #26477, #14981, #29657 ) ;
#37020 = DIRECTION ( 'NONE',  ( 0.000000000000000000, 0.000000000000000000, 1.000000000000000000 ) ) ;
#37021 = AXIS2_PLACEMENT_3D ( 'NONE', #46741, #9044, #16875 ) ;
#37022 = CARTESIAN_POINT ( 'NONE',  ( 4.553649124439118623E-15, 4.011548038196366406E-15, 52.00000000000002132 ) ) ;
#37023 = VERTEX_POINT ( 'NONE', #3184 ) ;
#37024 = CARTESIAN_POINT ( 'NONE',  ( 0.000000000000000000, -81.34940948281328588, -10.30890764327469711 ) ) ;
#37025 = AXIS2_PLACEMENT_3D ( 'NONE', #2780, #18437, #21377 ) ;
#37026 = ORIENTED_EDGE ( 'NONE', *, *, #41488, .F. ) ;
#37027 = ADVANCED_FACE ( 'NONE', ( #10791 ), #29394, .T. ) ;
#37028 = EDGE_CURVE ( 'NONE', #36483, #47876, #2711, .T. ) ;
#37029 = FACE_OUTER_BOUND ( 'NONE', #23246, .T. ) ;
#37030 = VERTEX_POINT ( 'NONE', #25466 ) ;
#37031 = AXIS2_PLACEMENT_3D ( 'NONE', #32404, #25520, #14524 ) ;
#37032 = EDGE_CURVE ( 'NONE', #11671, #29028, #14768, .T. ) ;
#37033 = AXIS2_PLACEMENT_3D ( 'NONE', #18138, #22326, #33080 ) ;
#37034 = LINE ( 'NONE', #14283, #37829 ) ;
#37035 = VERTEX_POINT ( 'NONE', #17875 ) ;
#37036 = CARTESIAN_POINT ( 'NONE',  ( -12.50000000000000000, -132.5000000000000000, 2.500000000000000000 ) ) ;
#37037 = AXIS2_PLACEMENT_3D ( 'NONE', #1318, #34335, #46338 ) ;
#37038 = AXIS2_PLACEMENT_3D ( 'NONE', #36629, #14367, #10705 ) ;
#37039 = LINE ( 'NONE', #44626, #16030 ) ;
#37040 = VECTOR ( 'NONE', #28542, 1000.000000000000000 ) ;
#37041 = ORIENTED_EDGE ( 'NONE', *, *, #43267, .T. ) ;
#37042 = CARTESIAN_POINT ( 'NONE',  ( 10.00000000000000000, 37.16516213103285082, -4.992566952384588141 ) ) ;
#37043 = ORIENTED_EDGE ( 'NONE', *, *, #47708, .F. ) ;
#37044 = LINE ( 'NONE', #3514, #46461 ) ;
#37045 = DIRECTION ( 'NONE',  ( 1.000000000000000000, 0.000000000000000000, 0.000000000000000000 ) ) ;
#37046 = CARTESIAN_POINT ( 'NONE',  ( 10.00000000000000000, -59.75363087400034345, -56.15606465355021015 ) ) ;
#37047 = CARTESIAN_POINT ( 'NONE',  ( 0.000000000000000000, 0.000000000000000000, 0.000000000000000000 ) ) ;
#37048 = CIRCLE ( 'NONE', #24557, 82.00000000000000000 ) ;
#37049 = AXIS2_PLACEMENT_3D ( 'NONE', #12297, #7876, #42381 ) ;
#37050 = ORIENTED_EDGE ( 'NONE', *, *, #35094, .T. ) ;
#37051 = CARTESIAN_POINT ( 'NONE',  ( 10.00000000000000000, 0.000000000000000000, 0.000000000000000000 ) ) ;
#37052 = ORIENTED_EDGE ( 'NONE', *, *, #2306, .F. ) ;
#37053 = ORIENTED_EDGE ( 'NONE', *, *, #41548, .F. ) ;
#37054 = AXIS2_PLACEMENT_3D ( 'NONE', #12458, #23703, #27626 ) ;
#37055 = DIRECTION ( 'NONE',  ( 0.000000000000000000, 0.000000000000000000, 1.000000000000000000 ) ) ;
#37056 = CARTESIAN_POINT ( 'NONE',  ( 0.000000000000000000, 50.23322058963442061, -64.81221759200289512 ) ) ;
#37057 = DIRECTION ( 'NONE',  ( 0.000000000000000000, 0.000000000000000000, 1.000000000000000000 ) ) ;
#37058 = CARTESIAN_POINT ( 'NONE',  ( -10.00000000000000000, 0.000000000000000000, 0.000000000000000000 ) ) ;
#37059 = ORIENTED_EDGE ( 'NONE', *, *, #5426, .T. ) ;
#37060 = DIRECTION ( 'NONE',  ( -1.000000000000000000, -0.000000000000000000, 0.000000000000000000 ) ) ;
#37061 = CIRCLE ( 'NONE', #40180, 16.00000000000000000 ) ;
#37062 = CARTESIAN_POINT ( 'NONE',  ( 11.99999999999999822, 0.000000000000000000, 0.000000000000000000 ) ) ;
#37063 = DIRECTION ( 'NONE',  ( 1.000000000000000000, -0.000000000000000000, -0.000000000000000000 ) ) ;
#37064 = DIRECTION ( 'NONE',  ( -0.000000000000000000, -0.000000000000000000, -1.000000000000000000 ) ) ;
#37065 = FACE_OUTER_BOUND ( 'NONE', #30419, .T. ) ;
#37066 = DIRECTION ( 'NONE',  ( -1.000000000000000000, 0.000000000000000000, -0.000000000000000000 ) ) ;
#37067 = CARTESIAN_POINT ( 'NONE',  ( 11.99999999999999822, 20.40083707022882820, 72.35432306680490910 ) ) ;
#37068 = CARTESIAN_POINT ( 'NONE',  ( 10.00000000000000000, 39.78640506895700213, -66.50666863321957578 ) ) ;
#37069 = EDGE_CURVE ( 'NONE', #34359, #25700, #27282, .T. ) ;
#37070 = DIRECTION ( 'NONE',  ( 0.000000000000000000, 0.000000000000000000, 1.000000000000000000 ) ) ;
#37071 = DIRECTION ( 'NONE',  ( 0.000000000000000000, 0.000000000000000000, 1.000000000000000000 ) ) ;
#37072 = EDGE_CURVE ( 'NONE', #18858, #44417, #28142, .T. ) ;
#37073 = DIRECTION ( 'NONE',  ( 0.9997280174009348652, -0.02332147558787931590, 0.000000000000000000 ) ) ;
#37074 = CIRCLE ( 'NONE', #22233, 77.49900000000000944 ) ;
#37075 = DIRECTION ( 'NONE',  ( 1.000000000000000000, 0.000000000000000000, 0.000000000000000000 ) ) ;
#37076 = LINE ( 'NONE', #6744, #10487 ) ;
#37077 = CARTESIAN_POINT ( 'NONE',  ( 10.00000000000000000, -37.01155633439063308, 6.555932627142289526 ) ) ;
#37078 = CARTESIAN_POINT ( 'NONE',  ( 16.84844760790522855, -103.5491698323862124, 5.500000000000000000 ) ) ;
#37079 = VECTOR ( 'NONE', #14271, 1000.000000000000000 ) ;
#37080 = VECTOR ( 'NONE', #30932, 1000.000000000000000 ) ;
#37081 = DIRECTION ( 'NONE',  ( -1.000000000000000000, 0.000000000000000000, 0.000000000000000000 ) ) ;
#37082 = ORIENTED_EDGE ( 'NONE', *, *, #39580, .F. ) ;
#37083 = ADVANCED_FACE ( 'NONE', ( #26205 ), #30594, .F. ) ;
#37084 = ORIENTED_EDGE ( 'NONE', *, *, #47127, .T. ) ;
#37085 = EDGE_CURVE ( 'NONE', #42163, #3180, #11521, .T. ) ;
#37086 = CIRCLE ( 'NONE', #16802, 16.00000000000000000 ) ;
#37087 = CIRCLE ( 'NONE', #325, 82.00000000000000000 ) ;
#37088 = ADVANCED_FACE ( 'NONE', ( #501 ), #19550, .F. ) ;
#37089 = AXIS2_PLACEMENT_3D ( 'NONE', #39850, #2871, #13416 ) ;
#37090 = CIRCLE ( 'NONE', #16000, 82.00000000000000000 ) ;
#37091 = FACE_OUTER_BOUND ( 'NONE', #19248, .T. ) ;
#37092 = VERTEX_POINT ( 'NONE', #8547 ) ;
#37093 = VECTOR ( 'NONE', #23245, 1000.000000000000000 ) ;
#37094 = EDGE_CURVE ( 'NONE', #44946, #19509, #15194, .T. ) ;
#37095 = DIRECTION ( 'NONE',  ( 0.000000000000000000, 0.000000000000000000, 1.000000000000000000 ) ) ;
#37096 = DIRECTION ( 'NONE',  ( -1.000000000000000000, 0.000000000000000000, 0.000000000000000000 ) ) ;
#37098 = VERTEX_POINT ( 'NONE', #34740 ) ;
#37097 = DIRECTION ( 'NONE',  ( 0.000000000000000000, 0.4539904997395412534, 0.8910065241883706744 ) ) ;
#37099 = VERTEX_POINT ( 'NONE', #23253 ) ;
#37100 = LINE ( 'NONE', #7494, #3921 ) ;
#37101 = ORIENTED_EDGE ( 'NONE', *, *, #45302, .T. ) ;
#37102 = EDGE_LOOP ( 'NONE', ( #23943, #4652, #40535, #13175 ) ) ;
#37103 = DIRECTION ( 'NONE',  ( -1.000000000000000000, 0.000000000000000000, 0.000000000000000000 ) ) ;
#37104 = CARTESIAN_POINT ( 'NONE',  ( 10.00000000000000000, 0.000000000000000000, 0.000000000000000000 ) ) ;
#37106 = DIRECTION ( 'NONE',  ( 0.000000000000000000, 0.000000000000000000, 1.000000000000000000 ) ) ;
#37105 = AXIS2_PLACEMENT_3D ( 'NONE', #9257, #9023, #42562 ) ;
#37107 = ORIENTED_EDGE ( 'NONE', *, *, #18566, .F. ) ;
#37108 = ORIENTED_EDGE ( 'NONE', *, *, #35261, .T. ) ;
#37109 = DIRECTION ( 'NONE',  ( 0.000000000000000000, -0.4999999999999930611, 0.8660254037844425934 ) ) ;
#37110 = VERTEX_POINT ( 'NONE', #26686 ) ;
#37111 = AXIS2_PLACEMENT_3D ( 'NONE', #37782, #23098, #583 ) ;
#37112 = DIRECTION ( 'NONE',  ( 0.000000000000000000, 0.000000000000000000, 1.000000000000000000 ) ) ;
#37113 = CARTESIAN_POINT ( 'NONE',  ( 0.000000000000000000, 74.65491531819105830, 8.830959090343693418 ) ) ;
#37114 = DIRECTION ( 'NONE',  ( 0.000000000000000000, 0.000000000000000000, 1.000000000000000000 ) ) ;
#37115 = FACE_OUTER_BOUND ( 'NONE', #17884, .T. ) ;
#37116 = FACE_OUTER_BOUND ( 'NONE', #33615, .T. ) ;
#37117 = CARTESIAN_POINT ( 'NONE',  ( 11.99999999999999822, 0.000000000000000000, 0.000000000000000000 ) ) ;
#37118 =( LENGTH_UNIT ( ) NAMED_UNIT ( * ) SI_UNIT ( .MILLI., .METRE. ) );
#37119 = CYLINDRICAL_SURFACE ( 'NONE', #45702, 31.99999999999998579 ) ;
#37120 = ORIENTED_EDGE ( 'NONE', *, *, #14658, .F. ) ;
#37121 = CARTESIAN_POINT ( 'NONE',  ( 5.999999999999999112, -51.29473840253177030, -63.97538442413482329 ) ) ;
#37122 = AXIS2_PLACEMENT_3D ( 'NONE', #38808, #9398, #24336 ) ;
#37123 = VECTOR ( 'NONE', #17981, 1000.000000000000000 ) ;
#37124 = ORIENTED_EDGE ( 'NONE', *, *, #29727, .T. ) ;
#37125 = EDGE_CURVE ( 'NONE', #31325, #23206, #45051, .T. ) ;
#37126 = CARTESIAN_POINT ( 'NONE',  ( 10.00000000000000000, 77.19088730480524418, 6.903761155838049390 ) ) ;
#37127 = ORIENTED_EDGE ( 'NONE', *, *, #10281, .F. ) ;
#37128 = EDGE_CURVE ( 'NONE', #14493, #46638, #11728, .T. ) ;
#37129 = AXIS2_PLACEMENT_3D ( 'NONE', #8233, #33271, #10761 ) ;
#37130 = CARTESIAN_POINT ( 'NONE',  ( 0.000000000000000000, 70.53064760720316428, -26.01480285779861035 ) ) ;
#37131 = CARTESIAN_POINT ( 'NONE',  ( 0.000000000000000000, -22.90783923731686045, 78.73519480814945837 ) ) ;
#37132 = CARTESIAN_POINT ( 'NONE',  ( -3.000000000000000000, -18.13022148937263012, 15.02647892043544608 ) ) ;
#37133 = AXIS2_PLACEMENT_3D ( 'NONE', #32441, #17016, #39556 ) ;
#37134 = EDGE_CURVE ( 'NONE', #5004, #20016, #17959, .T. ) ;
#37135 = CIRCLE ( 'NONE', #48065, 35.50000000000000711 ) ;
#37136 = DIRECTION ( 'NONE',  ( 0.000000000000000000, -0.5877852522924624790, -0.8090169943749552228 ) ) ;
#37137 = CARTESIAN_POINT ( 'NONE',  ( -6.782329983125267248, 10.49999999999999645, -105.0000000000000000 ) ) ;
#37138 = EDGE_CURVE ( 'NONE', #9789, #1027, #32070, .T. ) ;
#37139 = ORIENTED_EDGE ( 'NONE', *, *, #14130, .T. ) ;
#37140 = DIRECTION ( 'NONE',  ( -1.000000000000000000, -0.000000000000000000, -0.000000000000000000 ) ) ;
#37141 = EDGE_CURVE ( 'NONE', #28726, #690, #25028, .T. ) ;
#37142 = DIRECTION ( 'NONE',  ( 0.000000000000000000, 0.000000000000000000, 1.000000000000000000 ) ) ;
#37143 = ADVANCED_FACE ( 'NONE', ( #7829 ), #22764, .T. ) ;
#37144 = VECTOR ( 'NONE', #218, 1000.000000000000000 ) ;
#37145 = CARTESIAN_POINT ( 'NONE',  ( 0.000000000000000000, 33.80338159004307386, -16.23288003029461279 ) ) ;
#37146 = CARTESIAN_POINT ( 'NONE',  ( -10.00000000000000000, 0.000000000000000000, 0.000000000000000000 ) ) ;
#37147 = EDGE_LOOP ( 'NONE', ( #9454, #44549, #9819, #33254 ) ) ;
#37148 = ORIENTED_EDGE ( 'NONE', *, *, #39400, .T. ) ;
#37149 = AXIS2_PLACEMENT_3D ( 'NONE', #13898, #29488, #25799 ) ;
#37150 = AXIS2_PLACEMENT_3D ( 'NONE', #4205, #45306, #7861 ) ;
#37151 = ORIENTED_EDGE ( 'NONE', *, *, #1456, .T. ) ;
#37152 = ORIENTED_EDGE ( 'NONE', *, *, #21555, .F. ) ;
#37153 = DIRECTION ( 'NONE',  ( 0.000000000000000000, 0.000000000000000000, -1.000000000000000000 ) ) ;
#37154 = DIRECTION ( 'NONE',  ( 0.000000000000000000, -0.1564344650402170744, -0.9876883405951399908 ) ) ;
#37155 = EDGE_LOOP ( 'NONE', ( #10611, #48281, #38789, #46991 ) ) ;
#37156 = ORIENTED_EDGE ( 'NONE', *, *, #19659, .F. ) ;
#37157 = EDGE_CURVE ( 'NONE', #35449, #2830, #24225, .T. ) ;
#37158 = CIRCLE ( 'NONE', #22317, 31.99999999999998579 ) ;
#37159 = CARTESIAN_POINT ( 'NONE',  ( 0.000000000000000000, 74.65491531819118620, -8.830959090342659579 ) ) ;
#37160 = VERTEX_POINT ( 'NONE', #34253 ) ;
#37161 = ORIENTED_EDGE ( 'NONE', *, *, #45366, .F. ) ;
#37162 = EDGE_CURVE ( 'NONE', #43853, #30369, #31094, .T. ) ;
#37163 = AXIS2_PLACEMENT_3D ( 'NONE', #31596, #43325, #24718 ) ;
#37164 = EDGE_CURVE ( 'NONE', #41833, #36384, #4424, .T. ) ;
#37165 = DIRECTION ( 'NONE',  ( -1.000000000000000000, 0.000000000000000000, -0.000000000000000000 ) ) ;
#37166 = ORIENTED_EDGE ( 'NONE', *, *, #24758, .F. ) ;
#37167 = DIRECTION ( 'NONE',  ( 0.000000000000000000, 0.000000000000000000, 1.000000000000000000 ) ) ;
#37168 = ORIENTED_EDGE ( 'NONE', *, *, #7361, .F. ) ;
#37169 = ORIENTED_EDGE ( 'NONE', *, *, #32268, .F. ) ;
#37170 = DIRECTION ( 'NONE',  ( -1.000000000000000000, -0.000000000000000000, 0.000000000000000000 ) ) ;
#37171 = CARTESIAN_POINT ( 'NONE',  ( -3.000000000000000000, 23.50000000000000000, -1.500000000000001332 ) ) ;
#37172 = CARTESIAN_POINT ( 'NONE',  ( 10.00000000000000000, 0.000000000000000000, 0.000000000000000000 ) ) ;
#37173 = ORIENTED_EDGE ( 'NONE', *, *, #23530, .F. ) ;
#37174 = EDGE_LOOP ( 'NONE', ( #14329, #24338, #6942 ) ) ;
#37176 = ADVANCED_FACE ( 'NONE', ( #4172 ), #15435, .T. ) ;
#37175 = DIRECTION ( 'NONE',  ( 0.000000000000000000, 0.000000000000000000, 1.000000000000000000 ) ) ;
#37177 = CIRCLE ( 'NONE', #15322, 37.49900000000000944 ) ;
#37178 = PLANE ( 'NONE',  #3219 ) ;
#37179 = ORIENTED_EDGE ( 'NONE', *, *, #10469, .T. ) ;
#37180 = ORIENTED_EDGE ( 'NONE', *, *, #42273, .F. ) ;
#37181 = EDGE_CURVE ( 'NONE', #11996, #10143, #44555, .T. ) ;
#37182 = DIRECTION ( 'NONE',  ( 0.000000000000000000, 0.000000000000000000, 1.000000000000000000 ) ) ;
#37183 = CARTESIAN_POINT ( 'NONE',  ( 0.000000000000000000, -68.55367621811173251, 44.99326035066031437 ) ) ;
#37184 = ORIENTED_EDGE ( 'NONE', *, *, #28463, .T. ) ;
#37185 = DIRECTION ( 'NONE',  ( 1.000000000000000000, 0.000000000000000000, 0.000000000000000000 ) ) ;
#37186 = CARTESIAN_POINT ( 'NONE',  ( 10.00000000000000000, -21.32104025579135964, 30.84782396557210760 ) ) ;
#37187 = LINE ( 'NONE', #26176, #36835 ) ;
#37188 = DIRECTION ( 'NONE',  ( 0.000000000000000000, 0.000000000000000000, 1.000000000000000000 ) ) ;
#37189 = EDGE_CURVE ( 'NONE', #19593, #45468, #36719, .T. ) ;
#37190 = DIRECTION ( 'NONE',  ( 0.000000000000000000, 0.000000000000000000, -1.000000000000000000 ) ) ;
#37191 = CYLINDRICAL_SURFACE ( 'NONE', #35153, 31.99999999999998579 ) ;
#37192 = CARTESIAN_POINT ( 'NONE',  ( 10.00000000000000000, 36.73666225445894185, 65.58780272294090707 ) ) ;
#37193 = DIRECTION ( 'NONE',  ( 0.000000000000000000, 0.000000000000000000, 1.000000000000000000 ) ) ;
#37194 = DIRECTION ( 'NONE',  ( 0.000000000000000000, 0.000000000000000000, 1.000000000000000000 ) ) ;
#37195 = ADVANCED_FACE ( 'NONE', ( #232 ), #24702, .T. ) ;
#37196 = AXIS2_PLACEMENT_3D ( 'NONE', #47539, #43636, #42923 ) ;
#37197 = CARTESIAN_POINT ( 'NONE',  ( 15.00000000000000000, 5.835314593368777558, 22.81335362449846471 ) ) ;
#37198 = DIRECTION ( 'NONE',  ( -1.000000000000000000, 0.000000000000000000, -0.000000000000000000 ) ) ;
#37199 = AXIS2_PLACEMENT_3D ( 'NONE', #14790, #29952, #29707 ) ;
#37200 = DIRECTION ( 'NONE',  ( 1.000000000000000000, 0.000000000000000000, 0.000000000000000000 ) ) ;
#37201 = EDGE_LOOP ( 'NONE', ( #27589, #37889, #8536, #21432, #23854, #47397 ) ) ;
#37202 = ORIENTED_EDGE ( 'NONE', *, *, #46708, .T. ) ;
#37203 = CIRCLE ( 'NONE', #1266, 37.49900000000001654 ) ;
#37204 = CARTESIAN_POINT ( 'NONE',  ( 0.000000000000000000, 0.000000000000000000, 125.0000000000000000 ) ) ;
#37205 = VECTOR ( 'NONE', #37, 1000.000000000000114 ) ;
#37206 = VECTOR ( 'NONE', #37557, 1000.000000000000114 ) ;
#37207 = DIRECTION ( 'NONE',  ( 0.000000000000000000, 0.000000000000000000, 1.000000000000000000 ) ) ;
#37208 = ORIENTED_EDGE ( 'NONE', *, *, #15759, .T. ) ;
#37209 = VECTOR ( 'NONE', #25195, 1000.000000000000000 ) ;
#37210 = ORIENTED_EDGE ( 'NONE', *, *, #15735, .T. ) ;
#37211 = CARTESIAN_POINT ( 'NONE',  ( 10.00000000000000000, -35.38097989696503021, -12.42422080174676147 ) ) ;
#37212 = ORIENTED_EDGE ( 'NONE', *, *, #29570, .F. ) ;
#37213 = ORIENTED_EDGE ( 'NONE', *, *, #15431, .T. ) ;
#37214 = EDGE_LOOP ( 'NONE', ( #32755, #17216, #13772, #37816 ) ) ;
#37215 = ORIENTED_EDGE ( 'NONE', *, *, #9842, .T. ) ;
#37216 = ORIENTED_EDGE ( 'NONE', *, *, #13912, .F. ) ;
#37217 = DIRECTION ( 'NONE',  ( 0.000000000000000000, 0.000000000000000000, -1.000000000000000000 ) ) ;
#37218 = CIRCLE ( 'NONE', #27897, 31.99999999999998579 ) ;
#37219 = CARTESIAN_POINT ( 'NONE',  ( 10.00000000000000000, 0.000000000000000000, 0.000000000000000000 ) ) ;
#37220 = EDGE_LOOP ( 'NONE', ( #36773, #1571, #22474, #5388 ) ) ;
#37221 = CARTESIAN_POINT ( 'NONE',  ( 0.000000000000000000, -18.89407956138204980, -75.16055320797050854 ) ) ;
#37222 = EDGE_CURVE ( 'NONE', #28893, #22498, #34373, .T. ) ;
#37223 = EDGE_LOOP ( 'NONE', ( #45053, #34877, #30429, #18974 ) ) ;
#37224 = AXIS2_PLACEMENT_3D ( 'NONE', #17856, #25438, #33024 ) ;
#37225 = LINE ( 'NONE', #40431, #8204 ) ;
#37226 = DIRECTION ( 'NONE',  ( 0.000000000000000000, 0.000000000000000000, 1.000000000000000000 ) ) ;
#37227 = ORIENTED_EDGE ( 'NONE', *, *, #32797, .F. ) ;
#37228 = ORIENTED_EDGE ( 'NONE', *, *, #978, .T. ) ;
#37229 = CARTESIAN_POINT ( 'NONE',  ( 5.000000000000000000, -27.75498641678764855, 31.52238457039590358 ) ) ;
#37230 = DIRECTION ( 'NONE',  ( -1.000000000000000000, 0.000000000000000000, -0.000000000000000000 ) ) ;
#37231 = ORIENTED_EDGE ( 'NONE', *, *, #1495, .T. ) ;
#37233 = VERTEX_POINT ( 'NONE', #42589 ) ;
#37232 = CARTESIAN_POINT ( 'NONE',  ( -21.67772167707813935, -110.8034581014852762, 5.500000000000000000 ) ) ;
#37234 = FACE_OUTER_BOUND ( 'NONE', #41075, .T. ) ;
#37235 = EDGE_LOOP ( 'NONE', ( #11, #21325, #16745, #43303 ) ) ;
#37236 = CIRCLE ( 'NONE', #34901, 77.49899999999999523 ) ;
#37237 = CIRCLE ( 'NONE', #35572, 77.49899999999998101 ) ;
#37238 = LINE ( 'NONE', #36509, #20913 ) ;
#37239 = VERTEX_POINT ( 'NONE', #46503 ) ;
#37240 = ORIENTED_EDGE ( 'NONE', *, *, #12908, .F. ) ;
#37241 = DIRECTION ( 'NONE',  ( -1.000000000000000000, -0.000000000000000000, -0.000000000000000000 ) ) ;
#37242 = DIRECTION ( 'NONE',  ( 0.6064928550163511956, 0.7950889364178798102, -0.000000000000000000 ) ) ;
#37243 = ORIENTED_EDGE ( 'NONE', *, *, #39522, .T. ) ;
#37244 = FACE_OUTER_BOUND ( 'NONE', #20129, .T. ) ;
#37245 = DIRECTION ( 'NONE',  ( -0.8541291221503266584, 0.5200609990133008287, 0.000000000000000000 ) ) ;
#37246 = CYLINDRICAL_SURFACE ( 'NONE', #37019, 82.00000000000000000 ) ;
#37247 = EDGE_CURVE ( 'NONE', #13778, #8400, #13306, .T. ) ;
#37248 = AXIS2_PLACEMENT_3D ( 'NONE', #15215, #7618, #47997 ) ;
#37249 = DIRECTION ( 'NONE',  ( -1.000000000000000000, 0.000000000000000000, 0.000000000000000000 ) ) ;
#37250 = EDGE_CURVE ( 'NONE', #19346, #35835, #31308, .T. ) ;
#37251 = DIRECTION ( 'NONE',  ( -1.000000000000000000, 0.000000000000000000, 0.000000000000000000 ) ) ;
#37252 = EDGE_CURVE ( 'NONE', #7054, #38938, #8601, .T. ) ;
#37253 = AXIS2_PLACEMENT_3D ( 'NONE', #29321, #29554, #6558 ) ;
#37254 = CARTESIAN_POINT ( 'NONE',  ( 10.00000000000000000, 0.000000000000000000, 0.000000000000000000 ) ) ;
#37255 = DIRECTION ( 'NONE',  ( -0.000000000000000000, -0.9135454576426059736, 0.4067366430757887730 ) ) ;
#37256 = DIRECTION ( 'NONE',  ( 1.000000000000000000, 0.000000000000000000, 0.000000000000000000 ) ) ;
#37257 = DIRECTION ( 'NONE',  ( 0.000000000000000000, -1.000000000000000000, -1.047444401652940007E-14 ) ) ;
#37258 = FACE_OUTER_BOUND ( 'NONE', #21112, .T. ) ;
#37259 = ADVANCED_FACE ( 'NONE', ( #13203 ), #28128, .F. ) ;
#37260 = EDGE_CURVE ( 'NONE', #10554, #2634, #21111, .T. ) ;
#37261 = PLANE ( 'NONE',  #2580 ) ;
#37262 = CARTESIAN_POINT ( 'NONE',  ( 11.99999999999999822, -81.90746397400391743, 3.894527615417590294 ) ) ;
#37263 = CARTESIAN_POINT ( 'NONE',  ( -3.000000000000000000, 8.688484142253939169, 21.88630264137371029 ) ) ;
#37264 = DIRECTION ( 'NONE',  ( 0.000000000000000000, -0.07845909572783058006, -0.9969173337331290741 ) ) ;
#37265 = VERTEX_POINT ( 'NONE', #5871 ) ;
#37266 = VECTOR ( 'NONE', #26053, 1000.000000000000000 ) ;
#37267 = ORIENTED_EDGE ( 'NONE', *, *, #45502, .T. ) ;
#37268 = VECTOR ( 'NONE', #34884, 1000.000000000000000 ) ;
#37269 = DIRECTION ( 'NONE',  ( -0.2306669878475622604, -0.9730327541852497042, 0.000000000000000000 ) ) ;
#37270 = EDGE_LOOP ( 'NONE', ( #565, #36023, #44996, #15669 ) ) ;
#37271 = FACE_OUTER_BOUND ( 'NONE', #43310, .T. ) ;
#37272 = DIRECTION ( 'NONE',  ( 1.000000000000000000, 0.000000000000000000, 0.000000000000000000 ) ) ;
#37273 = CIRCLE ( 'NONE', #5246, 16.00000000000000000 ) ;
#37274 = CARTESIAN_POINT ( 'NONE',  ( 10.00000000000000000, -33.17418723428294669, -17.67226234102862747 ) ) ;
#37275 = VERTEX_POINT ( 'NONE', #38919 ) ;
#37276 = CIRCLE ( 'NONE', #4478, 82.00000000000000000 ) ;
#37277 = DIRECTION ( 'NONE',  ( 0.000000000000000000, 0.000000000000000000, 1.000000000000000000 ) ) ;
#37278 = VERTEX_POINT ( 'NONE', #43062 ) ;
#37280 = VERTEX_POINT ( 'NONE', #42336 ) ;
#37279 = AXIS2_PLACEMENT_3D ( 'NONE', #32213, #24621, #1623 ) ;
#37281 = AXIS2_PLACEMENT_3D ( 'NONE', #24141, #46175, #34657 ) ;
#37282 = EDGE_CURVE ( 'NONE', #22651, #41559, #31579, .T. ) ;
#37283 = DIRECTION ( 'NONE',  ( -1.000000000000000000, 0.000000000000000000, 0.000000000000000000 ) ) ;
#37284 = CARTESIAN_POINT ( 'NONE',  ( 22.94323693612312809, -114.6983135802921083, 5.500000000000000000 ) ) ;
#37286 = VERTEX_POINT ( 'NONE', #20790 ) ;
#37285 = LINE ( 'NONE', #36788, #8996 ) ;
#37287 = ADVANCED_FACE ( 'NONE', ( #38683 ), #35466, .T. ) ;
#37288 = ORIENTED_EDGE ( 'NONE', *, *, #9177, .F. ) ;
#37289 = DIRECTION ( 'NONE',  ( -0.08130631524010122069, 0.9966891607226784355, 0.000000000000000000 ) ) ;
#37290 = EDGE_CURVE ( 'NONE', #36459, #18078, #33617, .T. ) ;
#37291 = ORIENTED_EDGE ( 'NONE', *, *, #5698, .T. ) ;
#37292 = CIRCLE ( 'NONE', #22458, 31.99999999999998934 ) ;
#37293 = DIRECTION ( 'NONE',  ( 0.000000000000000000, 0.000000000000000000, 1.000000000000000000 ) ) ;
#37294 = DIRECTION ( 'NONE',  ( -1.000000000000000000, 0.000000000000000000, -0.000000000000000000 ) ) ;
#37295 = DIRECTION ( 'NONE',  ( 0.9227826878668540234, 0.3853207896976547087, 0.000000000000000000 ) ) ;
#37297 = DIRECTION ( 'NONE',  ( -1.000000000000000000, -0.000000000000000000, 0.000000000000000000 ) ) ;
#37296 = CIRCLE ( 'NONE', #16212, 37.49900000000000944 ) ;
#37298 = VERTEX_POINT ( 'NONE', #27914 ) ;
#37299 = DIRECTION ( 'NONE',  ( -1.000000000000000000, 0.000000000000000000, 0.000000000000000000 ) ) ;
#37300 = ORIENTED_EDGE ( 'NONE', *, *, #26148, .F. ) ;
#37301 = ORIENTED_EDGE ( 'NONE', *, *, #825, .T. ) ;
#37302 = DIRECTION ( 'NONE',  ( -0.000000000000000000, 0.1045284632676436315, 0.9945218953682742891 ) ) ;
#37303 = AXIS2_PLACEMENT_3D ( 'NONE', #24431, #9745, #43043 ) ;
#37304 = LINE ( 'NONE', #33618, #8987 ) ;
#37305 = DIRECTION ( 'NONE',  ( 0.000000000000000000, 0.000000000000000000, 1.000000000000000000 ) ) ;
#37306 = CARTESIAN_POINT ( 'NONE',  ( 5.999999999999999112, -68.55367621811110723, -44.99326035066126650 ) ) ;
#37307 = ORIENTED_EDGE ( 'NONE', *, *, #22937, .T. ) ;
#37308 = CARTESIAN_POINT ( 'NONE',  ( 11.99999999999999822, 55.38113227695858143, -54.21277698773617715 ) ) ;
#37309 = FACE_OUTER_BOUND ( 'NONE', #9228, .T. ) ;
#37310 = EDGE_CURVE ( 'NONE', #46337, #11996, #47594, .T. ) ;
#37311 = EDGE_CURVE ( 'NONE', #10700, #38800, #2406, .T. ) ;
#37312 = DIRECTION ( 'NONE',  ( -1.000000000000000000, 0.000000000000000000, 0.000000000000000000 ) ) ;
#37313 = CARTESIAN_POINT ( 'NONE',  ( 21.85433023846371370, -135.0628101570779620, 5.500000000000000000 ) ) ;
#37314 = DIRECTION ( 'NONE',  ( 0.000000000000000000, 0.000000000000000000, 1.000000000000000000 ) ) ;
#37315 = AXIS2_PLACEMENT_3D ( 'NONE', #42630, #9089, #27453 ) ;
#37316 = DIRECTION ( 'NONE',  ( -1.000000000000000000, -0.000000000000000000, -0.000000000000000000 ) ) ;
#37317 = DIRECTION ( 'NONE',  ( -1.000000000000000000, -0.000000000000000000, -0.000000000000000000 ) ) ;
#37318 = CYLINDRICAL_SURFACE ( 'NONE', #12273, 11.59999999999999787 ) ;
#37319 = DIRECTION ( 'NONE',  ( 0.000000000000000000, 0.000000000000000000, -1.000000000000000000 ) ) ;
#37320 = CARTESIAN_POINT ( 'NONE',  ( 10.00000000000000000, 55.20638768913760686, 51.02545421589343988 ) ) ;
#37321 = DIRECTION ( 'NONE',  ( -1.000000000000000000, 0.000000000000000000, 0.000000000000000000 ) ) ;
#37322 = EDGE_CURVE ( 'NONE', #13859, #32853, #5143, .T. ) ;
#37323 = VECTOR ( 'NONE', #36231, 1000.000000000000000 ) ;
#37324 = ORIENTED_EDGE ( 'NONE', *, *, #4644, .T. ) ;
#37325 = CARTESIAN_POINT ( 'NONE',  ( 3.250000000000000444, -13.95926121303099343, 0.000000000000000000 ) ) ;
#37326 = DIRECTION ( 'NONE',  ( -1.000000000000000000, -0.000000000000000000, -0.000000000000000000 ) ) ;
#37327 = DIRECTION ( 'NONE',  ( 1.000000000000000000, 0.000000000000000000, -0.000000000000000000 ) ) ;
#37328 = CARTESIAN_POINT ( 'NONE',  ( 10.00000000000000000, -37.48860685352290290, -0.8828120875904512665 ) ) ;
#37329 = CYLINDRICAL_SURFACE ( 'NONE', #7220, 37.49900000000000233 ) ;
#37330 = VERTEX_POINT ( 'NONE', #17335 ) ;
#37331 = EDGE_LOOP ( 'NONE', ( #12384, #11146, #34992, #31771 ) ) ;
#37332 = VECTOR ( 'NONE', #7624, 1000.000000000000000 ) ;
#37333 = ORIENTED_EDGE ( 'NONE', *, *, #39759, .T. ) ;
#37334 = AXIS2_PLACEMENT_3D ( 'NONE', #43527, #21001, #2389 ) ;
#37335 = CARTESIAN_POINT ( 'NONE',  ( 0.000000000000000000, 73.95703589263973754, 23.16143007188453851 ) ) ;
#37336 = ORIENTED_EDGE ( 'NONE', *, *, #18574, .T. ) ;
#37337 = EDGE_CURVE ( 'NONE', #10502, #2146, #5619, .T. ) ;
#37338 = VECTOR ( 'NONE', #659, 1000.000000000000000 ) ;
#37339 = CARTESIAN_POINT ( 'NONE',  ( -25.00516449930816876, -111.2255058058861010, -2.500000000000000000 ) ) ;
#37340 = FACE_OUTER_BOUND ( 'NONE', #44210, .T. ) ;
#37341 = DIRECTION ( 'NONE',  ( -1.000000000000000000, 0.000000000000000000, 0.000000000000000000 ) ) ;
#37342 = ADVANCED_FACE ( 'NONE', ( #12974 ), #42828, .T. ) ;
#37343 = EDGE_LOOP ( 'NONE', ( #15553, #24483, #32011, #30775 ) ) ;
#37344 = CARTESIAN_POINT ( 'NONE',  ( -3.702536634196121224, 8.043911037661892749, -64.01812422950395387 ) ) ;
#37345 = EDGE_LOOP ( 'NONE', ( #20966, #35471, #32757, #4427 ) ) ;
#37346 = EDGE_CURVE ( 'NONE', #34171, #44060, #9514, .T. ) ;
#37347 = VERTEX_POINT ( 'NONE', #28843 ) ;
#37348 = DIRECTION ( 'NONE',  ( -1.000000000000000000, 0.000000000000000000, 0.000000000000000000 ) ) ;
#37349 = CARTESIAN_POINT ( 'NONE',  ( 10.00000000000000000, -37.22597642581153821, -5.202137450156795850 ) ) ;
#37350 = CIRCLE ( 'NONE', #41274, 31.99999999999999289 ) ;
#37351 = FACE_BOUND ( 'NONE', #48257, .T. ) ;
#37352 = ORIENTED_EDGE ( 'NONE', *, *, #23312, .F. ) ;
#37353 = EDGE_LOOP ( 'NONE', ( #31172, #39875, #45161, #43234 ) ) ;
#37354 = ORIENTED_EDGE ( 'NONE', *, *, #882, .F. ) ;
#37355 = CARTESIAN_POINT ( 'NONE',  ( 15.00000000000000000, 22.07842321921480888, -8.187992925817425771 ) ) ;
#37356 = ORIENTED_EDGE ( 'NONE', *, *, #23542, .T. ) ;
#37357 = DIRECTION ( 'NONE',  ( 0.000000000000000000, 0.9876883405951372152, 0.1564344650402346160 ) ) ;
#37358 = DIRECTION ( 'NONE',  ( -1.000000000000000000, 0.000000000000000000, 0.000000000000000000 ) ) ;
#37359 = CARTESIAN_POINT ( 'NONE',  ( 10.00000000000000000, -31.46837873494930093, -68.27212725128309501 ) ) ;
#37360 = CARTESIAN_POINT ( 'NONE',  ( -6.880223345695647197, -142.5202692415819854, 5.500000000000000000 ) ) ;
#37361 = DIRECTION ( 'NONE',  ( -1.000000000000000000, -0.000000000000000000, 0.000000000000000000 ) ) ;
#37362 = FACE_OUTER_BOUND ( 'NONE', #439, .T. ) ;
#37363 = CARTESIAN_POINT ( 'NONE',  ( 15.00000000000000000, -11.95096189432345746, -23.69967320028757030 ) ) ;
#37364 = EDGE_CURVE ( 'NONE', #33288, #43680, #18664, .T. ) ;
#37365 = EDGE_CURVE ( 'NONE', #42351, #41545, #706, .T. ) ;
#37366 = CARTESIAN_POINT ( 'NONE',  ( 10.00000000000000000, -16.45098606841149902, 33.79645857604508308 ) ) ;
#37367 = FACE_OUTER_BOUND ( 'NONE', #37468, .T. ) ;
#37368 = DIRECTION ( 'NONE',  ( 0.000000000000000000, 0.000000000000000000, 1.000000000000000000 ) ) ;
#37369 = AXIS2_PLACEMENT_3D ( 'NONE', #42612, #19826, #2205 ) ;
#37370 = ORIENTED_EDGE ( 'NONE', *, *, #25689, .F. ) ;
#37371 = EDGE_CURVE ( 'NONE', #21081, #40538, #6341, .T. ) ;
#37372 = LINE ( 'NONE', #8473, #35865 ) ;
#37373 = EDGE_LOOP ( 'NONE', ( #34722, #466, #34793, #6418 ) ) ;
#37374 = VECTOR ( 'NONE', #10840, 1000.000000000000000 ) ;
#37375 = DIRECTION ( 'NONE',  ( -1.000000000000000000, -0.000000000000000000, 0.000000000000000000 ) ) ;
#37376 = ORIENTED_EDGE ( 'NONE', *, *, #6821, .F. ) ;
#37377 = DIRECTION ( 'NONE',  ( 1.000000000000000000, 0.000000000000000000, -0.000000000000000000 ) ) ;
#37378 = CARTESIAN_POINT ( 'NONE',  ( 10.00000000000000000, 46.53671651294032330, -59.03961581697353012 ) ) ;
#37379 = CIRCLE ( 'NONE', #36596, 77.49900000000000944 ) ;
#37380 = LINE ( 'NONE', #36879, #17710 ) ;
#37381 = DIRECTION ( 'NONE',  ( -1.000000000000000000, -0.000000000000000000, -0.000000000000000000 ) ) ;
#37382 = EDGE_CURVE ( 'NONE', #22127, #19593, #39819, .T. ) ;
#37383 = DIRECTION ( 'NONE',  ( -1.000000000000000000, -0.000000000000000000, 0.000000000000000000 ) ) ;
#37384 = DIRECTION ( 'NONE',  ( -1.000000000000000000, -0.000000000000000000, -0.000000000000000000 ) ) ;
#37385 = CARTESIAN_POINT ( 'NONE',  ( -18.12185313557660038, -104.9634299478706794, 5.500000000000000000 ) ) ;
#37386 = COLOUR_RGB ( '', 0.40784314, 0.44705882, 0.49803922) ;
#37387 =( NAMED_UNIT ( * ) SI_UNIT ( $, .STERADIAN. ) SOLID_ANGLE_UNIT ( ) );
#37388 = DIRECTION ( 'NONE',  ( 0.000000000000000000, -0.7604059656000368150, 0.6494480483301767748 ) ) ;
#37389 = VERTEX_POINT ( 'NONE', #48172 ) ;
#37390 = CIRCLE ( 'NONE', #6925, 11.59999999999999787 ) ;
#37391 = ORIENTED_EDGE ( 'NONE', *, *, #24377, .T. ) ;
#37392 = ORIENTED_EDGE ( 'NONE', *, *, #3796, .T. ) ;
#37393 = DIRECTION ( 'NONE',  ( 1.000000000000000000, -0.000000000000000000, 0.000000000000000000 ) ) ;
#37394 = CARTESIAN_POINT ( 'NONE',  ( 1.355716935723751293, -120.6418968688129496, 2.500000000000000000 ) ) ;
#37395 = DIRECTION ( 'NONE',  ( 0.000000000000000000, 0.000000000000000000, 1.000000000000000000 ) ) ;
#37397 = ADVANCED_FACE ( 'NONE', ( #32993 ), #47917, .F. ) ;
#37396 = AXIS2_PLACEMENT_3D ( 'NONE', #35424, #16585, #12440 ) ;
#37398 = ORIENTED_EDGE ( 'NONE', *, *, #17835, .F. ) ;
#37399 = EDGE_LOOP ( 'NONE', ( #40123, #13897, #6919, #42786 ) ) ;
#37400 = AXIS2_PLACEMENT_3D ( 'NONE', #4341, #19472, #15102 ) ;
#37401 = EDGE_CURVE ( 'NONE', #9856, #39253, #28833, .T. ) ;
#37402 = EDGE_CURVE ( 'NONE', #36037, #27530, #24158, .T. ) ;
#37403 = DIRECTION ( 'NONE',  ( -1.000000000000000000, 0.000000000000000000, -0.000000000000000000 ) ) ;
#37404 = DIRECTION ( 'NONE',  ( -1.000000000000000000, 0.000000000000000000, -0.000000000000000000 ) ) ;
#37405 = ADVANCED_FACE ( 'NONE', ( #29571 ), #18056, .F. ) ;
#37406 = DIRECTION ( 'NONE',  ( 0.8541291221503261033, -0.5200609990133016058, 0.000000000000000000 ) ) ;
#37407 = ORIENTED_EDGE ( 'NONE', *, *, #36530, .F. ) ;
#37408 = DIRECTION ( 'NONE',  ( -1.000000000000000000, -0.000000000000000000, 0.000000000000000000 ) ) ;
#37409 = EDGE_CURVE ( 'NONE', #30376, #33522, #25706, .T. ) ;
#37410 = ORIENTED_EDGE ( 'NONE', *, *, #23369, .T. ) ;
#37411 = CARTESIAN_POINT ( 'NONE',  ( -3.000000000000000000, -26.23277895567245821, -4.042438405570103477 ) ) ;
#37412 = CARTESIAN_POINT ( 'NONE',  ( 0.000000000000000000, -77.32052557432837148, -5.256550761633697277 ) ) ;
#37413 = PRODUCT_DEFINITION_FORMATION_WITH_SPECIFIED_SOURCE ( 'ANY', '', #36283, .NOT_KNOWN. ) ;
#37414 = CARTESIAN_POINT ( 'NONE',  ( 10.00000000000000000, -71.87247863392384772, -39.47590169984921005 ) ) ;
#37415 = ORIENTED_EDGE ( 'NONE', *, *, #17040, .T. ) ;
#37416 = ORIENTED_EDGE ( 'NONE', *, *, #25059, .T. ) ;
#37417 = VERTEX_POINT ( 'NONE', #22234 ) ;
#37418 = EDGE_CURVE ( 'NONE', #15863, #39100, #42150, .T. ) ;
#37419 = AXIS2_PLACEMENT_3D ( 'NONE', #24255, #2004, #2454 ) ;
#37420 = DIRECTION ( 'NONE',  ( -1.000000000000000000, 0.000000000000000000, -0.000000000000000000 ) ) ;
#37421 = FACE_OUTER_BOUND ( 'NONE', #18257, .T. ) ;
#37422 = EDGE_LOOP ( 'NONE', ( #3122, #7369, #2066, #45291 ) ) ;
#37423 = VERTEX_POINT ( 'NONE', #3625 ) ;
#37424 = EDGE_CURVE ( 'NONE', #21091, #37774, #45265, .T. ) ;
#37425 = DIRECTION ( 'NONE',  ( 0.000000000000000000, 0.000000000000000000, 1.000000000000000000 ) ) ;
#37426 = ORIENTED_EDGE ( 'NONE', *, *, #16272, .F. ) ;
#37427 = CARTESIAN_POINT ( 'NONE',  ( 11.99999999999999822, 65.58780272294076497, 36.73666225445916211 ) ) ;
#37428 = DIRECTION ( 'NONE',  ( -1.000000000000000000, 0.000000000000000000, 0.000000000000000000 ) ) ;
#37429 = DIRECTION ( 'NONE',  ( -1.000000000000000000, 0.000000000000000000, 0.000000000000000000 ) ) ;
#37430 = CARTESIAN_POINT ( 'NONE',  ( 5.000000000000000000, -32.34446384429989507, 26.79245525562703278 ) ) ;
#37431 = LINE ( 'NONE', #33276, #34620 ) ;
#37432 = DIRECTION ( 'NONE',  ( 0.000000000000000000, 0.000000000000000000, -1.000000000000000000 ) ) ;
#37433 = FACE_OUTER_BOUND ( 'NONE', #5899, .T. ) ;
#37434 = EDGE_CURVE ( 'NONE', #8908, #11885, #47449, .T. ) ;
#37435 = CARTESIAN_POINT ( 'NONE',  ( 10.00000000000000000, -37.48860685352290290, -0.8828120875904512665 ) ) ;
#37436 = VECTOR ( 'NONE', #1705, 1000.000000000000000 ) ;
#37437 = LINE ( 'NONE', #48210, #1196 ) ;
#37438 = ORIENTED_EDGE ( 'NONE', *, *, #5997, .F. ) ;
#37439 = CIRCLE ( 'NONE', #8496, 82.00000000000000000 ) ;
#37440 = DIRECTION ( 'NONE',  ( 0.000000000000000000, 0.000000000000000000, 1.000000000000000000 ) ) ;
#37441 = AXIS2_PLACEMENT_3D ( 'NONE', #44711, #38337, #155 ) ;
#37442 = CARTESIAN_POINT ( 'NONE',  ( 0.000000000000000000, 18.89407956138256139, 75.16055320797038064 ) ) ;
#37443 = AXIS2_PLACEMENT_3D ( 'NONE', #20925, #28513, #2540 ) ;
#37444 = DIRECTION ( 'NONE',  ( 0.000000000000000000, -0.5877852522924779111, -0.8090169943749440096 ) ) ;
#37445 = VERTEX_POINT ( 'NONE', #13918 ) ;
#37446 = EDGE_CURVE ( 'NONE', #19570, #2942, #13688, .T. ) ;
#37447 = PRODUCT_DEFINITION_CONTEXT ( 'detailed design', #29133, 'design' ) ;
#37448 = CARTESIAN_POINT ( 'NONE',  ( 10.00000000000000000, 10.41901085202078114, 40.68715046381932865 ) ) ;
#37449 = AXIS2_PLACEMENT_3D ( 'NONE', #1686, #17565, #12700 ) ;
#37450 = CARTESIAN_POINT ( 'NONE',  ( -10.00000000000000000, 0.000000000000000000, 0.000000000000000000 ) ) ;
#37451 = DIRECTION ( 'NONE',  ( 0.000000000000000000, 0.9510565162951504226, -0.3090169943749573322 ) ) ;
#37452 = VERTEX_POINT ( 'NONE', #36185 ) ;
#37453 = COLOUR_RGB ( '', 0.09019608, 0.27058824, 0.51372549) ;
#37454 = ORIENTED_EDGE ( 'NONE', *, *, #13923, .T. ) ;
#37455 = EDGE_CURVE ( 'NONE', #1792, #16097, #7733, .T. ) ;
#37456 = CARTESIAN_POINT ( 'NONE',  ( 0.000000000000000000, 0.000000000000000000, 0.000000000000000000 ) ) ;
#37457 = EDGE_LOOP ( 'NONE', ( #19960, #634, #24657, #27067 ) ) ;
#37458 = VERTEX_POINT ( 'NONE', #21249 ) ;
#37459 = EDGE_CURVE ( 'NONE', #46408, #31210, #43546, .T. ) ;
#37460 = ORIENTED_EDGE ( 'NONE', *, *, #12889, .T. ) ;
#37461 = VERTEX_POINT ( 'NONE', #24934 ) ;
#37462 = CARTESIAN_POINT ( 'NONE',  ( -10.00000000000000000, 0.000000000000000000, 0.000000000000000000 ) ) ;
#37463 = EDGE_CURVE ( 'NONE', #26870, #10088, #17820, .T. ) ;
#37464 = AXIS2_PLACEMENT_3D ( 'NONE', #19123, #534, #37491 ) ;
#37465 = DIRECTION ( 'NONE',  ( 0.000000000000000000, -0.7071067811865537900, 0.7071067811865413555 ) ) ;
#37466 = VECTOR ( 'NONE', #41744, 1000.000000000000000 ) ;
#37467 = ADVANCED_FACE ( 'NONE', ( #25162 ), #32748, .T. ) ;
#37468 = EDGE_LOOP ( 'NONE', ( #45516, #42309, #30291, #42054 ) ) ;
#37469 = PLANE ( 'NONE',  #22810 ) ;
#37470 = ORIENTED_EDGE ( 'NONE', *, *, #42255, .F. ) ;
#37471 = CIRCLE ( 'NONE', #20242, 82.00000000000000000 ) ;
#37472 = CARTESIAN_POINT ( 'NONE',  ( 10.00000000000000000, -40.68715046381937128, 10.41901085202062660 ) ) ;
#37473 = LINE ( 'NONE', #33781, #10305 ) ;
#37474 = EDGE_LOOP ( 'NONE', ( #14227, #5859, #16757, #19889 ) ) ;
#37475 = ORIENTED_EDGE ( 'NONE', *, *, #8824, .F. ) ;
#37476 = CARTESIAN_POINT ( 'NONE',  ( 0.000000000000000000, -71.27951684758046724, 30.41916302227088309 ) ) ;
#37477 = CYLINDRICAL_SURFACE ( 'NONE', #15364, 16.00000000000000000 ) ;
#37478 = VERTEX_POINT ( 'NONE', #22703 ) ;
#37480 = ORIENTED_EDGE ( 'NONE', *, *, #3177, .F. ) ;
#37479 = DIRECTION ( 'NONE',  ( 0.000000000000000000, 0.000000000000000000, 1.000000000000000000 ) ) ;
#37481 = CARTESIAN_POINT ( 'NONE',  ( -43.60332556124591719, -117.0000000000000000, 2.500000000000000000 ) ) ;
#37482 = ORIENTED_EDGE ( 'NONE', *, *, #5182, .F. ) ;
#37483 = CARTESIAN_POINT ( 'NONE',  ( 5.000000000000000000, 31.52238457039637609, -27.75498641678709788 ) ) ;
#37484 = AXIS2_PLACEMENT_3D ( 'NONE', #37047, #2367, #44399 ) ;
#37485 = EDGE_LOOP ( 'NONE', ( #21521, #3862, #20195, #27680 ) ) ;
#37486 = DIRECTION ( 'NONE',  ( 1.000000000000000000, 0.000000000000000000, -0.000000000000000000 ) ) ;
#37487 = DIRECTION ( 'NONE',  ( 0.9730327541852493711, -0.2306669878475637314, 0.000000000000000000 ) ) ;
#37488 = DIRECTION ( 'NONE',  ( 0.9827303690289282967, 0.1850432970638667407, -0.000000000000000000 ) ) ;
#37489 = CARTESIAN_POINT ( 'NONE',  ( 11.99999999999999822, 0.000000000000000000, 0.000000000000000000 ) ) ;
#37490 = CARTESIAN_POINT ( 'NONE',  ( 0.000000000000000000, -40.68715046381921496, -10.41901085202121280 ) ) ;
#37491 = DIRECTION ( 'NONE',  ( 0.000000000000000000, 0.1564344650402244852, 0.9876883405951387696 ) ) ;
#37492 = CARTESIAN_POINT ( 'NONE',  ( 15.00000000000000000, 23.49999999999999645, -1.500000000000003997 ) ) ;
#37493 = DIRECTION ( 'NONE',  ( 0.000000000000000000, 0.000000000000000000, -1.000000000000000000 ) ) ;
#37494 = ORIENTED_EDGE ( 'NONE', *, *, #13604, .F. ) ;
#37495 = CARTESIAN_POINT ( 'NONE',  ( 0.000000000000000000, 22.74946021919175720, -29.81001611430984255 ) ) ;
#37496 = DIRECTION ( 'NONE',  ( 0.000000000000000000, 0.4067366430758009854, -0.9135454576426004225 ) ) ;
#37497 = FACE_OUTER_BOUND ( 'NONE', #33424, .T. ) ;
#37498 = LINE ( 'NONE', #18877, #37205 ) ;
#37499 = FACE_OUTER_BOUND ( 'NONE', #26467, .T. ) ;
#37500 = PLANE ( 'NONE',  #19051 ) ;
#37501 = LINE ( 'NONE', #44368, #37374 ) ;
#37502 = CARTESIAN_POINT ( 'NONE',  ( 11.99999999999999822, -59.46389618801929089, -49.70050353004953081 ) ) ;
#37503 = ORIENTED_EDGE ( 'NONE', *, *, #3993, .F. ) ;
#37504 = VECTOR ( 'NONE', #41358, 1000.000000000000000 ) ;
#37505 = CARTESIAN_POINT ( 'NONE',  ( 0.000000000000000000, 3.925862922256160736, 41.81611651403863306 ) ) ;
#37506 = AXIS2_PLACEMENT_3D ( 'NONE', #29213, #14045, #10367 ) ;
#37507 = EDGE_LOOP ( 'NONE', ( #27238, #8002, #40049, #18514 ) ) ;
#37508 = CARTESIAN_POINT ( 'NONE',  ( 0.000000000000000000, -60.67117009219098378, -55.16347631943106933 ) ) ;
#37509 = DIRECTION ( 'NONE',  ( 0.9927274188295609481, 0.1203838523390816373, -2.034265265314174749E-17 ) ) ;
#37510 = CARTESIAN_POINT ( 'NONE',  ( 10.00000000000000000, -60.67117009219097667, -55.16347631943105512 ) ) ;
#37511 = EDGE_LOOP ( 'NONE', ( #40767, #35417, #1245, #11721 ) ) ;
#37512 = AXIS2_PLACEMENT_3D ( 'NONE', #32131, #9357, #35556 ) ;
#37513 = ADVANCED_FACE ( 'NONE', ( #8266 ), #37642, .T. ) ;
#37514 = DIRECTION ( 'NONE',  ( -1.000000000000000000, -0.000000000000000000, -0.000000000000000000 ) ) ;
#37515 = ORIENTED_EDGE ( 'NONE', *, *, #6405, .F. ) ;
#37516 = ADVANCED_FACE ( 'NONE', ( #44735 ), #4367, .T. ) ;
#37517 = DIRECTION ( 'NONE',  ( -1.000000000000000000, -0.000000000000000000, -0.000000000000000000 ) ) ;
#37518 = ADVANCED_FACE ( 'NONE', ( #41322 ), #19026, .F. ) ;
#37519 = CARTESIAN_POINT ( 'NONE',  ( 11.99999999999999822, 30.41916302227114599, 71.27951684758035356 ) ) ;
#37520 = SHAPE_REPRESENTATION ( 'slow gear_ISO - Spur gear 2M 80T 20PA 12FW ---S80A75H50L38.0N', ( #11636 ), #21023 ) ;
#37522 = EDGE_LOOP ( 'NONE', ( #23738, #3305, #34366, #5544 ) ) ;
#37521 = CYLINDRICAL_SURFACE ( 'NONE', #15304, 77.49899999999999523 ) ;
#37523 = VERTEX_POINT ( 'NONE', #26623 ) ;
#37524 = EDGE_CURVE ( 'NONE', #47099, #45945, #42044, .T. ) ;
#37525 = ORIENTED_EDGE ( 'NONE', *, *, #22104, .F. ) ;
#37526 = CARTESIAN_POINT ( 'NONE',  ( -10.00000000000000000, 0.000000000000000000, 0.000000000000000000 ) ) ;
#37527 = DIRECTION ( 'NONE',  ( -1.000000000000000000, 0.000000000000000000, 0.000000000000000000 ) ) ;
#37528 = LINE ( 'NONE', #18912, #15776 ) ;
#37529 = CIRCLE ( 'NONE', #16437, 82.00000000000000000 ) ;
#37530 = DIRECTION ( 'NONE',  ( 0.000000000000000000, 0.000000000000000000, 1.000000000000000000 ) ) ;
#37531 = ORIENTED_EDGE ( 'NONE', *, *, #15630, .T. ) ;
#37532 = VECTOR ( 'NONE', #8144, 1000.000000000000000 ) ;
#37533 = CARTESIAN_POINT ( 'NONE',  ( 0.000000000000000000, -41.81611651403864727, 3.925862922256025289 ) ) ;
#37534 = ORIENTED_EDGE ( 'NONE', *, *, #30913, .F. ) ;
#37535 = VERTEX_POINT ( 'NONE', #30311 ) ;
#37536 = DIRECTION ( 'NONE',  ( 0.000000000000000000, 0.3090169943749411785, 0.9510565162951556406 ) ) ;
#37537 = CIRCLE ( 'NONE', #25816, 14.09999999999999964 ) ;
#37538 = AXIS2_PLACEMENT_3D ( 'NONE', #7840, #4654, #11762 ) ;
#37539 = EDGE_CURVE ( 'NONE', #44846, #21976, #30060, .T. ) ;
#37540 = FACE_OUTER_BOUND ( 'NONE', #45633, .T. ) ;
#37541 = DIRECTION ( 'NONE',  ( 1.000000000000000000, 0.000000000000000000, 0.000000000000000000 ) ) ;
#37542 = CARTESIAN_POINT ( 'NONE',  ( 10.00000000000000000, 0.000000000000000000, 0.000000000000000000 ) ) ;
#37543 = ORIENTED_EDGE ( 'NONE', *, *, #13116, .T. ) ;
#37544 = CARTESIAN_POINT ( 'NONE',  ( 5.000000000000000000, -27.75498641678720446, -31.52238457039628727 ) ) ;
#37545 = CARTESIAN_POINT ( 'NONE',  ( 10.00000000000000000, 0.000000000000000000, 0.000000000000000000 ) ) ;
#37546 = AXIS2_PLACEMENT_3D ( 'NONE', #31648, #17162, #32118 ) ;
#37547 = LINE ( 'NONE', #21886, #36783 ) ;
#37548 = CIRCLE ( 'NONE', #1, 42.00000000000000000 ) ;
#37549 = DIRECTION ( 'NONE',  ( -0.1850432970638682395, 0.9827303690289280746, 0.000000000000000000 ) ) ;
#37550 = DIRECTION ( 'NONE',  ( -1.000000000000000000, 0.000000000000000000, 0.000000000000000000 ) ) ;
#37551 = CIRCLE ( 'NONE', #7841, 31.99999999999999289 ) ;
#37552 = CARTESIAN_POINT ( 'NONE',  ( 5.000000000000002665, 10.30890764327501863, -81.34940948281325745 ) ) ;
#37553 = PLANE ( 'NONE',  #9941 ) ;
#37554 = DIRECTION ( 'NONE',  ( -1.000000000000000000, 0.000000000000000000, 0.000000000000000000 ) ) ;
#37555 = CARTESIAN_POINT ( 'NONE',  ( 11.99999999999999822, 0.000000000000000000, 0.000000000000000000 ) ) ;
#37556 = DIRECTION ( 'NONE',  ( -1.000000000000000000, 0.000000000000000000, 0.000000000000000000 ) ) ;
#37557 = DIRECTION ( 'NONE',  ( -0.9827303690289279636, -0.1850432970638682117, 0.000000000000000000 ) ) ;
#37558 = ORIENTED_EDGE ( 'NONE', *, *, #41564, .T. ) ;
#37559 = EDGE_CURVE ( 'NONE', #1488, #32651, #30535, .T. ) ;
#37560 = DIRECTION ( 'NONE',  ( 1.000000000000000000, 0.000000000000000000, 0.000000000000000000 ) ) ;
#37561 = DIRECTION ( 'NONE',  ( 2.889240119132116694E-16, -1.000000000000000000, 0.000000000000000000 ) ) ;
#37562 = DIRECTION ( 'NONE',  ( -0.000000000000000000, -0.000000000000000000, -1.000000000000000000 ) ) ;
#37563 = CARTESIAN_POINT ( 'NONE',  ( 0.000000000000000000, 30.41916302227114599, 71.27951684758035356 ) ) ;
#37564 = ADVANCED_FACE ( 'NONE', ( #41557 ), #33955, .T. ) ;
#37565 = EDGE_CURVE ( 'NONE', #18579, #7117, #13982, .T. ) ;
#37566 = CARTESIAN_POINT ( 'NONE',  ( 0.000000000000000000, -62.20884554313985149, -46.21855187248698371 ) ) ;
#37567 = ORIENTED_EDGE ( 'NONE', *, *, #37539, .T. ) ;
#37568 = ORIENTED_EDGE ( 'NONE', *, *, #47183, .F. ) ;
#37569 = VECTOR ( 'NONE', #37063, 1000.000000000000000 ) ;
#37570 = AXIS2_PLACEMENT_3D ( 'NONE', #20602, #21574, #6647 ) ;
#37571 = CIRCLE ( 'NONE', #36030, 77.49899999999999523 ) ;
#37572 = AXIS2_PLACEMENT_3D ( 'NONE', #3934, #29631, #45286 ) ;
#37573 = DIRECTION ( 'NONE',  ( 0.000000000000000000, -0.2079116908177533474, 0.9781476007338069101 ) ) ;
#37574 = ADVANCED_FACE ( 'NONE', ( #45457 ), #22479, .T. ) ;
#37575 = EDGE_LOOP ( 'NONE', ( #18774, #11845, #38797, #22425 ) ) ;
#37576 = AXIS2_PLACEMENT_3D ( 'NONE', #4197, #37965, #40916 ) ;
#37577 = EDGE_CURVE ( 'NONE', #42453, #42302, #24925, .T. ) ;
#37578 = EDGE_CURVE ( 'NONE', #25169, #4138, #15384, .T. ) ;
#37579 = VECTOR ( 'NONE', #6904, 1000.000000000000000 ) ;
#37580 = CARTESIAN_POINT ( 'NONE',  ( 11.99999999999999822, -73.73191006444561424, -14.66109333815538918 ) ) ;
#37581 = AXIS2_PLACEMENT_3D ( 'NONE', #46220, #23952, #17072 ) ;
#37582 = CARTESIAN_POINT ( 'NONE',  ( 10.00000000000000000, 0.000000000000000000, 0.000000000000000000 ) ) ;
#37583 = DIRECTION ( 'NONE',  ( 0.000000000000000000, 0.000000000000000000, 1.000000000000000000 ) ) ;
#37584 = ORIENTED_EDGE ( 'NONE', *, *, #17008, .T. ) ;
#37585 = CARTESIAN_POINT ( 'NONE',  ( -3.000000000000000000, 6.762365576493643893, -25.66652317338391853 ) ) ;
#37586 = ORIENTED_EDGE ( 'NONE', *, *, #44712, .T. ) ;
#37587 = ORIENTED_EDGE ( 'NONE', *, *, #2535, .F. ) ;
#37588 = VERTEX_POINT ( 'NONE', #4832 ) ;
#37589 = FACE_OUTER_BOUND ( 'NONE', #13078, .T. ) ;
#37590 = DIRECTION ( 'NONE',  ( 0.000000000000000000, -0.4999999999999920064, -0.8660254037844432595 ) ) ;
#37591 = CARTESIAN_POINT ( 'NONE',  ( 0.000000000000000000, -8.840884882375609877, 74.65374052328647281 ) ) ;
#37592 = EDGE_LOOP ( 'NONE', ( #41672, #41293, #14911, #19128 ) ) ;
#37593 = ORIENTED_EDGE ( 'NONE', *, *, #16344, .F. ) ;
#37594 = ORIENTED_EDGE ( 'NONE', *, *, #14608, .T. ) ;
#37595 = DIRECTION ( 'NONE',  ( -1.000000000000000000, 0.000000000000000000, 0.000000000000000000 ) ) ;
#37596 = ORIENTED_EDGE ( 'NONE', *, *, #3140, .F. ) ;
#37597 = CARTESIAN_POINT ( 'NONE',  ( 12.00000000000000000, -18.13022148937263012, -15.02647892043543898 ) ) ;
#37598 = FACE_OUTER_BOUND ( 'NONE', #45580, .T. ) ;
#37599 = CYLINDRICAL_SURFACE ( 'NONE', #43237, 82.00000000000000000 ) ;
#37600 = DIRECTION ( 'NONE',  ( -1.000000000000000000, 0.000000000000000000, 0.000000000000000000 ) ) ;
#37601 = CARTESIAN_POINT ( 'NONE',  ( 11.99999999999999822, 73.95703589263975175, 23.16143007188452785 ) ) ;
#37602 = CYLINDRICAL_SURFACE ( 'NONE', #7273, 37.49900000000000233 ) ;
#37603 = CARTESIAN_POINT ( 'NONE',  ( 0.000000000000000000, -120.0000000000000000, 2.500000000000000000 ) ) ;
#37604 = DIRECTION ( 'NONE',  ( 0.000000000000000000, -0.000000000000000000, 1.000000000000000000 ) ) ;
#37605 = DIRECTION ( 'NONE',  ( -1.000000000000000000, 0.000000000000000000, 0.000000000000000000 ) ) ;
#37606 = ORIENTED_EDGE ( 'NONE', *, *, #35461, .F. ) ;
#37607 = AXIS2_PLACEMENT_3D ( 'NONE', #1262, #4683, #27689 ) ;
#37608 = DIRECTION ( 'NONE',  ( 1.000000000000000000, -0.000000000000000000, 0.000000000000000000 ) ) ;
#37609 = EDGE_LOOP ( 'NONE', ( #19543, #41988, #30835, #41044, #36091, #47915, #18611, #37059, #24672, #46277, #12000, #15078, #6052, #10807, #35884, #17331, #26456, #2032, #41978, #10565, #37709, #7882, #41997, #4231, #34319, #15446, #26222, #16295, #33730, #40313, #41920, #24382, #9360, #37148, #9138, #34067, #2544, #38247, #38744, #6621, #11216, #8844, #24616, #42047, #36435, #732, #19261, #2091, #11369, #41913, #8286, #6995, #37307, #23993, #30882, #8347, #11466, #10731, #6396, #23731, #39102, #21128, #42219, #1810, #36987, #25153, #38545, #10327, #31911, #39504, #17952, #28391, #28781, #10884, #38138, #31012, #9366, #22260, #34683, #42718, #23958, #9633, #32065, #12313, #26206, #41948, #35597, #26360, #21196, #40633, #46860, #27558, #34377, #30617, #22804, #9975, #2138, #32164, #8208, #5484, #3636, #1243, #621, #24601, #23484, #46375, #17944, #17901, #9284, #13866, #11411, #21396, #36919, #30370, #25857, #36510, #47511, #8162, #16982, #22632, #16346, #34161, #27482, #33324, #13737, #4332, #27342, #8549, #36690, #1490, #6295, #20962, #33720, #5873, #9521, #19852, #30706, #39106, #26374, #7655, #9942, #26853, #47287, #8809, #17396, #35227, #11294, #32027, #41580, #13234, #47681, #7962, #11264, #34668, #42759, #25727, #43767, #36181, #8152, #8202, #15002, #28018, #16892, #25642, #35894, #24214, #44006, #9479, #40560, #19293, #38786, #40113, #10135, #23102, #11764, #39694, #25238, #312, #17088, #9877, #6722, #19792, #38317, #5823, #1185, #37880, #32817, #19176, #40784, #31351, #31228, #9595, #39995, #11226, #8778, #38678, #22451, #24119, #9530, #17047, #41924, #1100, #27141, #26697, #4656, #20761, #27794, #39210, #46020, #29429, #25252, #10973, #14913, #33521, #19771, #36670, #16561, #46735, #19220, #32550, #35133, #14631, #4934, #9358, #12427, #34601, #25005, #16398, #43884, #44993, #46766, #10401, #31048, #27200, #44680, #13035, #22769, #6012, #31916, #6086, #12654, #28767, #36847, #22765, #16125, #44760, #10307, #438, #30143, #24947, #23660, #22160, #6409, #35899, #42108, #20133, #41621, #16407, #20844, #12551, #20427, #24403, #44284, #19404, #22903, #30122, #3884, #26142, #15182, #38985, #46130, #32563, #28258, #24974, #3086, #24448, #23717, #23503, #1515, #46218, #9973, #7043, #9041, #20647, #39033, #8682, #33926, #44374, #28556, #34015, #32402, #14721, #5840, #42585, #10864, #17322, #25656, #16846, #47852, #30084, #44819, #22576, #42943, #853, #22121, #503, #48399, #31103, #39826, #3124, #47139, #29363, #14297, #33540, #11378, #17648, #2399, #12413, #42418, #11650, #30530, #40270, #17211, #26524, #21028 ) ) ;
#37610 = EDGE_LOOP ( 'NONE', ( #12859, #25002, #37828, #38598 ) ) ;
#37611 = AXIS2_PLACEMENT_3D ( 'NONE', #7001, #3574, #32942 ) ;
#37612 = DIRECTION ( 'NONE',  ( -1.000000000000000000, -0.000000000000000000, 0.000000000000000000 ) ) ;
#37613 = CIRCLE ( 'NONE', #16507, 37.49900000000000233 ) ;
#37614 = AXIS2_PLACEMENT_3D ( 'NONE', #34496, #8556, #46260 ) ;
#37615 = FACE_OUTER_BOUND ( 'NONE', #15400, .T. ) ;
#37616 = DIRECTION ( 'NONE',  ( -0.9997280174009349762, 0.02332147558787671729, 0.000000000000000000 ) ) ;
#37617 = CARTESIAN_POINT ( 'NONE',  ( -11.68233973192911535, 0.000000000000000000, -17.37152077436032371 ) ) ;
#37618 = AXIS2_PLACEMENT_3D ( 'NONE', #13711, #14907, #48424 ) ;
#37619 = AXIS2_PLACEMENT_3D ( 'NONE', #36693, #5901, #32318 ) ;
#37620 = CARTESIAN_POINT ( 'NONE',  ( 10.00000000000000000, -5.202137450156129717, -37.22597642581163768 ) ) ;
#37621 = VERTEX_POINT ( 'NONE', #4592 ) ;
#37622 = EDGE_CURVE ( 'NONE', #38863, #960, #33478, .T. ) ;
#37623 = CARTESIAN_POINT ( 'NONE',  ( 12.00000000000000000, -19.89357724624986901, 12.59942793731086219 ) ) ;
#37624 = VECTOR ( 'NONE', #3836, 1000.000000000000000 ) ;
#37625 = CARTESIAN_POINT ( 'NONE',  ( -3.000000000000000000, 23.50000000000000000, -1.500000000000001332 ) ) ;
#37626 = EDGE_CURVE ( 'NONE', #37278, #25452, #26504, .T. ) ;
#37627 = LINE ( 'NONE', #46614, #8912 ) ;
#37628 =( NAMED_UNIT ( * ) SI_UNIT ( $, .STERADIAN. ) SOLID_ANGLE_UNIT ( ) );
#37629 = ADVANCED_FACE ( 'NONE', ( #900 ), #15134, .T. ) ;
#37630 = DIRECTION ( 'NONE',  ( 0.000000000000000000, 0.000000000000000000, 1.000000000000000000 ) ) ;
#37631 = ORIENTED_EDGE ( 'NONE', *, *, #32199, .T. ) ;
#37632 = AXIS2_PLACEMENT_3D ( 'NONE', #24911, #9261, #46953 ) ;
#37633 = VERTEX_POINT ( 'NONE', #15849 ) ;
#37634 = VERTEX_POINT ( 'NONE', #12195 ) ;
#37635 = DIRECTION ( 'NONE',  ( -1.000000000000000000, 0.000000000000000000, 0.000000000000000000 ) ) ;
#37636 = CARTESIAN_POINT ( 'NONE',  ( 0.000000000000000000, -10.30890764327323161, -81.34940948281348483 ) ) ;
#37637 = ORIENTED_EDGE ( 'NONE', *, *, #41725, .F. ) ;
#37638 = EDGE_CURVE ( 'NONE', #19851, #13864, #48407, .T. ) ;
#37639 = EDGE_CURVE ( 'NONE', #28820, #16811, #21798, .T. ) ;
#37640 = AXIS2_PLACEMENT_3D ( 'NONE', #42748, #38589, #46894 ) ;
#37641 = AXIS2_PLACEMENT_3D ( 'NONE', #24344, #31723, #8680 ) ;
#37642 = CYLINDRICAL_SURFACE ( 'NONE', #13230, 77.49899999999999523 ) ;
#37643 = ORIENTED_EDGE ( 'NONE', *, *, #16917, .F. ) ;
#37644 = CIRCLE ( 'NONE', #16551, 31.99999999999998934 ) ;
#37645 = CARTESIAN_POINT ( 'NONE',  ( 10.00000000000000000, 30.41916302227216562, -71.27951684757994144 ) ) ;
#37646 = EDGE_CURVE ( 'NONE', #45561, #20366, #8531, .T. ) ;
#37647 = DIRECTION ( 'NONE',  ( 0.000000000000000000, 0.2079116908177664758, 0.9781476007338042455 ) ) ;
#37648 = CARTESIAN_POINT ( 'NONE',  ( 23.41451323550360186, -132.5004227906269989, 5.500000000000000000 ) ) ;
#37649 = VERTEX_POINT ( 'NONE', #8732 ) ;
#37650 = DIRECTION ( 'NONE',  ( 0.000000000000000000, 0.4539904997395477482, -0.8910065241883673437 ) ) ;
#37651 = ORIENTED_EDGE ( 'NONE', *, *, #965, .T. ) ;
#37652 = VERTEX_POINT ( 'NONE', #38861 ) ;
#37653 = CARTESIAN_POINT ( 'NONE',  ( 11.99999999999999822, -63.97538442413390669, -51.29473840253292138 ) ) ;
#37654 = AXIS2_PLACEMENT_3D ( 'NONE', #25955, #10074, #47512 ) ;
#37655 = DIRECTION ( 'NONE',  ( 0.000000000000000000, 0.000000000000000000, -1.000000000000000000 ) ) ;
#37656 = DIRECTION ( 'NONE',  ( -1.000000000000000000, 0.000000000000000000, 0.000000000000000000 ) ) ;
#37657 = EDGE_LOOP ( 'NONE', ( #48054, #16271, #22297, #35591 ) ) ;
#37658 = ORIENTED_EDGE ( 'NONE', *, *, #45786, .F. ) ;
#37659 = LINE ( 'NONE', #33732, #25871 ) ;
#37660 = CARTESIAN_POINT ( 'NONE',  ( 10.00000000000000000, -37.58145647212453611, -0.6853352020794456489 ) ) ;
#37661 = ORIENTED_EDGE ( 'NONE', *, *, #5724, .F. ) ;
#37662 = VERTEX_POINT ( 'NONE', #43008 ) ;
#37663 = CARTESIAN_POINT ( 'NONE',  ( 15.00000000000000000, 8.688484142253932063, -21.88630264137371029 ) ) ;
#37664 = ORIENTED_EDGE ( 'NONE', *, *, #34742, .F. ) ;
#37665 = DIRECTION ( 'NONE',  ( 1.000000000000000000, 0.000000000000000000, 0.000000000000000000 ) ) ;
#37666 = DIRECTION ( 'NONE',  ( 0.9966891607226785466, 0.08130631524010119293, -0.000000000000000000 ) ) ;
#37667 = DIRECTION ( 'NONE',  ( 0.000000000000000000, 0.000000000000000000, 1.000000000000000000 ) ) ;
#37668 = LINE ( 'NONE', #7324, #1890 ) ;
#37669 = ORIENTED_EDGE ( 'NONE', *, *, #14149, .T. ) ;
#37670 = CARTESIAN_POINT ( 'NONE',  ( 10.00000000000000000, -44.88180994100329713, -63.18004540533077318 ) ) ;
#37671 = CARTESIAN_POINT ( 'NONE',  ( 5.000000000000002665, 8.966570791701863996, -81.50828551894218776 ) ) ;
#37673 = AXIS2_PLACEMENT_3D ( 'NONE', #6975, #21665, #36820 ) ;
#37672 = DIRECTION ( 'NONE',  ( -1.000000000000000000, 0.000000000000000000, 0.000000000000000000 ) ) ;
#37674 = DIRECTION ( 'NONE',  ( 1.000000000000000000, 0.000000000000000000, 0.000000000000000000 ) ) ;
#37675 = CARTESIAN_POINT ( 'NONE',  ( 11.99999999999999822, 0.000000000000000000, 0.000000000000000000 ) ) ;
#37676 = AXIS2_PLACEMENT_3D ( 'NONE', #7614, #10, #41393 ) ;
#37677 = EDGE_CURVE ( 'NONE', #36949, #3853, #5555, .T. ) ;
#37678 = CARTESIAN_POINT ( 'NONE',  ( -3.000000000000000000, 14.60985201121704513, 18.46759930825707841 ) ) ;
#37679 = CARTESIAN_POINT ( 'NONE',  ( 11.99999999999999822, -68.67312586195022561, 35.91791733033451806 ) ) ;
#37680 =( NAMED_UNIT ( * ) SI_UNIT ( $, .STERADIAN. ) SOLID_ANGLE_UNIT ( ) );
#37681 = CARTESIAN_POINT ( 'NONE',  ( -25.50183398199384044, -112.6408924756582053, -2.500000000000000000 ) ) ;
#37682 = EDGE_CURVE ( 'NONE', #33388, #15777, #3823, .T. ) ;
#37683 = AXIS2_PLACEMENT_3D ( 'NONE', #8953, #15820, #46165 ) ;
#37684 = VERTEX_POINT ( 'NONE', #35406 ) ;
#37685 = EDGE_CURVE ( 'NONE', #15671, #31890, #31041, .T. ) ;
#37686 = LINE ( 'NONE', #7341, #22921 ) ;
#37687 = VECTOR ( 'NONE', #38141, 1000.000000000000000 ) ;
#37688 = CARTESIAN_POINT ( 'NONE',  ( 10.00000000000000000, 26.02418014898407961, -70.52718814184231633 ) ) ;
#37689 = CYLINDRICAL_SURFACE ( 'NONE', #15166, 82.00000000000000000 ) ;
#37690 = ORIENTED_EDGE ( 'NONE', *, *, #21130, .F. ) ;
#37691 = ADVANCED_FACE ( 'NONE', ( #31523 ), #5325, .T. ) ;
#37692 = ORIENTED_EDGE ( 'NONE', *, *, #24259, .T. ) ;
#37693 = EDGE_CURVE ( 'NONE', #46360, #2363, #16333, .T. ) ;
#37694 = CARTESIAN_POINT ( 'NONE',  ( -10.00000000000000000, 0.000000000000000000, 0.000000000000000000 ) ) ;
#37695 = ORIENTED_EDGE ( 'NONE', *, *, #41138, .T. ) ;
#37696 = ORIENTED_EDGE ( 'NONE', *, *, #9839, .F. ) ;
#37697 = VERTEX_POINT ( 'NONE', #19996 ) ;
#37698 = AXIS2_PLACEMENT_3D ( 'NONE', #23347, #38282, #1070 ) ;
#37699 = EDGE_CURVE ( 'NONE', #13885, #34506, #12914, .T. ) ;
#37700 = CIRCLE ( 'NONE', #46309, 82.00000000000000000 ) ;
#37701 = FACE_OUTER_BOUND ( 'NONE', #30492, .T. ) ;
#37702 = VERTEX_POINT ( 'NONE', #39090 ) ;
#37703 = ORIENTED_EDGE ( 'NONE', *, *, #20210, .F. ) ;
#37704 = DIRECTION ( 'NONE',  ( -1.000000000000000000, -0.000000000000000000, 0.000000000000000000 ) ) ;
#37705 = AXIS2_PLACEMENT_3D ( 'NONE', #19102, #11771, #37226 ) ;
#37706 = ORIENTED_EDGE ( 'NONE', *, *, #8129, .T. ) ;
#37707 = FACE_OUTER_BOUND ( 'NONE', #26736, .T. ) ;
#37708 = DIRECTION ( 'NONE',  ( 0.000000000000000000, -0.5877852522924624790, -0.8090169943749553338 ) ) ;
#37709 = ORIENTED_EDGE ( 'NONE', *, *, #19387, .T. ) ;
#37710 = VECTOR ( 'NONE', #18588, 1000.000000000000000 ) ;
#37711 = VERTEX_POINT ( 'NONE', #45959 ) ;
#37712 = CARTESIAN_POINT ( 'NONE',  ( 0.000000000000000000, 37.22597642581158084, -5.202137450156524068 ) ) ;
#37713 = ORIENTED_EDGE ( 'NONE', *, *, #3637, .F. ) ;
#37714 = EDGE_CURVE ( 'NONE', #45171, #4936, #27853, .T. ) ;
#37715 = CARTESIAN_POINT ( 'NONE',  ( 4.999999999999999112, -3.925862922256468046, 41.81611651403860463 ) ) ;
#37716 = DIRECTION ( 'NONE',  ( 0.6575728627325955200, -0.7533909544171996098, -1.230411769795008318E-16 ) ) ;
#37717 = EDGE_LOOP ( 'NONE', ( #28101, #20837, #23142, #4772 ) ) ;
#37718 = VECTOR ( 'NONE', #39291, 1000.000000000000000 ) ;
#37719 = CARTESIAN_POINT ( 'NONE',  ( 0.000000000000000000, -59.75363087400113926, 56.15606465354937882 ) ) ;
#37720 = VERTEX_POINT ( 'NONE', #28075 ) ;
#37721 = ORIENTED_EDGE ( 'NONE', *, *, #41303, .F. ) ;
#37722 = DIRECTION ( 'NONE',  ( 0.000000000000000000, 0.5877852522924708056, -0.8090169943749491166 ) ) ;
#37723 = DIRECTION ( 'NONE',  ( 0.000000000000000000, -0.8660254037844363761, -0.5000000000000039968 ) ) ;
#37724 = ORIENTED_EDGE ( 'NONE', *, *, #35828, .T. ) ;
#37725 = AXIS2_PLACEMENT_3D ( 'NONE', #39077, #17264, #13137 ) ;
#37726 = CARTESIAN_POINT ( 'NONE',  ( 11.99999999999999822, 0.000000000000000000, 0.000000000000000000 ) ) ;
#37727 = DIRECTION ( 'NONE',  ( 0.000000000000000000, 0.000000000000000000, 1.000000000000000000 ) ) ;
#37728 = CARTESIAN_POINT ( 'NONE',  ( 11.99999999999999822, 31.47745569255237896, -68.26794271651228030 ) ) ;
#37729 = CARTESIAN_POINT ( 'NONE',  ( 4.999999999999999112, 9.188173127307898369, -40.98264845739739570 ) ) ;
#37730 = CARTESIAN_POINT ( 'NONE',  ( -8.826826895187510402, -94.96827758698185562, 5.500000000000000000 ) ) ;
#37731 = LINE ( 'NONE', #3475, #11433 ) ;
#37732 = VERTEX_POINT ( 'NONE', #46438 ) ;
#37733 = CARTESIAN_POINT ( 'NONE',  ( -3.000000000000000000, 0.000000000000000000, 0.000000000000000000 ) ) ;
#37734 = DIRECTION ( 'NONE',  ( -1.000000000000000000, -0.000000000000000000, -0.000000000000000000 ) ) ;
#37735 = DIRECTION ( 'NONE',  ( -1.000000000000000000, 0.000000000000000000, -0.000000000000000000 ) ) ;
#37736 = ADVANCED_FACE ( 'NONE', ( #31276 ), #24159, .T. ) ;
#37737 = CIRCLE ( 'NONE', #38508, 31.99999999999998579 ) ;
#37738 = ADVANCED_FACE ( 'NONE', ( #46190 ), #42526, .T. ) ;
#37739 = LINE ( 'NONE', #11567, #15839 ) ;
#37740 = CARTESIAN_POINT ( 'NONE',  ( -10.00000000000000000, 0.000000000000000000, 0.000000000000000000 ) ) ;
#37742 = CIRCLE ( 'NONE', #21301, 77.49899999999999523 ) ;
#37741 = DIRECTION ( 'NONE',  ( -1.000000000000000000, 0.000000000000000000, 0.000000000000000000 ) ) ;
#37743 = FACE_OUTER_BOUND ( 'NONE', #31708, .T. ) ;
#37744 = ADVANCED_FACE ( 'NONE', ( #2135 ), #17048, .T. ) ;
#37745 = AXIS2_PLACEMENT_3D ( 'NONE', #33753, #45033, #48212 ) ;
#37746 = ORIENTED_EDGE ( 'NONE', *, *, #44001, .F. ) ;
#37747 = AXIS2_PLACEMENT_3D ( 'NONE', #43336, #47239, #39424 ) ;
#37748 = CARTESIAN_POINT ( 'NONE',  ( 4.999999999999999112, -2.663952781846440576, 41.91543099594817789 ) ) ;
#37749 = ORIENTED_EDGE ( 'NONE', *, *, #14859, .F. ) ;
#37750 = EDGE_CURVE ( 'NONE', #47807, #3020, #43243, .T. ) ;
#37751 = DIRECTION ( 'NONE',  ( 1.000000000000000000, 0.000000000000000000, 0.000000000000000000 ) ) ;
#37752 = CIRCLE ( 'NONE', #22087, 16.00000000000000000 ) ;
#37753 = CIRCLE ( 'NONE', #30695, 31.99999999999999289 ) ;
#37754 = DIRECTION ( 'NONE',  ( 0.000000000000000000, -0.2334453638558921240, -0.9723699203976797767 ) ) ;
#37755 = VECTOR ( 'NONE', #19778, 1000.000000000000000 ) ;
#37756 = ORIENTED_EDGE ( 'NONE', *, *, #109, .T. ) ;
#37757 = AXIS2_PLACEMENT_3D ( 'NONE', #27029, #34838, #1059 ) ;
#37758 = VECTOR ( 'NONE', #13553, 1000.000000000000000 ) ;
#37759 = LINE ( 'NONE', #15259, #28505 ) ;
#37760 = EDGE_LOOP ( 'NONE', ( #20394, #6243, #20165, #1529 ) ) ;
#37761 = EDGE_CURVE ( 'NONE', #40687, #13194, #35117, .T. ) ;
#37762 = DIRECTION ( 'NONE',  ( -1.000000000000000000, 0.000000000000000000, 0.000000000000000000 ) ) ;
#37763 = FACE_OUTER_BOUND ( 'NONE', #16320, .T. ) ;
#37765 = VERTEX_POINT ( 'NONE', #42277 ) ;
#37764 = CYLINDRICAL_SURFACE ( 'NONE', #18391, 16.00000000000000000 ) ;
#37766 = ORIENTED_EDGE ( 'NONE', *, *, #12447, .F. ) ;
#37767 = VECTOR ( 'NONE', #27227, 1000.000000000000000 ) ;
#37768 = EDGE_CURVE ( 'NONE', #28440, #43899, #1642, .T. ) ;
#37769 = DIRECTION ( 'NONE',  ( 0.000000000000000000, 0.000000000000000000, 1.000000000000000000 ) ) ;
#37770 = CARTESIAN_POINT ( 'NONE',  ( 10.00000000000000000, -26.01480285779885904, 70.53064760720306481 ) ) ;
#37771 = CARTESIAN_POINT ( 'NONE',  ( 0.000000000000000000, 21.32104025579158701, -30.84782396557194772 ) ) ;
#37772 = AXIS2_PLACEMENT_3D ( 'NONE', #6563, #47199, #20774 ) ;
#37773 = LINE ( 'NONE', #15278, #13270 ) ;
#37774 = VERTEX_POINT ( 'NONE', #18245 ) ;
#37775 = DIRECTION ( 'NONE',  ( 0.000000000000000000, 0.000000000000000000, 1.000000000000000000 ) ) ;
#37776 = ORIENTED_EDGE ( 'NONE', *, *, #24577, .F. ) ;
#37777 = VERTEX_POINT ( 'NONE', #10683 ) ;
#37778 = VECTOR ( 'NONE', #42484, 1000.000000000000000 ) ;
#37779 = LINE ( 'NONE', #4267, #14536 ) ;
#37780 = VECTOR ( 'NONE', #6073, 1000.000000000000000 ) ;
#37781 = AXIS2_PLACEMENT_3D ( 'NONE', #6811, #36651, #7036 ) ;
#37782 = CARTESIAN_POINT ( 'NONE',  ( 0.000000000000000000, -68.27212725128298132, 31.46837873494953541 ) ) ;
#37783 = CARTESIAN_POINT ( 'NONE',  ( 0.000000000000000000, 34.44570377933598593, 69.42325613327452061 ) ) ;
#37784 = DIRECTION ( 'NONE',  ( 0.000000000000000000, 0.000000000000000000, 1.000000000000000000 ) ) ;
#37785 = VERTEX_POINT ( 'NONE', #47857 ) ;
#37786 = CYLINDRICAL_SURFACE ( 'NONE', #7302, 31.99999999999998579 ) ;
#37787 = VECTOR ( 'NONE', #42026, 1000.000000000000000 ) ;
#37788 = DIRECTION ( 'NONE',  ( 0.000000000000000000, 0.000000000000000000, 1.000000000000000000 ) ) ;
#37789 = CARTESIAN_POINT ( 'NONE',  ( 25.38712131070745315, -112.4010479962415872, 2.500000000000000000 ) ) ;
#37790 = FACE_OUTER_BOUND ( 'NONE', #12552, .T. ) ;
#37791 = LINE ( 'NONE', #40739, #9804 ) ;
#37792 = AXIS2_PLACEMENT_3D ( 'NONE', #19385, #19863, #15974 ) ;
#37793 = CARTESIAN_POINT ( 'NONE',  ( 10.00000000000000000, 0.000000000000000000, 0.000000000000000000 ) ) ;
#37794 = LINE ( 'NONE', #22621, #4469 ) ;
#37795 = CARTESIAN_POINT ( 'NONE',  ( 0.000000000000000000, 0.000000000000000000, -54.99999999999998579 ) ) ;
#37796 = CIRCLE ( 'NONE', #6561, 11.59999999999999787 ) ;
#37797 = EDGE_CURVE ( 'NONE', #6843, #35390, #17767, .T. ) ;
#37798 = AXIS2_PLACEMENT_3D ( 'NONE', #3990, #41205, #41928 ) ;
#37799 = DIRECTION ( 'NONE',  ( -0.000000000000000000, -0.9135454576426058626, -0.4067366430757889395 ) ) ;
#37800 = CARTESIAN_POINT ( 'NONE',  ( 23.41451323550360186, -132.5004227906269989, 5.500000000000000000 ) ) ;
#37801 = ADVANCED_FACE ( 'NONE', ( #21687 ), #14346, .T. ) ;
#37802 = CIRCLE ( 'NONE', #41718, 31.99999999999999645 ) ;
#37803 = DIRECTION ( 'NONE',  ( 0.000000000000000000, 0.000000000000000000, 1.000000000000000000 ) ) ;
#37804 = FACE_OUTER_BOUND ( 'NONE', #4803, .T. ) ;
#37805 = DIRECTION ( 'NONE',  ( -1.000000000000000000, 0.000000000000000000, -0.000000000000000000 ) ) ;
#37806 = DIRECTION ( 'NONE',  ( 0.000000000000000000, 0.000000000000000000, 1.000000000000000000 ) ) ;
#37807 = VERTEX_POINT ( 'NONE', #6765 ) ;
#37808 = ADVANCED_FACE ( 'NONE', ( #18000 ), #25347, .T. ) ;
#37809 = ADVANCED_FACE ( 'NONE', ( #2352 ), #47151, .T. ) ;
#37810 = CARTESIAN_POINT ( 'NONE',  ( 10.00000000000000000, -37.58145647212455032, 0.6853352020789044152 ) ) ;
#37811 = ORIENTED_EDGE ( 'NONE', *, *, #14208, .F. ) ;
#37812 = VECTOR ( 'NONE', #12962, 1000.000000000000000 ) ;
#37813 = EDGE_LOOP ( 'NONE', ( #42697, #24001, #39930, #3794 ) ) ;
#37814 = AXIS2_PLACEMENT_3D ( 'NONE', #21655, #25311, #10150 ) ;
#37815 = VECTOR ( 'NONE', #10204, 1000.000000000000114 ) ;
#37816 = ORIENTED_EDGE ( 'NONE', *, *, #42451, .T. ) ;
#37817 = DIRECTION ( 'NONE',  ( -1.000000000000000000, 0.000000000000000000, 0.000000000000000000 ) ) ;
#37818 = ORIENTED_EDGE ( 'NONE', *, *, #6333, .F. ) ;
#37819 = AXIS2_PLACEMENT_3D ( 'NONE', #2394, #9266, #32270 ) ;
#37820 = CARTESIAN_POINT ( 'NONE',  ( 10.00000000000000000, -70.53064760720297954, -26.01480285779911839 ) ) ;
#37821 = VECTOR ( 'NONE', #7577, 1000.000000000000000 ) ;
#37822 = LINE ( 'NONE', #23136, #18723 ) ;
#37823 = CIRCLE ( 'NONE', #1893, 16.00000000000000355 ) ;
#37824 = CARTESIAN_POINT ( 'NONE',  ( 11.99999999999999822, 0.000000000000000000, 0.000000000000000000 ) ) ;
#37825 = ORIENTED_EDGE ( 'NONE', *, *, #25161, .F. ) ;
#37826 = DIRECTION ( 'NONE',  ( -1.000000000000000000, 3.469446951953614189E-15, 0.000000000000000000 ) ) ;
#37827 = VERTEX_POINT ( 'NONE', #29025 ) ;
#37828 = ORIENTED_EDGE ( 'NONE', *, *, #35086, .T. ) ;
#37829 = VECTOR ( 'NONE', #33123, 1000.000000000000227 ) ;
#37830 = ADVANCED_FACE ( 'NONE', ( #32934 ), #40308, .T. ) ;
#37831 = DIRECTION ( 'NONE',  ( -1.000000000000000000, 0.000000000000000000, 0.000000000000000000 ) ) ;
#37832 = DIRECTION ( 'NONE',  ( -1.000000000000000000, 0.000000000000000000, 0.000000000000000000 ) ) ;
#37833 = CARTESIAN_POINT ( 'NONE',  ( 11.99999999999999822, 77.16300072079698680, -27.74655509720590629 ) ) ;
#37834 = EDGE_LOOP ( 'NONE', ( #16342, #4310, #29627, #4379 ) ) ;
#37835 = ORIENTED_EDGE ( 'NONE', *, *, #22217, .F. ) ;
#37836 = VERTEX_POINT ( 'NONE', #29277 ) ;
#37837 = DIRECTION ( 'NONE',  ( 0.000000000000000000, 0.000000000000000000, 1.000000000000000000 ) ) ;
#37838 = VERTEX_POINT ( 'NONE', #48114 ) ;
#37839 = CARTESIAN_POINT ( 'NONE',  ( 11.99999999999999822, -0.8261519478425843888, -77.49459641780887864 ) ) ;
#37840 = ADVANCED_FACE ( 'NONE', ( #44207 ), #14600, .T. ) ;
#37841 = DIRECTION ( 'NONE',  ( -1.000000000000000000, 0.000000000000000000, -0.000000000000000000 ) ) ;
#37842 = DIRECTION ( 'NONE',  ( -1.000000000000000000, -0.000000000000000000, 0.000000000000000000 ) ) ;
#37843 = DIRECTION ( 'NONE',  ( 0.000000000000000000, 0.07845909572784512398, -0.9969173337331279638 ) ) ;
#37844 = DIRECTION ( 'NONE',  ( -1.000000000000000000, 0.000000000000000000, 0.000000000000000000 ) ) ;
#37845 = DIRECTION ( 'NONE',  ( 0.000000000000000000, -1.000000000000000000, 0.000000000000000000 ) ) ;
#37846 = CARTESIAN_POINT ( 'NONE',  ( 0.000000000000000000, 0.000000000000000000, 0.000000000000000000 ) ) ;
#37847 =( NAMED_UNIT ( * ) SI_UNIT ( $, .STERADIAN. ) SOLID_ANGLE_UNIT ( ) );
#37848 = DIRECTION ( 'NONE',  ( 0.000000000000000000, -0.5224985647159561264, 0.8526401643540878483 ) ) ;
#37849 = ORIENTED_EDGE ( 'NONE', *, *, #9505, .F. ) ;
#37850 = DIRECTION ( 'NONE',  ( -1.000000000000000000, 0.000000000000000000, 0.000000000000000000 ) ) ;
#37851 = ORIENTED_EDGE ( 'NONE', *, *, #45319, .F. ) ;
#37852 = ORIENTED_EDGE ( 'NONE', *, *, #45687, .T. ) ;
#37853 = DIRECTION ( 'NONE',  ( -0.2306669878475622604, -0.9730327541852497042, 0.000000000000000000 ) ) ;
#37854 = AXIS2_PLACEMENT_3D ( 'NONE', #469, #22503, #41353 ) ;
#37855 = CIRCLE ( 'NONE', #1086, 42.00000000000000000 ) ;
#37856 = DIRECTION ( 'NONE',  ( -1.000000000000000000, 0.000000000000000000, 0.000000000000000000 ) ) ;
#37857 = CIRCLE ( 'NONE', #16755, 31.99999999999998579 ) ;
#37858 = CARTESIAN_POINT ( 'NONE',  ( 10.00000000000000000, 14.66109333815564852, -73.73191006444555740 ) ) ;
#37859 = LINE ( 'NONE', #12642, #5750 ) ;
#37860 = ADVANCED_FACE ( 'NONE', ( #13623 ), #10428, .T. ) ;
#37861 = EDGE_CURVE ( 'NONE', #38863, #44846, #17928, .T. ) ;
#37862 = EDGE_CURVE ( 'NONE', #30321, #26404, #33588, .T. ) ;
#37863 = DIRECTION ( 'NONE',  ( -1.000000000000000000, -0.000000000000000000, -0.000000000000000000 ) ) ;
#37864 = CARTESIAN_POINT ( 'NONE',  ( 10.00000000000000000, 59.03961581697399907, 46.53671651293969802 ) ) ;
#37865 = EDGE_LOOP ( 'NONE', ( #1077, #13229, #5250, #39043 ) ) ;
#37866 = CIRCLE ( 'NONE', #1091, 77.49900000000000944 ) ;
#37867 = CIRCLE ( 'NONE', #16760, 77.49900000000002365 ) ;
#37868 = LINE ( 'NONE', #30520, #4459 ) ;
#37869 = DIRECTION ( 'NONE',  ( -1.000000000000000000, 0.000000000000000000, 0.000000000000000000 ) ) ;
#37870 = CIRCLE ( 'NONE', #48055, 82.00000000000000000 ) ;
#37871 = EDGE_CURVE ( 'NONE', #3376, #46202, #38277, .T. ) ;
#37872 = AXIS2_PLACEMENT_3D ( 'NONE', #33241, #44496, #47669 ) ;
#37873 = EDGE_CURVE ( 'NONE', #36027, #41278, #21191, .T. ) ;
#37874 = LINE ( 'NONE', #1634, #18137 ) ;
#37875 = CIRCLE ( 'NONE', #31639, 20.69999999999999929 ) ;
#37876 = ORIENTED_EDGE ( 'NONE', *, *, #5145, .T. ) ;
#37877 = EDGE_LOOP ( 'NONE', ( #6795, #16033, #45288, #9760 ) ) ;
#37878 = VERTEX_POINT ( 'NONE', #35888 ) ;
#37879 = ORIENTED_EDGE ( 'NONE', *, *, #15213, .F. ) ;
#37880 = ORIENTED_EDGE ( 'NONE', *, *, #21006, .T. ) ;
#37881 = DIRECTION ( 'NONE',  ( -1.000000000000000000, 0.000000000000000000, -0.000000000000000000 ) ) ;
#37882 = CARTESIAN_POINT ( 'NONE',  ( 10.00000000000000000, 40.65526001592713357, -71.21200624218752750 ) ) ;
#37883 = ORIENTED_EDGE ( 'NONE', *, *, #44340, .T. ) ;
#37884 = VECTOR ( 'NONE', #41642, 1000.000000000000000 ) ;
#37885 = CARTESIAN_POINT ( 'NONE',  ( 0.000000000000000000, 8.830959090343430518, -74.65491531819107252 ) ) ;
#37886 = AXIS2_PLACEMENT_3D ( 'NONE', #36843, #6992, #25824 ) ;
#37887 = AXIS2_PLACEMENT_3D ( 'NONE', #39986, #10610, #21844 ) ;
#37888 = VERTEX_POINT ( 'NONE', #32233 ) ;
#37889 = ORIENTED_EDGE ( 'NONE', *, *, #28524, .T. ) ;
#37890 = ADVANCED_FACE ( 'NONE', ( #28559 ), #32472, .F. ) ;
#37891 = FACE_OUTER_BOUND ( 'NONE', #3504, .T. ) ;
#37892 = CARTESIAN_POINT ( 'NONE',  ( 10.00000000000000000, 0.000000000000000000, 0.000000000000000000 ) ) ;
#37893 = DIRECTION ( 'NONE',  ( -1.000000000000000000, 0.000000000000000000, 0.000000000000000000 ) ) ;
#37894 = ADVANCED_FACE ( 'NONE', ( #25108 ), #6519, .T. ) ;
#37895 = VERTEX_POINT ( 'NONE', #34371 ) ;
#37896 = VECTOR ( 'NONE', #17509, 1000.000000000000000 ) ;
#37897 = ORIENTED_EDGE ( 'NONE', *, *, #26072, .T. ) ;
#37898 = FACE_OUTER_BOUND ( 'NONE', #31770, .T. ) ;
#37899 = ORIENTED_EDGE ( 'NONE', *, *, #32466, .F. ) ;
#37900 = EDGE_LOOP ( 'NONE', ( #43503, #29344, #34690, #19326 ) ) ;
#37901 = VECTOR ( 'NONE', #32155, 999.9999999999998863 ) ;
#37902 = CARTESIAN_POINT ( 'NONE',  ( 0.000000000000000000, -26.01480285779785362, -70.53064760720343429 ) ) ;
#37903 = EDGE_CURVE ( 'NONE', #12095, #34190, #35929, .T. ) ;
#37904 = AXIS2_PLACEMENT_3D ( 'NONE', #15227, #30156, #10321 ) ;
#37905 = CARTESIAN_POINT ( 'NONE',  ( 10.00000000000000000, -16.45098606841102651, -33.79645857604531045 ) ) ;
#37906 = DIRECTION ( 'NONE',  ( 0.000000000000000000, 0.000000000000000000, -1.000000000000000000 ) ) ;
#37907 = EDGE_CURVE ( 'NONE', #30527, #42392, #42187, .T. ) ;
#37909 = ORIENTED_EDGE ( 'NONE', *, *, #5196, .T. ) ;
#37908 = AXIS2_PLACEMENT_3D ( 'NONE', #24613, #46889, #28272 ) ;
#37910 = ORIENTED_EDGE ( 'NONE', *, *, #21260, .T. ) ;
#37911 = DIRECTION ( 'NONE',  ( -1.000000000000000000, 0.000000000000000000, 0.000000000000000000 ) ) ;
#37912 = LINE ( 'NONE', #928, #32172 ) ;
#37913 = ORIENTED_EDGE ( 'NONE', *, *, #32175, .T. ) ;
#37914 = CARTESIAN_POINT ( 'NONE',  ( 10.00000000000000000, 62.50329211542494789, -41.76937507738723099 ) ) ;
#37915 = VERTEX_POINT ( 'NONE', #26565 ) ;
#37916 = CARTESIAN_POINT ( 'NONE',  ( 0.000000000000000000, 0.000000000000000000, 0.000000000000000000 ) ) ;
#37917 = CARTESIAN_POINT ( 'NONE',  ( 10.00000000000000000, -74.65491531819111515, -8.830959090343204920 ) ) ;
#37918 = CARTESIAN_POINT ( 'NONE',  ( 5.000000000000000000, -35.47612816024539484, 22.48208911017487921 ) ) ;
#37919 = CARTESIAN_POINT ( 'NONE',  ( 11.99999999999999822, 18.89407956138362010, -75.16055320797013906 ) ) ;
#37920 = CARTESIAN_POINT ( 'NONE',  ( 6.000000000000000000, -3.894527615417333610, -81.90746397400393164 ) ) ;
#37921 = LINE ( 'NONE', #19306, #38301 ) ;
#37922 = EDGE_CURVE ( 'NONE', #31513, #42004, #14028, .T. ) ;
#37923 = EDGE_CURVE ( 'NONE', #6602, #3764, #42963, .T. ) ;
#37924 = CARTESIAN_POINT ( 'NONE',  ( 0.000000000000000000, -11.30684508768284680, -76.66974797899850103 ) ) ;
#37925 = VECTOR ( 'NONE', #4620, 1000.000000000000000 ) ;
#37926 = DIRECTION ( 'NONE',  ( 0.000000000000000000, 0.000000000000000000, 1.000000000000000000 ) ) ;
#37927 = DIRECTION ( 'NONE',  ( 0.000000000000000000, 0.000000000000000000, 1.000000000000000000 ) ) ;
#37928 = ORIENTED_EDGE ( 'NONE', *, *, #21664, .T. ) ;
#37929 = CARTESIAN_POINT ( 'NONE',  ( 5.999999999999999112, -79.10210256391353312, -21.60688246758669351 ) ) ;
#37930 = FACE_OUTER_BOUND ( 'NONE', #15574, .T. ) ;
#37931 = DIRECTION ( 'NONE',  ( -0.000000000000000000, -0.000000000000000000, -1.000000000000000000 ) ) ;
#37932 = EDGE_CURVE ( 'NONE', #6665, #32258, #15069, .T. ) ;
#37933 = ORIENTED_EDGE ( 'NONE', *, *, #25439, .T. ) ;
#37934 = CIRCLE ( 'NONE', #11354, 21.00000000000000000 ) ;
#37935 = AXIS2_PLACEMENT_3D ( 'NONE', #47568, #6712, #25772 ) ;
#37936 = UNCERTAINTY_MEASURE_WITH_UNIT (LENGTH_MEASURE( 1.000000000000000082E-05 ), #9344, 'distance_accuracy_value', 'NONE');
#37937 = DIRECTION ( 'NONE',  ( 0.000000000000000000, 0.8660254037844370423, -0.5000000000000029976 ) ) ;
#37938 = CIRCLE ( 'NONE', #37129, 16.00000000000000000 ) ;
#37939 = DIRECTION ( 'NONE',  ( -1.000000000000000000, 0.000000000000000000, 0.000000000000000000 ) ) ;
#37940 = CYLINDRICAL_SURFACE ( 'NONE', #35487, 77.49899999999999523 ) ;
#37941 = AXIS2_PLACEMENT_3D ( 'NONE', #17237, #39781, #13346 ) ;
#37942 = ORIENTED_EDGE ( 'NONE', *, *, #40914, .T. ) ;
#37943 = AXIS2_PLACEMENT_3D ( 'NONE', #23268, #42111, #26951 ) ;
#37944 = CIRCLE ( 'NONE', #44196, 31.99999999999998224 ) ;
#37945 = CARTESIAN_POINT ( 'NONE',  ( 10.00000000000000000, -59.46389618801999433, 49.70050353004867816 ) ) ;
#37946 = ORIENTED_EDGE ( 'NONE', *, *, #10176, .F. ) ;
#37947 = EDGE_LOOP ( 'NONE', ( #28300, #39874, #43231, #16950 ) ) ;
#37948 = VECTOR ( 'NONE', #38665, 1000.000000000000114 ) ;
#37949 = VERTEX_POINT ( 'NONE', #19218 ) ;
#37950 = CIRCLE ( 'NONE', #23108, 31.99999999999998579 ) ;
#37951 = DIRECTION ( 'NONE',  ( -1.000000000000000000, -0.000000000000000000, 0.000000000000000000 ) ) ;
#37952 = EDGE_CURVE ( 'NONE', #26872, #27749, #48351, .T. ) ;
#37953 = VERTEX_POINT ( 'NONE', #26081 ) ;
#37954 = VERTEX_POINT ( 'NONE', #3807 ) ;
#37955 = CARTESIAN_POINT ( 'NONE',  ( 5.000000000000000000, 35.47612816024523852, 22.48208911017513145 ) ) ;
#37956 = ORIENTED_EDGE ( 'NONE', *, *, #29275, .T. ) ;
#37957 = EDGE_CURVE ( 'NONE', #25651, #45129, #37822, .T. ) ;
#37958 = DIRECTION ( 'NONE',  ( -1.000000000000000000, -0.000000000000000000, -0.000000000000000000 ) ) ;
#37959 = FACE_OUTER_BOUND ( 'NONE', #44617, .T. ) ;
#37960 = EDGE_CURVE ( 'NONE', #40162, #46110, #40771, .T. ) ;
#37961 = ORIENTED_EDGE ( 'NONE', *, *, #14657, .F. ) ;
#37962 = DIRECTION ( 'NONE',  ( -1.000000000000000000, 0.000000000000000000, 0.000000000000000000 ) ) ;
#37963 = EDGE_LOOP ( 'NONE', ( #4675, #38625, #25431, #20351 ) ) ;
#37964 = DIRECTION ( 'NONE',  ( -1.000000000000000000, 0.000000000000000000, 0.000000000000000000 ) ) ;
#37965 = DIRECTION ( 'NONE',  ( -1.000000000000000000, 0.000000000000000000, -0.000000000000000000 ) ) ;
#37966 = VECTOR ( 'NONE', #25168, 1000.000000000000000 ) ;
#37967 = ORIENTED_EDGE ( 'NONE', *, *, #9390, .F. ) ;
#37968 = DIRECTION ( 'NONE',  ( 0.000000000000000000, -0.07845909572785220165, 0.9969173337331274087 ) ) ;
#37969 = ORIENTED_EDGE ( 'NONE', *, *, #44156, .F. ) ;
#37970 = ORIENTED_EDGE ( 'NONE', *, *, #30528, .T. ) ;
#37971 = CARTESIAN_POINT ( 'NONE',  ( 10.00000000000000000, 0.000000000000000000, 0.000000000000000000 ) ) ;
#37972 = CYLINDRICAL_SURFACE ( 'NONE', #46507, 11.59999999999999964 ) ;
#37973 = ORIENTED_EDGE ( 'NONE', *, *, #11353, .T. ) ;
#37974 = CARTESIAN_POINT ( 'NONE',  ( 10.00000000000000000, 0.000000000000000000, 0.000000000000000000 ) ) ;
#37975 = VECTOR ( 'NONE', #29247, 1000.000000000000000 ) ;
#37976 = ADVANCED_BREP_SHAPE_REPRESENTATION ( '', ( #2442, #11636 ), #10100 ) ;
#37977 = FACE_OUTER_BOUND ( 'NONE', #31173, .T. ) ;
#37978 = FACE_OUTER_BOUND ( 'NONE', #21443, .T. ) ;
#37979 = LINE ( 'NONE', #45814, #34341 ) ;
#37980 = ADVANCED_FACE ( 'NONE', ( #37340 ), #22886, .T. ) ;
#37981 = CARTESIAN_POINT ( 'NONE',  ( 0.000000000000000000, 81.90746397400393164, -3.894527615416979671 ) ) ;
#37982 = EDGE_CURVE ( 'NONE', #5793, #29949, #15548, .T. ) ;
#37983 = DIRECTION ( 'NONE',  ( -1.000000000000000000, 0.000000000000000000, -0.000000000000000000 ) ) ;
#37984 = ORIENTED_EDGE ( 'NONE', *, *, #23582, .F. ) ;
#37985 = CARTESIAN_POINT ( 'NONE',  ( -4.653126046682595884, -146.1313684676804314, 5.500000000000000000 ) ) ;
#37986 = EDGE_CURVE ( 'NONE', #23867, #11188, #30479, .T. ) ;
#37987 = CARTESIAN_POINT ( 'NONE',  ( 0.000000000000000000, -74.65374052328654386, 8.840884882374837161 ) ) ;
#37988 = CARTESIAN_POINT ( 'NONE',  ( 15.00000000000000000, 9.615535125379096826, 24.73947219025905042 ) ) ;
#37989 = ORIENTED_EDGE ( 'NONE', *, *, #31764, .F. ) ;
#37990 = FACE_OUTER_BOUND ( 'NONE', #36746, .T. ) ;
#37991 = LINE ( 'NONE', #45825, #8967 ) ;
#37992 = CYLINDRICAL_SURFACE ( 'NONE', #7643, 77.49899999999999523 ) ;
#37993 = VECTOR ( 'NONE', #30229, 1000.000000000000000 ) ;
#37994 = CARTESIAN_POINT ( 'NONE',  ( -3.000000000000000000, 5.835314593368772229, -22.81335362449846826 ) ) ;
#37995 = ORIENTED_EDGE ( 'NONE', *, *, #1397, .F. ) ;
#37996 = EDGE_LOOP ( 'NONE', ( #5010, #9982, #8447, #38507 ) ) ;
#37997 = EDGE_CURVE ( 'NONE', #21394, #29885, #11881, .T. ) ;
#37998 = EDGE_LOOP ( 'NONE', ( #34597, #3615, #26955, #5171 ) ) ;
#37999 = CIRCLE ( 'NONE', #48111, 82.00000000000000000 ) ;
#38000 = DIRECTION ( 'NONE',  ( 0.000000000000000000, 0.000000000000000000, 1.000000000000000000 ) ) ;
#38001 = EDGE_LOOP ( 'NONE', ( #12006, #28641, #33902, #47453 ) ) ;
#38002 = LINE ( 'NONE', #10848, #3345 ) ;
#38003 = CONTEXT_DEPENDENT_SHAPE_REPRESENTATION ( #46682, #14411 ) ;
#38004 = ORIENTED_EDGE ( 'NONE', *, *, #34778, .F. ) ;
#38005 = CARTESIAN_POINT ( 'NONE',  ( 10.00000000000000000, 55.38113227695858143, -54.21277698773617715 ) ) ;
#38006 = ORIENTED_EDGE ( 'NONE', *, *, #22021, .F. ) ;
#38007 = VECTOR ( 'NONE', #21461, 1000.000000000000000 ) ;
#38008 = ORIENTED_EDGE ( 'NONE', *, *, #46384, .F. ) ;
#38009 = DIRECTION ( 'NONE',  ( 0.000000000000000000, 0.000000000000000000, -1.000000000000000000 ) ) ;
#38010 = AXIS2_PLACEMENT_3D ( 'NONE', #41965, #8644, #1322 ) ;
#38011 = ORIENTED_EDGE ( 'NONE', *, *, #46643, .F. ) ;
#38012 = CARTESIAN_POINT ( 'NONE',  ( -3.000000000000002665, 0.000000000000000000, 20.64000000000000057 ) ) ;
#38013 = CYLINDRICAL_SURFACE ( 'NONE', #22686, 77.49899999999999523 ) ;
#38015 = ORIENTED_EDGE ( 'NONE', *, *, #37181, .T. ) ;
#38014 = DIRECTION ( 'NONE',  ( -1.000000000000000000, 0.000000000000000000, 0.000000000000000000 ) ) ;
#38016 = ORIENTED_EDGE ( 'NONE', *, *, #11743, .T. ) ;
#38017 = EDGE_CURVE ( 'NONE', #8792, #34171, #849, .T. ) ;
#38018 = VECTOR ( 'NONE', #29179, 1000.000000000000000 ) ;
#38019 = CIRCLE ( 'NONE', #1302, 16.00000000000000000 ) ;
#38020 = ADVANCED_FACE ( 'NONE', ( #29751 ), #45648, .T. ) ;
#38021 = EDGE_CURVE ( 'NONE', #16137, #14267, #1524, .T. ) ;
#38022 = CARTESIAN_POINT ( 'NONE',  ( 0.000000000000000000, 0.000000000000000000, 0.000000000000000000 ) ) ;
#38023 = DIRECTION ( 'NONE',  ( 0.000000000000000000, 0.000000000000000000, -1.000000000000000000 ) ) ;
#38024 = FACE_OUTER_BOUND ( 'NONE', #13678, .T. ) ;
#38025 = AXIS2_PLACEMENT_3D ( 'NONE', #29114, #18593, #47253 ) ;
#38026 = EDGE_CURVE ( 'NONE', #46446, #5128, #33657, .T. ) ;
#38027 = DIRECTION ( 'NONE',  ( -1.000000000000000000, 0.000000000000000000, -0.000000000000000000 ) ) ;
#38028 = VERTEX_POINT ( 'NONE', #41265 ) ;
#38029 = ADVANCED_FACE ( 'NONE', ( #7718 ), #22644, .T. ) ;
#38030 = DIRECTION ( 'NONE',  ( 0.000000000000000000, -0.6691306063588654540, -0.7431448254773878048 ) ) ;
#38031 = ORIENTED_EDGE ( 'NONE', *, *, #26696, .T. ) ;
#38032 = EDGE_LOOP ( 'NONE', ( #13085, #29573, #31145, #14597 ) ) ;
#38033 = EDGE_CURVE ( 'NONE', #45751, #31219, #33897, .T. ) ;
#38034 = DIRECTION ( 'NONE',  ( 1.000000000000000000, 0.000000000000000000, 0.000000000000000000 ) ) ;
#38035 = LINE ( 'NONE', #34331, #26184 ) ;
#38036 = PLANE ( 'NONE',  #18771 ) ;
#38037 = DIRECTION ( 'NONE',  ( 0.000000000000000000, 0.000000000000000000, -1.000000000000000000 ) ) ;
#38038 = EDGE_LOOP ( 'NONE', ( #31324, #4771, #32930, #1375 ) ) ;
#38039 = DIRECTION ( 'NONE',  ( -1.000000000000000000, -0.000000000000000000, -0.000000000000000000 ) ) ;
#38040 = CARTESIAN_POINT ( 'NONE',  ( 11.99999999999999822, 71.27951684758026829, 30.41916302227139113 ) ) ;
#38041 = DIRECTION ( 'NONE',  ( 0.000000000000000000, 0.000000000000000000, 1.000000000000000000 ) ) ;
#38042 = CARTESIAN_POINT ( 'NONE',  ( 11.99999999999999822, 0.000000000000000000, 0.000000000000000000 ) ) ;
#38043 = CARTESIAN_POINT ( 'NONE',  ( 0.000000000000000000, 0.000000000000000000, 40.80000000000001847 ) ) ;
#38044 = AXIS2_PLACEMENT_3D ( 'NONE', #26820, #23148, #38087 ) ;
#38045 = DIRECTION ( 'NONE',  ( -1.000000000000000000, 0.000000000000000000, 0.000000000000000000 ) ) ;
#38046 = EDGE_CURVE ( 'NONE', #5367, #36144, #38807, .T. ) ;
#38047 = DIRECTION ( 'NONE',  ( 0.000000000000000000, 0.000000000000000000, -1.000000000000000000 ) ) ;
#38048 = DIRECTION ( 'NONE',  ( -1.000000000000000000, -0.000000000000000000, -0.000000000000000000 ) ) ;
#38049 = AXIS2_PLACEMENT_3D ( 'NONE', #46537, #39432, #36223 ) ;
#38050 = DIRECTION ( 'NONE',  ( 0.000000000000000000, 0.000000000000000000, 1.000000000000000000 ) ) ;
#38051 = CARTESIAN_POINT ( 'NONE',  ( 10.00000000000000000, -22.64427369931191336, 30.00120703465197280 ) ) ;
#38052 = CARTESIAN_POINT ( 'NONE',  ( 10.00000000000000000, -34.44570377933549565, -69.42325613327476219 ) ) ;
#38053 = EDGE_CURVE ( 'NONE', #22253, #5635, #12533, .T. ) ;
#38054 = DIRECTION ( 'NONE',  ( 0.3311129884571304971, 0.9435911131814395114, -0.000000000000000000 ) ) ;
#38055 = CARTESIAN_POINT ( 'NONE',  ( 10.00000000000000000, 12.42422080174639021, 35.38097989696516521 ) ) ;
#38056 = VECTOR ( 'NONE', #46722, 1000.000000000000000 ) ;
#38057 = CARTESIAN_POINT ( 'NONE',  ( 0.000000000000000000, 0.000000000000000000, 0.000000000000000000 ) ) ;
#38058 = EDGE_LOOP ( 'NONE', ( #37567, #15357, #27130, #32737 ) ) ;
#38059 = CIRCLE ( 'NONE', #18520, 82.00000000000000000 ) ;
#38060 = CARTESIAN_POINT ( 'NONE',  ( 5.000000000000000000, -35.47612816024506088, -22.48208911017539435 ) ) ;
#38061 = ORIENTED_EDGE ( 'NONE', *, *, #9291, .F. ) ;
#38062 = VECTOR ( 'NONE', #34912, 1000.000000000000000 ) ;
#38063 = EDGE_CURVE ( 'NONE', #3614, #46270, #27380, .T. ) ;
#38064 = ORIENTED_EDGE ( 'NONE', *, *, #11352, .F. ) ;
#38065 = EDGE_LOOP ( 'NONE', ( #8727, #4602, #14656, #2888 ) ) ;
#38067 = VERTEX_POINT ( 'NONE', #39267 ) ;
#38066 = ADVANCED_BREP_SHAPE_REPRESENTATION ( '', ( #19912, #11636 ), #38234 ) ;
#38068 = CARTESIAN_POINT ( 'NONE',  ( 10.00000000000000000, -72.35160999960831418, 20.41045688087797672 ) ) ;
#38069 = ORIENTED_EDGE ( 'NONE', *, *, #21987, .T. ) ;
#38070 = AXIS2_PLACEMENT_3D ( 'NONE', #45148, #30456, #15765 ) ;
#38071 = EDGE_CURVE ( 'NONE', #13186, #9766, #42712, .T. ) ;
#38072 = CIRCLE ( 'NONE', #6827, 82.00000000000000000 ) ;
#38073 = DIRECTION ( 'NONE',  ( -1.000000000000000000, -0.000000000000000000, 0.000000000000000000 ) ) ;
#38074 = ADVANCED_FACE ( 'NONE', ( #39031 ), #12607, .T. ) ;
#38075 = DIRECTION ( 'NONE',  ( 1.000000000000000000, 6.951859121168206841E-17, -0.000000000000000000 ) ) ;
#38076 = CARTESIAN_POINT ( 'NONE',  ( 0.000000000000000000, -18.13022148937263012, 15.02647892043544608 ) ) ;
#38077 = ORIENTED_EDGE ( 'NONE', *, *, #29393, .T. ) ;
#38078 = AXIS2_PLACEMENT_3D ( 'NONE', #704, #34718, #41359 ) ;
#38079 = CARTESIAN_POINT ( 'NONE',  ( 15.00000000000000000, -25.60904388321925040, -6.976881207771165272 ) ) ;
#38080 = EDGE_LOOP ( 'NONE', ( #39226, #29861, #20581, #13366 ) ) ;
#38081 = EDGE_CURVE ( 'NONE', #12813, #1582, #27534, .T. ) ;
#38082 = CARTESIAN_POINT ( 'NONE',  ( 10.00000000000000000, -76.41127070299262414, -12.93880638057396304 ) ) ;
#38083 = DIRECTION ( 'NONE',  ( 0.000000000000000000, 0.5224985647159500202, -0.8526401643540915121 ) ) ;
#38084 = ORIENTED_EDGE ( 'NONE', *, *, #2827, .T. ) ;
#38085 = CIRCLE ( 'NONE', #21661, 82.00000000000000000 ) ;
#38086 = ORIENTED_EDGE ( 'NONE', *, *, #3179, .F. ) ;
#38087 = DIRECTION ( 'NONE',  ( 0.000000000000000000, 0.000000000000000000, -1.000000000000000000 ) ) ;
#38088 = ORIENTED_EDGE ( 'NONE', *, *, #17701, .F. ) ;
#38089 = ADVANCED_FACE ( 'NONE', ( #42460 ), #16041, .F. ) ;
#38090 = DIRECTION ( 'NONE',  ( -1.000000000000000000, 0.000000000000000000, 0.000000000000000000 ) ) ;
#38091 = CARTESIAN_POINT ( 'NONE',  ( -7.670864526094549163, -97.73662565058241114, 5.500000000000000000 ) ) ;
#38092 = DIRECTION ( 'NONE',  ( 0.000000000000000000, 0.000000000000000000, 1.000000000000000000 ) ) ;
#38093 = CARTESIAN_POINT ( 'NONE',  ( -3.961125083139900749, -143.2122702051246677, 5.500000000000000000 ) ) ;
#38094 = DIRECTION ( 'NONE',  ( 0.000000000000000000, 8.881784197001252323E-16, 1.000000000000000000 ) ) ;
#38095 = CARTESIAN_POINT ( 'NONE',  ( 5.000000000000000000, 81.96053171279902472, 2.543863470248670211 ) ) ;
#38096 = FACE_OUTER_BOUND ( 'NONE', #39511, .T. ) ;
#38097 = CARTESIAN_POINT ( 'NONE',  ( -26.53422223201112828, -120.6595836127786043, -5.500000000000000000 ) ) ;
#38098 = DIRECTION ( 'NONE',  ( 0.000000000000000000, 0.6691306063588676745, -0.7431448254773856954 ) ) ;
#38099 = ORIENTED_EDGE ( 'NONE', *, *, #1873, .F. ) ;
#38100 = VECTOR ( 'NONE', #47602, 1000.000000000000000 ) ;
#38101 = DIRECTION ( 'NONE',  ( -1.000000000000000000, -0.000000000000000000, 0.000000000000000000 ) ) ;
#38102 = PLANE ( 'NONE',  #33247 ) ;
#38103 = ORIENTED_EDGE ( 'NONE', *, *, #33797, .T. ) ;
#38104 = VERTEX_POINT ( 'NONE', #28023 ) ;
#38105 = DIRECTION ( 'NONE',  ( -1.000000000000000000, 0.000000000000000000, 0.000000000000000000 ) ) ;
#38106 = LINE ( 'NONE', #23400, #20711 ) ;
#38107 = DIRECTION ( 'NONE',  ( -1.000000000000000000, -0.000000000000000000, 0.000000000000000000 ) ) ;
#38108 = PLANE ( 'NONE',  #44802 ) ;
#38109 = SURFACE_STYLE_USAGE ( .BOTH. , #23176 ) ;
#38110 = DIRECTION ( 'NONE',  ( -0.000000000000000000, -0.000000000000000000, -1.000000000000000000 ) ) ;
#38111 = AXIS2_PLACEMENT_3D ( 'NONE', #37051, #37299, #18683 ) ;
#38112 = VERTEX_POINT ( 'NONE', #42214 ) ;
#38113 = LINE ( 'NONE', #22463, #31023 ) ;
#38114 = DIRECTION ( 'NONE',  ( 0.000000000000000000, -6.938893903907231533E-15, 1.000000000000000000 ) ) ;
#38115 = AXIS2_PLACEMENT_3D ( 'NONE', #25389, #40345, #26122 ) ;
#38116 =( LENGTH_UNIT ( ) NAMED_UNIT ( * ) SI_UNIT ( .MILLI., .METRE. ) );
#38117 = DIRECTION ( 'NONE',  ( -0.000000000000000000, -0.000000000000000000, -1.000000000000000000 ) ) ;
#38118 = ORIENTED_EDGE ( 'NONE', *, *, #27479, .T. ) ;
#38119 = CIRCLE ( 'NONE', #28725, 31.99999999999998934 ) ;
#38120 = ORIENTED_EDGE ( 'NONE', *, *, #29347, .F. ) ;
#38121 = ORIENTED_EDGE ( 'NONE', *, *, #30718, .F. ) ;
#38122 = DIRECTION ( 'NONE',  ( -1.000000000000000000, -0.000000000000000000, -0.000000000000000000 ) ) ;
#38123 = DIRECTION ( 'NONE',  ( -1.000000000000000000, 0.000000000000000000, 0.000000000000000000 ) ) ;
#38124 = ORIENTED_EDGE ( 'NONE', *, *, #35464, .T. ) ;
#38125 = VECTOR ( 'NONE', #14451, 1000.000000000000000 ) ;
#38126 = VERTEX_POINT ( 'NONE', #27061 ) ;
#38127 = EDGE_CURVE ( 'NONE', #25362, #15864, #24220, .T. ) ;
#38128 = DIRECTION ( 'NONE',  ( 0.000000000000000000, 0.000000000000000000, 1.000000000000000000 ) ) ;
#38129 = VERTEX_POINT ( 'NONE', #20667 ) ;
#38130 = ORIENTED_EDGE ( 'NONE', *, *, #35958, .F. ) ;
#38131 = EDGE_CURVE ( 'NONE', #32654, #29523, #776, .T. ) ;
#38132 = LINE ( 'NONE', #4598, #14773 ) ;
#38133 = DIRECTION ( 'NONE',  ( -1.000000000000000000, -0.000000000000000000, 0.000000000000000000 ) ) ;
#38134 = VECTOR ( 'NONE', #39228, 1000.000000000000000 ) ;
#38135 = CARTESIAN_POINT ( 'NONE',  ( 10.00000000000000000, 0.000000000000000000, 0.000000000000000000 ) ) ;
#38136 = ORIENTED_EDGE ( 'NONE', *, *, #36523, .F. ) ;
#38137 = CARTESIAN_POINT ( 'NONE',  ( 10.00000000000000000, 27.05870788708267582, -26.08949754952995903 ) ) ;
#38138 = ORIENTED_EDGE ( 'NONE', *, *, #41012, .T. ) ;
#38139 = ORIENTED_EDGE ( 'NONE', *, *, #6635, .T. ) ;
#38140 = EDGE_CURVE ( 'NONE', #7713, #30905, #5497, .T. ) ;
#38141 = DIRECTION ( 'NONE',  ( -1.000000000000000000, 0.000000000000000000, 0.000000000000000000 ) ) ;
#38142 = CYLINDRICAL_SURFACE ( 'NONE', #31164, 82.00000000000000000 ) ;
#38143 = ORIENTED_EDGE ( 'NONE', *, *, #3297, .F. ) ;
#38144 = AXIS2_PLACEMENT_3D ( 'NONE', #10345, #16316, #46173 ) ;
#38145 = EDGE_CURVE ( 'NONE', #48048, #17812, #1563, .T. ) ;
#38146 = DIRECTION ( 'NONE',  ( 1.000000000000000000, 0.000000000000000000, 0.000000000000000000 ) ) ;
#38147 = DIRECTION ( 'NONE',  ( 0.9038112904824853189, -0.4279312458752977388, 0.000000000000000000 ) ) ;
#38148 = AXIS2_PLACEMENT_3D ( 'NONE', #28566, #29524, #36137 ) ;
#38149 = ORIENTED_EDGE ( 'NONE', *, *, #18419, .T. ) ;
#38150 = ORIENTED_EDGE ( 'NONE', *, *, #21274, .F. ) ;
#38151 = DIRECTION ( 'NONE',  ( 0.000000000000000000, 0.000000000000000000, 1.000000000000000000 ) ) ;
#38152 = LINE ( 'NONE', #26895, #72 ) ;
#38153 = EDGE_LOOP ( 'NONE', ( #47689, #20875, #48415, #11758 ) ) ;
#38154 = DIRECTION ( 'NONE',  ( 0.000000000000000000, -0.7431448254773954654, 0.6691306063588569053 ) ) ;
#38155 = EDGE_LOOP ( 'NONE', ( #40895, #33310 ) ) ;
#38156 = DIRECTION ( 'NONE',  ( 0.000000000000000000, 0.000000000000000000, -1.000000000000000000 ) ) ;
#38157 = DIRECTION ( 'NONE',  ( 0.000000000000000000, 0.000000000000000000, -1.000000000000000000 ) ) ;
#38158 = DIRECTION ( 'NONE',  ( 0.000000000000000000, -0.2079116908177532363, -0.9781476007338070211 ) ) ;
#38159 = LINE ( 'NONE', #42807, #17519 ) ;
#38160 =( GEOMETRIC_REPRESENTATION_CONTEXT ( 3 ) GLOBAL_UNCERTAINTY_ASSIGNED_CONTEXT ( ( #30582 ) ) GLOBAL_UNIT_ASSIGNED_CONTEXT ( ( #38116, #33944, #37387 ) ) REPRESENTATION_CONTEXT ( 'NONE', 'WORKASPACE' ) );
#38161 = DIRECTION ( 'NONE',  ( 0.000000000000000000, 0.3090169943749411230, 0.9510565162951555296 ) ) ;
#38162 = LINE ( 'NONE', #8300, #14054 ) ;
#38163 = LINE ( 'NONE', #26665, #46684 ) ;
#38164 = DIRECTION ( 'NONE',  ( 0.000000000000000000, 0.000000000000000000, 1.000000000000000000 ) ) ;
#38165 = CARTESIAN_POINT ( 'NONE',  ( 10.00000000000000000, 10.96151621346540317, -35.95386929396244113 ) ) ;
#38166 = VERTEX_POINT ( 'NONE', #34871 ) ;
#38167 = CARTESIAN_POINT ( 'NONE',  ( -1.029419772574582836, -121.0910063848724718, -2.500000000000000000 ) ) ;
#38168 = CARTESIAN_POINT ( 'NONE',  ( 0.000000000000000000, -76.41127070299280888, 12.93880638057290788 ) ) ;
#38169 = PRODUCT_CONTEXT ( 'NONE', #25068, 'mechanical' ) ;
#38170 = LINE ( 'NONE', #222, #20965 ) ;
#38171 = ORIENTED_EDGE ( 'NONE', *, *, #36070, .F. ) ;
#38172 = EDGE_LOOP ( 'NONE', ( #11827, #44852, #25365, #8937 ) ) ;
#38173 = EDGE_LOOP ( 'NONE', ( #20877, #16574, #14931, #20754 ) ) ;
#38174 = ADVANCED_FACE ( 'NONE', ( #16515 ), #1588, .T. ) ;
#38175 = CARTESIAN_POINT ( 'NONE',  ( 0.000000000000000000, 41.76106447765489094, 62.50884508063442269 ) ) ;
#38176 = EDGE_LOOP ( 'NONE', ( #42203, #7228, #34033, #8481 ) ) ;
#38177 = EDGE_CURVE ( 'NONE', #15200, #10250, #1831, .T. ) ;
#38178 = VECTOR ( 'NONE', #10446, 1000.000000000000000 ) ;
#38179 = CARTESIAN_POINT ( 'NONE',  ( 10.00000000000000000, -18.89407956138203204, -75.16055320797050854 ) ) ;
#38180 = DIRECTION ( 'NONE',  ( 0.000000000000000000, -0.1564344650402170189, -0.9876883405951399908 ) ) ;
#38181 = VECTOR ( 'NONE', #21865, 1000.000000000000000 ) ;
#38182 = EDGE_CURVE ( 'NONE', #25221, #41422, #25023, .T. ) ;
#38183 = VERTEX_POINT ( 'NONE', #35604 ) ;
#38184 = ORIENTED_EDGE ( 'NONE', *, *, #3002, .T. ) ;
#38185 = DIRECTION ( 'NONE',  ( 0.000000000000000000, 0.9135454576426005335, -0.4067366430758010409 ) ) ;
#38186 = ORIENTED_EDGE ( 'NONE', *, *, #43357, .T. ) ;
#38187 = VERTEX_POINT ( 'NONE', #23370 ) ;
#38188 = AXIS2_PLACEMENT_3D ( 'NONE', #33357, #41430, #36545 ) ;
#38189 = EDGE_CURVE ( 'NONE', #16881, #21229, #32064, .T. ) ;
#38190 = EDGE_CURVE ( 'NONE', #44007, #9506, #6277, .T. ) ;
#38191 = ADVANCED_FACE ( 'NONE', ( #10131 ), #21635, .T. ) ;
#38192 = AXIS2_PLACEMENT_3D ( 'NONE', #36537, #10841, #26257 ) ;
#38193 = DIRECTION ( 'NONE',  ( 0.000000000000000000, 0.000000000000000000, 1.000000000000000000 ) ) ;
#38194 = ORIENTED_EDGE ( 'NONE', *, *, #15094, .T. ) ;
#38195 = CARTESIAN_POINT ( 'NONE',  ( 10.00000000000000000, 36.88895765772642932, -6.736453364083163642 ) ) ;
#38196 = EDGE_LOOP ( 'NONE', ( #11983, #20274, #7831, #23592 ) ) ;
#38197 = LINE ( 'NONE', #37955, #41576 ) ;
#38198 = ORIENTED_EDGE ( 'NONE', *, *, #20784, .F. ) ;
#38199 = LINE ( 'NONE', #12265, #22289 ) ;
#38200 = DIRECTION ( 'NONE',  ( 0.000000000000000000, 0.000000000000000000, 1.000000000000000000 ) ) ;
#38201 = ORIENTED_EDGE ( 'NONE', *, *, #23250, .T. ) ;
#38202 = DIRECTION ( 'NONE',  ( -1.000000000000000000, 0.000000000000000000, 0.000000000000000000 ) ) ;
#38203 = ORIENTED_EDGE ( 'NONE', *, *, #23990, .T. ) ;
#38204 = ADVANCED_FACE ( 'NONE', ( #13563 ), #36320, .T. ) ;
#38206 = ORIENTED_EDGE ( 'NONE', *, *, #20619, .F. ) ;
#38205 = DIRECTION ( 'NONE',  ( -0.000000000000000000, -0.000000000000000000, -1.000000000000000000 ) ) ;
#38207 = FACE_OUTER_BOUND ( 'NONE', #27184, .T. ) ;
#38208 = ORIENTED_EDGE ( 'NONE', *, *, #36997, .F. ) ;
#38209 = DIRECTION ( 'NONE',  ( -0.9997280174009349762, 0.02332147558787674504, 0.000000000000000000 ) ) ;
#38210 = AXIS2_PLACEMENT_3D ( 'NONE', #20531, #31334, #27651 ) ;
#38211 = ORIENTED_EDGE ( 'NONE', *, *, #8671, .F. ) ;
#38212 = CARTESIAN_POINT ( 'NONE',  ( -35.50000000000000711, -120.0000000000000000, -5.500000000000000000 ) ) ;
#38213 = DIRECTION ( 'NONE',  ( 0.000000000000000000, -0.4539904997395542430, 0.8910065241883641241 ) ) ;
#38214 = VERTEX_POINT ( 'NONE', #33125 ) ;
#38215 = AXIS2_PLACEMENT_3D ( 'NONE', #46740, #20048, #8784 ) ;
#38216 = CARTESIAN_POINT ( 'NONE',  ( 5.999999999999999112, 79.10210256391368944, 21.60688246758614994 ) ) ;
#38217 = LINE ( 'NONE', #35016, #4008 ) ;
#38218 = CYLINDRICAL_SURFACE ( 'NONE', #19054, 82.00000000000000000 ) ;
#38219 = AXIS2_PLACEMENT_3D ( 'NONE', #10460, #21948, #6796 ) ;
#38220 = CIRCLE ( 'NONE', #714, 12.50000000000000000 ) ;
#38221 = DIRECTION ( 'NONE',  ( -1.000000000000000000, 0.000000000000000000, -0.000000000000000000 ) ) ;
#38222 = CARTESIAN_POINT ( 'NONE',  ( -26.29030328629083968, -123.6496510949466341, 5.500000000000000000 ) ) ;
#38223 = CARTESIAN_POINT ( 'NONE',  ( 11.99999999999999822, -36.72794159290197769, -65.59268652807249111 ) ) ;
#38224 = DIRECTION ( 'NONE',  ( -1.000000000000000000, 0.000000000000000000, 0.000000000000000000 ) ) ;
#38225 = DIRECTION ( 'NONE',  ( 0.000000000000000000, 0.000000000000000000, -1.000000000000000000 ) ) ;
#38226 = CARTESIAN_POINT ( 'NONE',  ( 0.000000000000000000, -80.28980883073769803, 16.65972982744905551 ) ) ;
#38227 = VERTEX_POINT ( 'NONE', #6001 ) ;
#38228 = CYLINDRICAL_SURFACE ( 'NONE', #43232, 16.00000000000000000 ) ;
#38229 = DIRECTION ( 'NONE',  ( 1.000000000000000000, 0.000000000000000000, 0.000000000000000000 ) ) ;
#38230 = CARTESIAN_POINT ( 'NONE',  ( 11.99999999999999822, 0.000000000000000000, 0.000000000000000000 ) ) ;
#38231 = CARTESIAN_POINT ( 'NONE',  ( 12.50000000000000000, -132.5000000000000000, 2.500000000000000000 ) ) ;
#38232 = CARTESIAN_POINT ( 'NONE',  ( 10.00000000000000000, 15.33399622253600292, -80.55351364060572905 ) ) ;
#38233 = ORIENTED_EDGE ( 'NONE', *, *, #34036, .T. ) ;
#38234 =( GEOMETRIC_REPRESENTATION_CONTEXT ( 3 ) GLOBAL_UNCERTAINTY_ASSIGNED_CONTEXT ( ( #4637 ) ) GLOBAL_UNIT_ASSIGNED_CONTEXT ( ( #47711, #40402, #36704 ) ) REPRESENTATION_CONTEXT ( 'NONE', 'WORKASPACE' ) );
#38235 = EDGE_CURVE ( 'NONE', #15455, #42951, #39532, .T. ) ;
#38236 = FACE_BOUND ( 'NONE', #2242, .T. ) ;
#38237 = VERTEX_POINT ( 'NONE', #17715 ) ;
#38238 = CARTESIAN_POINT ( 'NONE',  ( 10.00000000000000000, -59.03342792756297541, 46.54456581323783126 ) ) ;
#38239 = EDGE_CURVE ( 'NONE', #16956, #24649, #24824, .T. ) ;
#38240 = CONTEXT_DEPENDENT_SHAPE_REPRESENTATION ( #15068, #22240 ) ;
#38241 = LINE ( 'NONE', #1284, #5765 ) ;
#38242 = EDGE_CURVE ( 'NONE', #39757, #46672, #3018, .T. ) ;
#38243 = ORIENTED_EDGE ( 'NONE', *, *, #9317, .T. ) ;
#38244 = VECTOR ( 'NONE', #10003, 1000.000000000000000 ) ;
#38245 = DIRECTION ( 'NONE',  ( 0.000000000000000000, 0.000000000000000000, 1.000000000000000000 ) ) ;
#38246 = AXIS2_PLACEMENT_3D ( 'NONE', #23917, #42272, #38614 ) ;
#38247 = ORIENTED_EDGE ( 'NONE', *, *, #21857, .T. ) ;
#38248 = EDGE_CURVE ( 'NONE', #45189, #26808, #3109, .T. ) ;
#38249 = EDGE_CURVE ( 'NONE', #28893, #21133, #14056, .T. ) ;
#38250 = LINE ( 'NONE', #4484, #39413 ) ;
#38251 = AXIS2_PLACEMENT_3D ( 'NONE', #1307, #27497, #5226 ) ;
#38252 = CARTESIAN_POINT ( 'NONE',  ( 2.047646702416564768, -96.54137380445985173, 5.500000000000000000 ) ) ;
#38254 = ORIENTED_EDGE ( 'NONE', *, *, #8906, .T. ) ;
#38253 = DIRECTION ( 'NONE',  ( -0.9966891607226786576, -0.08130631524009861166, 0.000000000000000000 ) ) ;
#38255 = ORIENTED_EDGE ( 'NONE', *, *, #38026, .T. ) ;
#38256 = CARTESIAN_POINT ( 'NONE',  ( 4.999999999999999112, -41.91543099594816368, -2.663952781846588014 ) ) ;
#38257 = CYLINDRICAL_SURFACE ( 'NONE', #41106, 15.99999999999999645 ) ;
#38258 = CARTESIAN_POINT ( 'NONE',  ( 0.000000000000000000, 46.54456581323805153, 59.03342792756280488 ) ) ;
#38259 = ADVANCED_FACE ( 'NONE', ( #25049 ), #47095, .F. ) ;
#38261 = ORIENTED_EDGE ( 'NONE', *, *, #5630, .F. ) ;
#38260 = FACE_OUTER_BOUND ( 'NONE', #38809, .T. ) ;
#38262 = VERTEX_POINT ( 'NONE', #43184 ) ;
#38263 = FACE_OUTER_BOUND ( 'NONE', #38173, .T. ) ;
#38264 = ORIENTED_EDGE ( 'NONE', *, *, #39876, .T. ) ;
#38265 = ORIENTED_EDGE ( 'NONE', *, *, #38026, .F. ) ;
#38266 = DIRECTION ( 'NONE',  ( -0.000000000000000000, -0.8660254037844427044, 0.4999999999999929501 ) ) ;
#38267 = DIRECTION ( 'NONE',  ( -1.000000000000000000, -0.000000000000000000, -0.000000000000000000 ) ) ;
#38268 = CARTESIAN_POINT ( 'NONE',  ( 4.999999999999999112, -41.91543099594816368, -2.663952781846588014 ) ) ;
#38269 = DIRECTION ( 'NONE',  ( 0.000000000000000000, 0.000000000000000000, -1.000000000000000000 ) ) ;
#38270 = ORIENTED_EDGE ( 'NONE', *, *, #2297, .F. ) ;
#38271 = DIRECTION ( 'NONE',  ( 0.9918136447140101231, -0.1276937514489694114, 0.000000000000000000 ) ) ;
#38272 = PLANE ( 'NONE',  #32309 ) ;
#38273 = DIRECTION ( 'NONE',  ( -1.000000000000000000, 0.000000000000000000, 0.000000000000000000 ) ) ;
#38274 = DIRECTION ( 'NONE',  ( 0.000000000000000000, -0.3090169943749549453, 0.9510565162951511997 ) ) ;
#38276 = CIRCLE ( 'NONE', #7766, 82.00000000000000000 ) ;
#38275 = DIRECTION ( 'NONE',  ( 0.000000000000000000, 0.000000000000000000, 1.000000000000000000 ) ) ;
#38277 = CIRCLE ( 'NONE', #17156, 16.00000000000000000 ) ;
#38278 = CARTESIAN_POINT ( 'NONE',  ( 10.00000000000000000, 0.000000000000000000, 0.000000000000000000 ) ) ;
#38279 = DIRECTION ( 'NONE',  ( -1.000000000000000000, 0.000000000000000000, 0.000000000000000000 ) ) ;
#38280 = DIRECTION ( 'NONE',  ( 0.000000000000000000, -0.9876883405951393247, 0.1564344650402205161 ) ) ;
#38281 = CIRCLE ( 'NONE', #6245, 32.50000000000000000 ) ;
#38282 = DIRECTION ( 'NONE',  ( -1.000000000000000000, -0.000000000000000000, -0.000000000000000000 ) ) ;
#38283 = CARTESIAN_POINT ( 'NONE',  ( -10.00000000000000000, 0.000000000000000000, 0.000000000000000000 ) ) ;
#38284 = ORIENTED_EDGE ( 'NONE', *, *, #8008, .F. ) ;
#38285 = ORIENTED_EDGE ( 'NONE', *, *, #35529, .T. ) ;
#38286 = DIRECTION ( 'NONE',  ( 1.000000000000000000, 0.000000000000000000, -0.000000000000000000 ) ) ;
#38287 = DIRECTION ( 'NONE',  ( -1.000000000000000000, -0.000000000000000000, -0.000000000000000000 ) ) ;
#38288 = CIRCLE ( 'NONE', #17142, 16.00000000000000711 ) ;
#38289 = ORIENTED_EDGE ( 'NONE', *, *, #27871, .T. ) ;
#38290 = VERTEX_POINT ( 'NONE', #25534 ) ;
#38291 = EDGE_CURVE ( 'NONE', #36740, #25081, #21135, .T. ) ;
#38292 = PRODUCT_DEFINITION_SHAPE ( 'NONE', 'NONE',  #48466 ) ;
#38293 = CARTESIAN_POINT ( 'NONE',  ( -3.000000000000000000, 18.84667830672605859, -18.68964196561243796 ) ) ;
#38294 = EDGE_CURVE ( 'NONE', #42217, #38611, #30478, .T. ) ;
#38295 = ORIENTED_EDGE ( 'NONE', *, *, #38888, .F. ) ;
#38296 = EDGE_CURVE ( 'NONE', #32513, #30166, #9373, .T. ) ;
#38297 = VERTEX_POINT ( 'NONE', #40484 ) ;
#38298 = VERTEX_POINT ( 'NONE', #6943 ) ;
#38299 = ORIENTED_EDGE ( 'NONE', *, *, #35768, .T. ) ;
#38300 = ADVANCED_FACE ( 'NONE', ( #32875 ), #9636, .T. ) ;
#38301 = VECTOR ( 'NONE', #30570, 1000.000000000000000 ) ;
#38302 = CYLINDRICAL_SURFACE ( 'NONE', #12883, 31.99999999999999289 ) ;
#38303 = AXIS2_PLACEMENT_3D ( 'NONE', #17463, #28741, #17942 ) ;
#38304 = EDGE_CURVE ( 'NONE', #1706, #9886, #3890, .T. ) ;
#38305 = CARTESIAN_POINT ( 'NONE',  ( 10.00000000000000000, -16.45098606841102651, -33.79645857604531045 ) ) ;
#38306 = CARTESIAN_POINT ( 'NONE',  ( 10.00000000000000000, 10.74501242461333028, -35.92658777277499382 ) ) ;
#38307 = AXIS2_PLACEMENT_3D ( 'NONE', #30365, #41377, #34017 ) ;
#38308 = VERTEX_POINT ( 'NONE', #36787 ) ;
#38309 = LINE ( 'NONE', #19446, #9395 ) ;
#38310 = EDGE_LOOP ( 'NONE', ( #7919, #26657, #33927, #2341 ) ) ;
#38311 = AXIS2_PLACEMENT_3D ( 'NONE', #23795, #20123, #1766 ) ;
#38312 = CARTESIAN_POINT ( 'NONE',  ( 10.00000000000000000, 46.11716303203188261, 67.80270845531904911 ) ) ;
#38313 = CARTESIAN_POINT ( 'NONE',  ( 1.250000000000000444, -16.78109714094927085, 0.000000000000000000 ) ) ;
#38314 = AXIS2_PLACEMENT_3D ( 'NONE', #2552, #24840, #10876 ) ;
#38315 = FACE_OUTER_BOUND ( 'NONE', #37223, .T. ) ;
#38316 = ADVANCED_FACE ( 'NONE', ( #21858 ), #40001, .F. ) ;
#38317 = ORIENTED_EDGE ( 'NONE', *, *, #44532, .T. ) ;
#38318 = ORIENTED_EDGE ( 'NONE', *, *, #25243, .F. ) ;
#38319 = VERTEX_POINT ( 'NONE', #32179 ) ;
#38320 = CIRCLE ( 'NONE', #18737, 31.99999999999998579 ) ;
#38321 = DIRECTION ( 'NONE',  ( -1.000000000000000000, -0.000000000000000000, -0.000000000000000000 ) ) ;
#38322 = ORIENTED_EDGE ( 'NONE', *, *, #15682, .F. ) ;
#38323 = DIRECTION ( 'NONE',  ( -1.000000000000000000, 0.000000000000000000, -0.000000000000000000 ) ) ;
#38324 = LINE ( 'NONE', #42234, #18590 ) ;
#38325 = DIRECTION ( 'NONE',  ( 0.000000000000000000, -0.9781476007338041345, 0.2079116908177664480 ) ) ;
#38326 = DIRECTION ( 'NONE',  ( -1.000000000000000000, 0.000000000000000000, 0.000000000000000000 ) ) ;
#38327 = CARTESIAN_POINT ( 'NONE',  ( 0.000000000000000000, 0.000000000000000000, 0.000000000000000000 ) ) ;
#38328 = CARTESIAN_POINT ( 'NONE',  ( -24.50849501662245800, -109.8101191361138831, -5.500000000000000000 ) ) ;
#38329 = DIRECTION ( 'NONE',  ( -1.000000000000000000, -0.000000000000000000, -0.000000000000000000 ) ) ;
#38330 = LINE ( 'NONE', #27816, #43041 ) ;
#38331 = DIRECTION ( 'NONE',  ( -1.000000000000000000, -0.000000000000000000, -0.000000000000000000 ) ) ;
#38332 = EDGE_CURVE ( 'NONE', #24479, #29380, #41426, .T. ) ;
#38333 = CARTESIAN_POINT ( 'NONE',  ( 10.00000000000000000, 0.8828120875900632436, 37.48860685352291000 ) ) ;
#38334 = DIRECTION ( 'NONE',  ( -1.000000000000000000, -0.000000000000000000, -0.000000000000000000 ) ) ;
#38335 = ORIENTED_EDGE ( 'NONE', *, *, #20683, .F. ) ;
#38336 = ORIENTED_EDGE ( 'NONE', *, *, #38294, .F. ) ;
#38337 = DIRECTION ( 'NONE',  ( -1.000000000000000000, -0.000000000000000000, 0.000000000000000000 ) ) ;
#38338 = FACE_OUTER_BOUND ( 'NONE', #16655, .T. ) ;
#38339 = CYLINDRICAL_SURFACE ( 'NONE', #40819, 31.99999999999999289 ) ;
#38340 = DIRECTION ( 'NONE',  ( -1.000000000000000000, 0.000000000000000000, 0.000000000000000000 ) ) ;
#38341 = CARTESIAN_POINT ( 'NONE',  ( -3.000000000000000000, -20.55727247249748046, 16.78983467731285018 ) ) ;
#38342 = CARTESIAN_POINT ( 'NONE',  ( 10.00000000000000000, -35.38097989696520074, 12.42422080174625520 ) ) ;
#38343 = EDGE_LOOP ( 'NONE', ( #8013, #23329, #42761, #7722 ) ) ;
#38344 = DIRECTION ( 'NONE',  ( 1.000000000000000000, -0.000000000000000000, -0.000000000000000000 ) ) ;
#38345 = CARTESIAN_POINT ( 'NONE',  ( 10.00000000000000000, -10.74501242461308159, 35.92658777277507909 ) ) ;
#38346 = VECTOR ( 'NONE', #15731, 1000.000000000000000 ) ;
#38347 = ORIENTED_EDGE ( 'NONE', *, *, #1158, .F. ) ;
#38348 = ADVANCED_FACE ( 'NONE', ( #18439 ), #33372, .T. ) ;
#38349 = VECTOR ( 'NONE', #39053, 1000.000000000000000 ) ;
#38350 = AXIS2_PLACEMENT_3D ( 'NONE', #10071, #3441, #18376 ) ;
#38351 = EDGE_CURVE ( 'NONE', #33111, #18992, #41211, .T. ) ;
#38352 = VERTEX_POINT ( 'NONE', #26017 ) ;
#38353 = DIRECTION ( 'NONE',  ( -1.000000000000000000, -0.000000000000000000, -0.000000000000000000 ) ) ;
#38354 = EDGE_CURVE ( 'NONE', #32798, #2634, #10859, .T. ) ;
#38355 = CIRCLE ( 'NONE', #8640, 11.59999999999999787 ) ;
#38356 = ORIENTED_EDGE ( 'NONE', *, *, #26139, .T. ) ;
#38357 = CIRCLE ( 'NONE', #5508, 31.99999999999999289 ) ;
#38358 = ORIENTED_EDGE ( 'NONE', *, *, #30580, .F. ) ;
#38359 = CIRCLE ( 'NONE', #31319, 12.85999999999999943 ) ;
#38360 = ADVANCED_FACE ( 'NONE', ( #22361 ), #7664, .F. ) ;
#38361 = ORIENTED_EDGE ( 'NONE', *, *, #14608, .F. ) ;
#38362 = CARTESIAN_POINT ( 'NONE',  ( 12.00000000000000000, -3.948201729842355068, -23.21447184625292692 ) ) ;
#38363 = ORIENTED_EDGE ( 'NONE', *, *, #19320, .F. ) ;
#38364 = EDGE_LOOP ( 'NONE', ( #33606, #30309, #6500, #32486 ) ) ;
#38365 = CARTESIAN_POINT ( 'NONE',  ( 11.99999999999999822, 0.000000000000000000, 0.000000000000000000 ) ) ;
#38366 = DIRECTION ( 'NONE',  ( -1.000000000000000000, 0.000000000000000000, 0.000000000000000000 ) ) ;
#38367 = ORIENTED_EDGE ( 'NONE', *, *, #30368, .T. ) ;
#38368 = EDGE_LOOP ( 'NONE', ( #3529, #47984, #43227, #38504 ) ) ;
#38369 = CARTESIAN_POINT ( 'NONE',  ( 0.000000000000000000, 0.000000000000000000, 0.000000000000000000 ) ) ;
#38371 = ORIENTED_EDGE ( 'NONE', *, *, #32920, .F. ) ;
#38370 = LINE ( 'NONE', #15141, #25854 ) ;
#38372 = CIRCLE ( 'NONE', #29775, 31.99999999999998579 ) ;
#38373 = ADVANCED_FACE ( 'NONE', ( #37763 ), #26514, .T. ) ;
#38374 = CARTESIAN_POINT ( 'NONE',  ( -16.06301359042743115, -102.7814171781257357, 2.500000000000000000 ) ) ;
#38376 = ORIENTED_EDGE ( 'NONE', *, *, #21316, .F. ) ;
#38375 = CIRCLE ( 'NONE', #9439, 31.99999999999998579 ) ;
#38377 = LINE ( 'NONE', #5336, #20810 ) ;
#38378 = EDGE_LOOP ( 'NONE', ( #46249, #33143, #5888, #41640 ) ) ;
#38379 = ORIENTED_EDGE ( 'NONE', *, *, #43262, .F. ) ;
#38380 = DIRECTION ( 'NONE',  ( -1.000000000000000000, 0.000000000000000000, -0.000000000000000000 ) ) ;
#38381 = AXIS2_PLACEMENT_3D ( 'NONE', #40590, #37165, #19283 ) ;
#38382 = DIRECTION ( 'NONE',  ( 0.000000000000000000, 0.3090169943749480619, -0.9510565162951533091 ) ) ;
#38383 = ORIENTED_EDGE ( 'NONE', *, *, #34854, .F. ) ;
#38384 = DIRECTION ( 'NONE',  ( -1.000000000000000000, 0.000000000000000000, 0.000000000000000000 ) ) ;
#38385 = LINE ( 'NONE', #7374, #4941 ) ;
#38386 = DIRECTION ( 'NONE',  ( 0.000000000000000000, 1.000000000000000000, -9.787530781167598712E-16 ) ) ;
#38387 = VERTEX_POINT ( 'NONE', #45339 ) ;
#38388 = AXIS2_PLACEMENT_3D ( 'NONE', #48193, #21758, #11239 ) ;
#38389 = ORIENTED_EDGE ( 'NONE', *, *, #41011, .T. ) ;
#38390 = CIRCLE ( 'NONE', #36798, 82.00000000000000000 ) ;
#38391 = DIRECTION ( 'NONE',  ( -1.000000000000000000, 0.000000000000000000, 0.000000000000000000 ) ) ;
#38392 = DIRECTION ( 'NONE',  ( -1.000000000000000000, -0.000000000000000000, 0.000000000000000000 ) ) ;
#38393 = ORIENTED_EDGE ( 'NONE', *, *, #6737, .F. ) ;
#38394 = AXIS2_PLACEMENT_3D ( 'NONE', #9483, #5586, #38887 ) ;
#38395 = DIRECTION ( 'NONE',  ( 0.000000000000000000, 0.000000000000000000, 1.000000000000000000 ) ) ;
#38396 = VERTEX_POINT ( 'NONE', #48056 ) ;
#38397 = CARTESIAN_POINT ( 'NONE',  ( 5.999999999999999112, -59.75363087400114637, 56.15606465354937171 ) ) ;
#38398 = CARTESIAN_POINT ( 'NONE',  ( 15.00000000000000000, 0.000000000000000000, 0.000000000000000000 ) ) ;
#38399 = LINE ( 'NONE', #8766, #47978 ) ;
#38400 = DIRECTION ( 'NONE',  ( 1.000000000000000000, 0.000000000000000000, 0.000000000000000000 ) ) ;
#38401 = CARTESIAN_POINT ( 'NONE',  ( 11.99999999999999822, 0.000000000000000000, 0.000000000000000000 ) ) ;
#38402 = DIRECTION ( 'NONE',  ( 0.000000000000000000, -0.4539904997395541320, 0.8910065241883640130 ) ) ;
#38403 = DIRECTION ( 'NONE',  ( -0.9730327541852491491, 0.2306669878475648139, 0.000000000000000000 ) ) ;
#38404 = DIRECTION ( 'NONE',  ( -1.000000000000000000, -0.000000000000000000, -0.000000000000000000 ) ) ;
#38405 = EDGE_CURVE ( 'NONE', #32185, #44060, #14775, .T. ) ;
#38406 = LINE ( 'NONE', #38167, #4964 ) ;
#38407 = EDGE_CURVE ( 'NONE', #17279, #7503, #44869, .T. ) ;
#38408 =( NAMED_UNIT ( * ) PLANE_ANGLE_UNIT ( ) SI_UNIT ( $, .RADIAN. ) );
#38409 = ORIENTED_EDGE ( 'NONE', *, *, #5709, .F. ) ;
#38410 = CIRCLE ( 'NONE', #29001, 77.49900000000000944 ) ;
#38411 = CIRCLE ( 'NONE', #27483, 16.00000000000000000 ) ;
#38412 = CARTESIAN_POINT ( 'NONE',  ( 0.000000000000000000, -68.26794271651286294, 31.47745569255117104 ) ) ;
#38413 = EDGE_CURVE ( 'NONE', #46842, #4186, #47657, .T. ) ;
#38414 = AXIS2_PLACEMENT_3D ( 'NONE', #20304, #19569, #26954 ) ;
#38415 = CIRCLE ( 'NONE', #25123, 15.39727592589476579 ) ;
#38416 = EDGE_CURVE ( 'NONE', #45508, #34545, #3507, .T. ) ;
#38417 = CARTESIAN_POINT ( 'NONE',  ( 0.000000000000000000, -21.32104025579091910, -30.84782396557241313 ) ) ;
#38418 = CYLINDRICAL_SURFACE ( 'NONE', #33146, 32.50000000000000000 ) ;
#38419 = ORIENTED_EDGE ( 'NONE', *, *, #22610, .T. ) ;
#38420 = VECTOR ( 'NONE', #43270, 1000.000000000000000 ) ;
#38421 = ORIENTED_EDGE ( 'NONE', *, *, #36125, .F. ) ;
#38422 = DIRECTION ( 'NONE',  ( 0.000000000000000000, 0.5224985647159441360, 0.8526401643540952868 ) ) ;
#38423 = VERTEX_POINT ( 'NONE', #41680 ) ;
#38424 = CIRCLE ( 'NONE', #35312, 42.00000000000000000 ) ;
#38425 = VERTEX_POINT ( 'NONE', #4246 ) ;
#38426 = EDGE_LOOP ( 'NONE', ( #42358, #16787, #16427, #13409 ) ) ;
#38427 = ORIENTED_EDGE ( 'NONE', *, *, #38795, .T. ) ;
#38428 = VERTEX_POINT ( 'NONE', #44625 ) ;
#38429 = ORIENTED_EDGE ( 'NONE', *, *, #19177, .T. ) ;
#38430 = CYLINDRICAL_SURFACE ( 'NONE', #28178, 32.00000000000000000 ) ;
#38431 = ORIENTED_EDGE ( 'NONE', *, *, #5257, .F. ) ;
#38432 = CARTESIAN_POINT ( 'NONE',  ( 10.00000000000000000, 77.19088730480534366, -6.903761155836915187 ) ) ;
#38433 = VERTEX_POINT ( 'NONE', #37519 ) ;
#38434 = CARTESIAN_POINT ( 'NONE',  ( 11.99999999999999822, -18.89407956138204980, -75.16055320797050854 ) ) ;
#38435 = CARTESIAN_POINT ( 'NONE',  ( 0.000000000000000000, -9.188173127307592836, 40.98264845739746676 ) ) ;
#38436 = DIRECTION ( 'NONE',  ( 0.000000000000000000, 0.000000000000000000, 1.000000000000000000 ) ) ;
#38437 = VERTEX_POINT ( 'NONE', #44388 ) ;
#38438 = DIRECTION ( 'NONE',  ( -1.000000000000000000, 0.000000000000000000, 0.000000000000000000 ) ) ;
#38439 = ORIENTED_EDGE ( 'NONE', *, *, #20967, .F. ) ;
#38440 = DIRECTION ( 'NONE',  ( 0.000000000000000000, 0.5877852522924741363, -0.8090169943749465631 ) ) ;
#38441 = EDGE_CURVE ( 'NONE', #21097, #22223, #7898, .T. ) ;
#38442 = CARTESIAN_POINT ( 'NONE',  ( 10.00000000000000000, 0.000000000000000000, 0.000000000000000000 ) ) ;
#38443 = ORIENTED_EDGE ( 'NONE', *, *, #27750, .T. ) ;
#38444 = AXIS2_PLACEMENT_3D ( 'NONE', #24062, #5224, #24287 ) ;
#38445 = DIRECTION ( 'NONE',  ( 0.000000000000000000, 0.000000000000000000, -1.000000000000000000 ) ) ;
#38446 = ORIENTED_EDGE ( 'NONE', *, *, #26378, .T. ) ;
#38447 = ORIENTED_EDGE ( 'NONE', *, *, #14385, .F. ) ;
#38448 = DIRECTION ( 'NONE',  ( 0.000000000000000000, 0.000000000000000000, 1.000000000000000000 ) ) ;
#38449 = CARTESIAN_POINT ( 'NONE',  ( 10.00000000000000000, 0.000000000000000000, 0.000000000000000000 ) ) ;
#38450 = AXIS2_PLACEMENT_3D ( 'NONE', #46813, #24529, #43383 ) ;
#38451 = EDGE_CURVE ( 'NONE', #12245, #6771, #3999, .T. ) ;
#38452 = CARTESIAN_POINT ( 'NONE',  ( -16.06301359042743115, -102.7814171781257357, -5.500000000000000000 ) ) ;
#38453 = CARTESIAN_POINT ( 'NONE',  ( 10.00000000000000000, 0.000000000000000000, 0.000000000000000000 ) ) ;
#38454 = CARTESIAN_POINT ( 'NONE',  ( 0.000000000000000000, 0.000000000000000000, -54.99999999999998579 ) ) ;
#38455 = PRESENTATION_LAYER_ASSIGNMENT (  '', '', ( #26719 ) ) ;
#38456 = EDGE_CURVE ( 'NONE', #29827, #11046, #10977, .T. ) ;
#38457 = LINE ( 'NONE', #15945, #39042 ) ;
#38458 = CIRCLE ( 'NONE', #10311, 31.99999999999999645 ) ;
#38459 = CARTESIAN_POINT ( 'NONE',  ( 12.13205353604972814, -140.1820037904669789, -2.500000000000000000 ) ) ;
#38460 = CARTESIAN_POINT ( 'NONE',  ( 10.00000000000000000, -51.03279382321125723, 55.19960302592048862 ) ) ;
#38461 = CARTESIAN_POINT ( 'NONE',  ( -10.90076147243505211, 0.000000000000000000, 0.000000000000000000 ) ) ;
#38462 = LINE ( 'NONE', #16669, #42037 ) ;
#38463 = DIRECTION ( 'NONE',  ( 1.000000000000000000, -0.000000000000000000, -0.000000000000000000 ) ) ;
#38464 = CIRCLE ( 'NONE', #32967, 30.50000000000000000 ) ;
#38465 = CARTESIAN_POINT ( 'NONE',  ( 10.00000000000000000, 41.81611651403867569, -3.925862922255714871 ) ) ;
#38466 = DIRECTION ( 'NONE',  ( -1.000000000000000000, -0.000000000000000000, -0.000000000000000000 ) ) ;
#38467 = CARTESIAN_POINT ( 'NONE',  ( 0.000000000000000000, -74.18225833017864090, -34.94270380257717790 ) ) ;
#38468 = ADVANCED_FACE ( 'NONE', ( #25769 ), #38013, .T. ) ;
#38469 = CARTESIAN_POINT ( 'NONE',  ( 0.000000000000000000, -12.26510123303284594, 35.53030884539080603 ) ) ;
#38470 = EDGE_CURVE ( 'NONE', #35947, #6714, #30426, .T. ) ;
#38471 = ORIENTED_EDGE ( 'NONE', *, *, #42563, .T. ) ;
#38472 = EDGE_CURVE ( 'NONE', #46674, #32773, #40708, .T. ) ;
#38473 = DIRECTION ( 'NONE',  ( 0.000000000000000000, -0.8910065241883626808, -0.4539904997395569075 ) ) ;
#38474 = ORIENTED_EDGE ( 'NONE', *, *, #4162, .T. ) ;
#38475 = DIRECTION ( 'NONE',  ( 0.000000000000000000, 0.5877852522924685852, 0.8090169943749508930 ) ) ;
#38476 = AXIS2_PLACEMENT_3D ( 'NONE', #17306, #2380, #5115 ) ;
#38477 = ITEM_DEFINED_TRANSFORMATION ( 'NONE', 'NONE', #44410,  #11636 ) ;
#38478 = EDGE_CURVE ( 'NONE', #26342, #19231, #35992, .T. ) ;
#38479 = CARTESIAN_POINT ( 'NONE',  ( 10.00000000000000000, -33.79645857604501913, -16.45098606841161626 ) ) ;
#38480 = EDGE_LOOP ( 'NONE', ( #9628, #1650, #20131, #41529 ) ) ;
#38481 = AXIS2_PLACEMENT_3D ( 'NONE', #17251, #10161, #25565 ) ;
#38482 = CIRCLE ( 'NONE', #3284, 16.00000000000000000 ) ;
#38483 = PLANE ( 'NONE',  #37792 ) ;
#38484 = EDGE_CURVE ( 'NONE', #30556, #6444, #4715, .T. ) ;
#38485 = ORIENTED_EDGE ( 'NONE', *, *, #10987, .T. ) ;
#38486 = CARTESIAN_POINT ( 'NONE',  ( 0.000000000000000000, 59.03961581697399907, 46.53671651293969802 ) ) ;
#38487 = CIRCLE ( 'NONE', #14276, 31.99999999999999645 ) ;
#38488 = CARTESIAN_POINT ( 'NONE',  ( -10.00000000000000000, 0.000000000000000000, 0.000000000000000000 ) ) ;
#38489 = CARTESIAN_POINT ( 'NONE',  ( 10.00000000000000000, 21.40280677340372151, 36.13751322684426981 ) ) ;
#38490 = VERTEX_POINT ( 'NONE', #20126 ) ;
#38492 = ORIENTED_EDGE ( 'NONE', *, *, #22037, .F. ) ;
#38491 = CYLINDRICAL_SURFACE ( 'NONE', #28569, 42.00000000000000000 ) ;
#38493 = AXIS2_PLACEMENT_3D ( 'NONE', #44431, #18486, #10671 ) ;
#38494 = ORIENTED_EDGE ( 'NONE', *, *, #21612, .F. ) ;
#38495 = ORIENTED_EDGE ( 'NONE', *, *, #23331, .T. ) ;
#38496 = DIRECTION ( 'NONE',  ( -0.000000000000000000, -0.000000000000000000, -1.000000000000000000 ) ) ;
#38497 = FACE_OUTER_BOUND ( 'NONE', #47815, .T. ) ;
#38498 = ADVANCED_FACE ( 'NONE', ( #16454 ), #41938, .T. ) ;
#38499 = CARTESIAN_POINT ( 'NONE',  ( 0.000000000000000000, -46.11716303203234446, 67.80270845531873647 ) ) ;
#38500 = CARTESIAN_POINT ( 'NONE',  ( 10.00000000000000000, -37.22597642581153821, -5.202137450156795850 ) ) ;
#38501 = EDGE_CURVE ( 'NONE', #33738, #18614, #35289, .T. ) ;
#38502 = ORIENTED_EDGE ( 'NONE', *, *, #3310, .F. ) ;
#38503 = DIRECTION ( 'NONE',  ( 0.6516173805718078471, -0.7585478161175706058, 0.000000000000000000 ) ) ;
#38504 = ORIENTED_EDGE ( 'NONE', *, *, #10609, .T. ) ;
#38505 = ORIENTED_EDGE ( 'NONE', *, *, #40653, .T. ) ;
#38506 = CARTESIAN_POINT ( 'NONE',  ( -26.29030328629083968, -123.6496510949466341, 5.500000000000000000 ) ) ;
#38507 = ORIENTED_EDGE ( 'NONE', *, *, #8404, .T. ) ;
#38508 = AXIS2_PLACEMENT_3D ( 'NONE', #5401, #46527, #13000 ) ;
#38509 = EDGE_CURVE ( 'NONE', #648, #500, #1770, .T. ) ;
#38510 = DIRECTION ( 'NONE',  ( -1.000000000000000000, 0.000000000000000000, -0.000000000000000000 ) ) ;
#38511 = DIRECTION ( 'NONE',  ( 0.000000000000000000, 0.000000000000000000, 1.000000000000000000 ) ) ;
#38512 = DIRECTION ( 'NONE',  ( -0.000000000000000000, 0.9945218953682731788, 0.1045284632676559550 ) ) ;
#38513 = ORIENTED_EDGE ( 'NONE', *, *, #11694, .F. ) ;
#38514 = CARTESIAN_POINT ( 'NONE',  ( -48.80839716909612491, -10.37454508288793065, 5.500000000000000000 ) ) ;
#38515 = AXIS2_PLACEMENT_3D ( 'NONE', #3358, #7762, #36420 ) ;
#38516 = ADVANCED_FACE ( 'NONE', ( #38748 ), #1030, .T. ) ;
#38517 = CARTESIAN_POINT ( 'NONE',  ( 10.00000000000000000, 62.50329211542435104, 41.76937507738811917 ) ) ;
#38518 = CARTESIAN_POINT ( 'NONE',  ( 11.99999999999999822, -77.32052557432845674, 5.256550761632577284 ) ) ;
#38519 = AXIS2_PLACEMENT_3D ( 'NONE', #47545, #28942, #10343 ) ;
#38520 = CARTESIAN_POINT ( 'NONE',  ( 3.429551818649054340, -146.3199197248623875, 5.500000000000000000 ) ) ;
#38521 = PLANE ( 'NONE',  #45845 ) ;
#38522 = AXIS2_PLACEMENT_3D ( 'NONE', #37971, #8817, #23510 ) ;
#38523 = CARTESIAN_POINT ( 'NONE',  ( 10.00000000000000000, 22.74946021919175720, -29.81001611430984255 ) ) ;
#38524 = CARTESIAN_POINT ( 'NONE',  ( 0.000000000000000000, 26.02418014898310261, 70.52718814184268581 ) ) ;
#38526 = LINE ( 'NONE', #38783, #27158 ) ;
#38525 =( REPRESENTATION_RELATIONSHIP ('NONE','NONE', #5957, #45973 ) REPRESENTATION_RELATIONSHIP_WITH_TRANSFORMATION ( #43365 )SHAPE_REPRESENTATION_RELATIONSHIP( ) );
#38527 = CIRCLE ( 'NONE', #8039, 31.99999999999999289 ) ;
#38528 = VECTOR ( 'NONE', #23945, 1000.000000000000000 ) ;
#38529 = CYLINDRICAL_SURFACE ( 'NONE', #34581, 31.99999999999999289 ) ;
#38530 = FACE_OUTER_BOUND ( 'NONE', #8434, .T. ) ;
#38531 = VECTOR ( 'NONE', #21230, 1000.000000000000000 ) ;
#38532 = ADVANCED_FACE ( 'NONE', ( #46318 ), #5215, .T. ) ;
#38533 = ORIENTED_EDGE ( 'NONE', *, *, #36932, .F. ) ;
#38534 = ADVANCED_FACE ( 'NONE', ( #31159 ), #42656, .T. ) ;
#38535 = CARTESIAN_POINT ( 'NONE',  ( -2.500000000000000000, 16.00000000000000000, 0.000000000000000000 ) ) ;
#38536 = VECTOR ( 'NONE', #24127, 1000.000000000000000 ) ;
#38537 = EDGE_LOOP ( 'NONE', ( #43739, #4447, #10551, #19638 ) ) ;
#38538 = ORIENTED_EDGE ( 'NONE', *, *, #29619, .T. ) ;
#38539 = DIRECTION ( 'NONE',  ( 0.000000000000000000, 0.000000000000000000, 1.000000000000000000 ) ) ;
#38540 = VECTOR ( 'NONE', #29202, 1000.000000000000000 ) ;
#38541 = CARTESIAN_POINT ( 'NONE',  ( -18.24502636017238899, -100.7225776329765665, -2.500000000000000444 ) ) ;
#38542 = ORIENTED_EDGE ( 'NONE', *, *, #28888, .T. ) ;
#38543 = EDGE_CURVE ( 'NONE', #6370, #43886, #46570, .T. ) ;
#38544 = ORIENTED_EDGE ( 'NONE', *, *, #15588, .T. ) ;
#38545 = ORIENTED_EDGE ( 'NONE', *, *, #40237, .T. ) ;
#38546 = EDGE_LOOP ( 'NONE', ( #16988, #33824, #21964, #25181 ) ) ;
#38547 = AXIS2_PLACEMENT_3D ( 'NONE', #7887, #37751, #45327 ) ;
#38548 = VERTEX_POINT ( 'NONE', #9114 ) ;
#38549 = AXIS2_PLACEMENT_3D ( 'NONE', #4222, #19136, #3975 ) ;
#38550 = DIRECTION ( 'NONE',  ( 0.9227826878668540234, 0.3853207896976547087, 0.000000000000000000 ) ) ;
#38551 = DIRECTION ( 'NONE',  ( -1.000000000000000000, -0.000000000000000000, 0.000000000000000000 ) ) ;
#38552 = CIRCLE ( 'NONE', #44793, 42.00000000000000000 ) ;
#38553 = AXIS2_PLACEMENT_3D ( 'NONE', #31904, #28694, #13513 ) ;
#38554 = CARTESIAN_POINT ( 'NONE',  ( -12.50000000000000000, -107.5000000000000000, 40.00000000000000000 ) ) ;
#38555 = VERTEX_POINT ( 'NONE', #5443 ) ;
#38556 = DIRECTION ( 'NONE',  ( -1.000000000000000000, 0.000000000000000000, 0.000000000000000000 ) ) ;
#38557 = AXIS2_PLACEMENT_3D ( 'NONE', #24894, #35906, #25844 ) ;
#38558 = VERTEX_POINT ( 'NONE', #24052 ) ;
#38559 = CIRCLE ( 'NONE', #45609, 31.99999999999999289 ) ;
#38560 = VERTEX_POINT ( 'NONE', #42894 ) ;
#38561 = DIRECTION ( 'NONE',  ( 0.9730327541852497042, -0.2306669878475623159, 0.000000000000000000 ) ) ;
#38562 = CYLINDRICAL_SURFACE ( 'NONE', #27837, 31.99999999999998579 ) ;
#38563 = FACE_OUTER_BOUND ( 'NONE', #9700, .T. ) ;
#38564 = VECTOR ( 'NONE', #14281, 1000.000000000000000 ) ;
#38565 = ORIENTED_EDGE ( 'NONE', *, *, #25801, .T. ) ;
#38566 = ORIENTED_EDGE ( 'NONE', *, *, #29243, .T. ) ;
#38567 = CARTESIAN_POINT ( 'NONE',  ( 11.99999999999999822, 0.000000000000000000, 0.000000000000000000 ) ) ;
#38568 = ORIENTED_EDGE ( 'NONE', *, *, #26185, .T. ) ;
#38569 = DIRECTION ( 'NONE',  ( 0.000000000000000000, 0.000000000000000000, -1.000000000000000000 ) ) ;
#38570 = CIRCLE ( 'NONE', #14347, 16.00000000000000000 ) ;
#38571 = EDGE_CURVE ( 'NONE', #37634, #1618, #31652, .T. ) ;
#38572 = CARTESIAN_POINT ( 'NONE',  ( -3.000000000000000000, 22.07842321921492612, -8.187992925817130896 ) ) ;
#38573 = PLANE ( 'NONE',  #18160 ) ;
#38574 = CARTESIAN_POINT ( 'NONE',  ( 10.00000000000000000, -5.256550761633413060, 77.32052557432841411 ) ) ;
#38575 = FACE_OUTER_BOUND ( 'NONE', #3034, .T. ) ;
#38576 = CARTESIAN_POINT ( 'NONE',  ( -10.00000000000000000, 0.000000000000000000, 0.000000000000000000 ) ) ;
#38577 = EDGE_CURVE ( 'NONE', #25331, #11148, #25048, .T. ) ;
#38578 = CONICAL_SURFACE ( 'NONE', #22141, 17.30399999999999849, 0.2094395102393129815 ) ;
#38579 = DIRECTION ( 'NONE',  ( -1.000000000000000000, -0.000000000000000000, -0.000000000000000000 ) ) ;
#38580 = ORIENTED_EDGE ( 'NONE', *, *, #44924, .T. ) ;
#38581 = DIRECTION ( 'NONE',  ( -0.000000000000000000, -0.000000000000000000, -1.000000000000000000 ) ) ;
#38582 = FACE_OUTER_BOUND ( 'NONE', #35470, .T. ) ;
#38583 = FACE_OUTER_BOUND ( 'NONE', #12411, .T. ) ;
#38584 = CARTESIAN_POINT ( 'NONE',  ( 0.000000000000000000, -62.50329211542407393, -41.76937507738853839 ) ) ;
#38585 = VERTEX_POINT ( 'NONE', #19868 ) ;
#38586 = ORIENTED_EDGE ( 'NONE', *, *, #14475, .F. ) ;
#38587 = CARTESIAN_POINT ( 'NONE',  ( 0.000000000000000000, 77.16300072079698680, -27.74655509720590985 ) ) ;
#38588 = CARTESIAN_POINT ( 'NONE',  ( -3.000000000000000000, -23.29833615347104825, -3.418703333116803744 ) ) ;
#38589 = DIRECTION ( 'NONE',  ( -1.000000000000000000, 0.000000000000000000, 0.000000000000000000 ) ) ;
#38590 = CARTESIAN_POINT ( 'NONE',  ( 0.000000000000000000, 0.000000000000000000, 0.000000000000000000 ) ) ;
#38591 = EDGE_CURVE ( 'NONE', #27090, #24152, #31333, .T. ) ;
#38592 = EDGE_CURVE ( 'NONE', #38028, #13081, #24279, .T. ) ;
#38593 =( NAMED_UNIT ( * ) PLANE_ANGLE_UNIT ( ) SI_UNIT ( $, .RADIAN. ) );
#38594 = CARTESIAN_POINT ( 'NONE',  ( 10.00000000000000000, 50.23322058963347558, 64.81221759200361987 ) ) ;
#38595 = DIRECTION ( 'NONE',  ( 0.000000000000000000, -0.7071067811865389130, -0.7071067811865561215 ) ) ;
#38596 = CARTESIAN_POINT ( 'NONE',  ( 11.99999999999999822, 0.000000000000000000, 0.000000000000000000 ) ) ;
#38597 = EDGE_CURVE ( 'NONE', #22836, #1330, #1297, .T. ) ;
#38598 = ORIENTED_EDGE ( 'NONE', *, *, #3804, .T. ) ;
#38599 = AXIS2_PLACEMENT_3D ( 'NONE', #30497, #4556, #37843 ) ;
#38600 = VERTEX_POINT ( 'NONE', #23316 ) ;
#38601 = DIRECTION ( 'NONE',  ( 0.000000000000000000, 0.000000000000000000, 1.000000000000000000 ) ) ;
#38602 = LINE ( 'NONE', #1144, #29895 ) ;
#38603 = ORIENTED_EDGE ( 'NONE', *, *, #16514, .T. ) ;
#38604 = ORIENTED_EDGE ( 'NONE', *, *, #48145, .F. ) ;
#38605 = EDGE_CURVE ( 'NONE', #10383, #337, #27237, .T. ) ;
#38606 = ORIENTED_EDGE ( 'NONE', *, *, #10431, .F. ) ;
#38607 = CIRCLE ( 'NONE', #18241, 31.99999999999998579 ) ;
#38608 = CIRCLE ( 'NONE', #9652, 31.99999999999998934 ) ;
#38609 = EDGE_LOOP ( 'NONE', ( #37166, #42201, #40233, #18196 ) ) ;
#38610 = AXIS2_PLACEMENT_3D ( 'NONE', #19583, #45545, #4918 ) ;
#38611 = VERTEX_POINT ( 'NONE', #38489 ) ;
#38612 = AXIS2_PLACEMENT_3D ( 'NONE', #954, #44788, #45506 ) ;
#38613 = ORIENTED_EDGE ( 'NONE', *, *, #15009, .T. ) ;
#38614 = DIRECTION ( 'NONE',  ( 0.000000000000000000, 0.5877852522924684742, 0.8090169943749506709 ) ) ;
#38615 = VERTEX_POINT ( 'NONE', #4955 ) ;
#38616 = VECTOR ( 'NONE', #37283, 1000.000000000000000 ) ;
#38617 = ORIENTED_EDGE ( 'NONE', *, *, #17913, .T. ) ;
#38618 = DIRECTION ( 'NONE',  ( -1.000000000000000000, 0.000000000000000000, 0.000000000000000000 ) ) ;
#38619 = CARTESIAN_POINT ( 'NONE',  ( -11.69999999999999929, 0.000000000000000000, -20.99999999999999645 ) ) ;
#38620 = ORIENTED_EDGE ( 'NONE', *, *, #629, .F. ) ;
#38621 = ORIENTED_EDGE ( 'NONE', *, *, #42354, .F. ) ;
#38622 = AXIS2_PLACEMENT_3D ( 'NONE', #47660, #44485, #11201 ) ;
#38623 = DIRECTION ( 'NONE',  ( -1.000000000000000000, -0.000000000000000000, 0.000000000000000000 ) ) ;
#38625 = ORIENTED_EDGE ( 'NONE', *, *, #13677, .F. ) ;
#38624 = LINE ( 'NONE', #42533, #30541 ) ;
#38627 = DIRECTION ( 'NONE',  ( 1.000000000000000000, 0.000000000000000000, 0.000000000000000000 ) ) ;
#38626 = AXIS2_PLACEMENT_3D ( 'NONE', #31427, #38998, #28212 ) ;
#38628 = VERTEX_POINT ( 'NONE', #34811 ) ;
#38629 = CARTESIAN_POINT ( 'NONE',  ( 10.00000000000000000, -75.11764819372149304, 2.946379043146075905 ) ) ;
#38630 = VERTEX_POINT ( 'NONE', #42405 ) ;
#38631 = ORIENTED_EDGE ( 'NONE', *, *, #12249, .T. ) ;
#38632 = EDGE_CURVE ( 'NONE', #36250, #17899, #8862, .T. ) ;
#38633 = CARTESIAN_POINT ( 'NONE',  ( 0.000000000000000000, 73.72996012237440766, 14.67089635893739619 ) ) ;
#38634 = AXIS2_PLACEMENT_3D ( 'NONE', #18808, #41834, #41115 ) ;
#38635 = AXIS2_PLACEMENT_3D ( 'NONE', #24608, #5518, #39551 ) ;
#38636 = DIRECTION ( 'NONE',  ( -1.000000000000000000, 0.000000000000000000, 0.000000000000000000 ) ) ;
#38637 = VECTOR ( 'NONE', #5537, 1000.000000000000000 ) ;
#38638 = EDGE_LOOP ( 'NONE', ( #4604, #21266, #48310, #1210 ) ) ;
#38639 = EDGE_CURVE ( 'NONE', #25598, #24721, #29144, .T. ) ;
#38640 = LINE ( 'NONE', #6072, #42438 ) ;
#38641 = CARTESIAN_POINT ( 'NONE',  ( 0.000000000000000000, 68.55367621811141987, 44.99326035066078333 ) ) ;
#38642 = LINE ( 'NONE', #5105, #47858 ) ;
#38643 = ADVANCED_FACE ( 'NONE', ( #10564 ), #28905, .T. ) ;
#38644 = ORIENTED_EDGE ( 'NONE', *, *, #38033, .T. ) ;
#38645 = EDGE_CURVE ( 'NONE', #34363, #35739, #6170, .T. ) ;
#38646 = ORIENTED_EDGE ( 'NONE', *, *, #44815, .T. ) ;
#38647 = LINE ( 'NONE', #12941, #21151 ) ;
#38648 = CARTESIAN_POINT ( 'NONE',  ( 23.49916127795269460, -121.5130826919798039, 5.500000000000000000 ) ) ;
#38649 = CIRCLE ( 'NONE', #42554, 42.00000000000000000 ) ;
#38650 = AXIS2_PLACEMENT_3D ( 'NONE', #40224, #6921, #10838 ) ;
#38651 = ORIENTED_EDGE ( 'NONE', *, *, #30304, .F. ) ;
#38652 = ADVANCED_FACE ( 'NONE', ( #40185 ), #2478, .F. ) ;
#38653 = AXIS2_PLACEMENT_3D ( 'NONE', #10766, #14683, #29598 ) ;
#38654 = DIRECTION ( 'NONE',  ( -1.000000000000000000, -0.000000000000000000, 0.000000000000000000 ) ) ;
#38655 = ORIENTED_EDGE ( 'NONE', *, *, #24101, .F. ) ;
#38656 = AXIS2_PLACEMENT_3D ( 'NONE', #22700, #8263, #26140 ) ;
#38657 = LINE ( 'NONE', #16138, #41041 ) ;
#38658 = CARTESIAN_POINT ( 'NONE',  ( 11.99999999999999822, 81.34940948281335693, 10.30890764327412334 ) ) ;
#38659 = DIRECTION ( 'NONE',  ( 1.000000000000000000, -0.000000000000000000, 0.000000000000000000 ) ) ;
#38660 = CARTESIAN_POINT ( 'NONE',  ( 10.00000000000000000, 0.8261519478441983200, -77.49459641780885022 ) ) ;
#38661 = AXIS2_PLACEMENT_3D ( 'NONE', #38412, #4879, #27403 ) ;
#38662 = DIRECTION ( 'NONE',  ( -1.000000000000000000, -0.000000000000000000, -0.000000000000000000 ) ) ;
#38663 = DIRECTION ( 'NONE',  ( 1.000000000000000000, 0.000000000000000000, 0.000000000000000000 ) ) ;
#38664 = CARTESIAN_POINT ( 'NONE',  ( 10.00000000000000000, -5.202137450156655518, 37.22597642581156663 ) ) ;
#38665 = DIRECTION ( 'NONE',  ( 0.5687579148473743684, -0.8225049752423791993, 0.000000000000000000 ) ) ;
#38666 = EDGE_CURVE ( 'NONE', #15492, #15162, #2241, .T. ) ;
#38667 = ORIENTED_EDGE ( 'NONE', *, *, #17563, .F. ) ;
#38668 = FACE_OUTER_BOUND ( 'NONE', #5291, .T. ) ;
#38669 = ORIENTED_EDGE ( 'NONE', *, *, #27712, .F. ) ;
#38670 = EDGE_CURVE ( 'NONE', #551, #43487, #14223, .T. ) ;
#38671 = AXIS2_PLACEMENT_3D ( 'NONE', #26475, #11553, #34049 ) ;
#38672 = FACE_OUTER_BOUND ( 'NONE', #2307, .T. ) ;
#38673 = VECTOR ( 'NONE', #7489, 1000.000000000000000 ) ;
#38674 = CIRCLE ( 'NONE', #8148, 31.99999999999999289 ) ;
#38675 = DIRECTION ( 'NONE',  ( 0.000000000000000000, 0.4539904997395479702, -0.8910065241883673437 ) ) ;
#38676 = EDGE_CURVE ( 'NONE', #21097, #4566, #29741, .T. ) ;
#38677 = DIRECTION ( 'NONE',  ( 0.000000000000000000, 0.000000000000000000, -1.000000000000000000 ) ) ;
#38678 = ORIENTED_EDGE ( 'NONE', *, *, #27014, .T. ) ;
#38679 = EDGE_CURVE ( 'NONE', #500, #21510, #20337, .T. ) ;
#38680 = AXIS2_PLACEMENT_3D ( 'NONE', #6994, #33188, #36846 ) ;
#38681 = AXIS2_PLACEMENT_3D ( 'NONE', #29608, #47710, #48446 ) ;
#38682 = CIRCLE ( 'NONE', #44121, 31.99999999999999289 ) ;
#38683 = FACE_OUTER_BOUND ( 'NONE', #25496, .T. ) ;
#38684 = AXIS2_PLACEMENT_3D ( 'NONE', #22098, #58, #44860 ) ;
#38685 = ORIENTED_EDGE ( 'NONE', *, *, #45367, .T. ) ;
#38686 = ORIENTED_EDGE ( 'NONE', *, *, #6454, .F. ) ;
#38687 = VECTOR ( 'NONE', #15690, 1000.000000000000000 ) ;
#38688 = EDGE_LOOP ( 'NONE', ( #23682, #37766, #38201, #38848 ) ) ;
#38689 = EDGE_CURVE ( 'NONE', #27618, #45989, #35192, .T. ) ;
#38690 = LINE ( 'NONE', #12728, #4003 ) ;
#38691 = VERTEX_POINT ( 'NONE', #25220 ) ;
#38692 = EDGE_LOOP ( 'NONE', ( #8763, #14452, #23932, #8609 ) ) ;
#38693 = LINE ( 'NONE', #46513, #8265 ) ;
#38694 = ORIENTED_EDGE ( 'NONE', *, *, #13496, .T. ) ;
#38695 = EDGE_CURVE ( 'NONE', #14593, #30621, #13757, .T. ) ;
#38696 = CARTESIAN_POINT ( 'NONE',  ( -10.00000000000000000, 0.000000000000000000, 0.000000000000000000 ) ) ;
#38697 = CARTESIAN_POINT ( 'NONE',  ( 11.99999999999999822, 0.000000000000000000, 0.000000000000000000 ) ) ;
#38698 = EDGE_CURVE ( 'NONE', #14780, #842, #32812, .T. ) ;
#38699 = DIRECTION ( 'NONE',  ( -1.000000000000000000, 0.000000000000000000, 0.000000000000000000 ) ) ;
#38700 = ORIENTED_EDGE ( 'NONE', *, *, #24217, .F. ) ;
#38701 = CARTESIAN_POINT ( 'NONE',  ( 10.00000000000000000, 30.84782396557248418, -21.32104025579081252 ) ) ;
#38702 = ORIENTED_EDGE ( 'NONE', *, *, #16751, .T. ) ;
#38703 = CARTESIAN_POINT ( 'NONE',  ( 0.000000000000000000, -120.0000000000000000, 2.500000000000000000 ) ) ;
#38704 = VECTOR ( 'NONE', #5354, 1000.000000000000000 ) ;
#38705 = DIRECTION ( 'NONE',  ( -1.000000000000000000, -0.000000000000000000, -0.000000000000000000 ) ) ;
#38706 = VERTEX_POINT ( 'NONE', #36494 ) ;
#38707 = FACE_OUTER_BOUND ( 'NONE', #23551, .T. ) ;
#38708 = ORIENTED_EDGE ( 'NONE', *, *, #18381, .F. ) ;
#38709 = EDGE_LOOP ( 'NONE', ( #2381, #24689, #45383, #2117 ) ) ;
#38710 = EDGE_CURVE ( 'NONE', #16517, #44620, #45351, .T. ) ;
#38711 = CARTESIAN_POINT ( 'NONE',  ( 0.000000000000000000, 0.8261519478431083030, 77.49459641780886443 ) ) ;
#38712 = AXIS2_PLACEMENT_3D ( 'NONE', #40987, #36336, #14791 ) ;
#38713 = DIRECTION ( 'NONE',  ( 0.000000000000000000, 0.000000000000000000, 1.000000000000000000 ) ) ;
#38714 = DIRECTION ( 'NONE',  ( -1.000000000000000000, 0.000000000000000000, 0.000000000000000000 ) ) ;
#38715 = DIRECTION ( 'NONE',  ( 0.000000000000000000, 0.000000000000000000, 1.000000000000000000 ) ) ;
#38716 = CARTESIAN_POINT ( 'NONE',  ( 11.99999999999999822, 26.02418014898407961, -70.52718814184231633 ) ) ;
#38717 = FACE_OUTER_BOUND ( 'NONE', #27744, .T. ) ;
#38718 = DIRECTION ( 'NONE',  ( -1.000000000000000000, 0.000000000000000000, 0.000000000000000000 ) ) ;
#38719 = DIRECTION ( 'NONE',  ( 0.000000000000000000, 0.000000000000000000, 1.000000000000000000 ) ) ;
#38720 = ORIENTED_EDGE ( 'NONE', *, *, #46259, .T. ) ;
#38721 = AXIS2_PLACEMENT_3D ( 'NONE', #17032, #47605, #5790 ) ;
#38722 = DIRECTION ( 'NONE',  ( 0.000000000000000000, 0.000000000000000000, 1.000000000000000000 ) ) ;
#38723 = LINE ( 'NONE', #5184, #25589 ) ;
#38724 = DIRECTION ( 'NONE',  ( 0.000000000000000000, 0.000000000000000000, 1.000000000000000000 ) ) ;
#38725 = AXIS2_PLACEMENT_3D ( 'NONE', #42618, #39172, #28643 ) ;
#38726 = DIRECTION ( 'NONE',  ( 0.000000000000000000, 0.000000000000000000, 1.000000000000000000 ) ) ;
#38727 = CARTESIAN_POINT ( 'NONE',  ( 10.00000000000000000, -39.78640506895559525, -66.50666863322042843 ) ) ;
#38728 = FACE_OUTER_BOUND ( 'NONE', #1843, .T. ) ;
#38729 = DIRECTION ( 'NONE',  ( -1.000000000000000000, 0.000000000000000000, 0.000000000000000000 ) ) ;
#38730 = TOROIDAL_SURFACE ( 'NONE', #6675, 20.69999999999999929, 0.2999999999999981570 ) ;
#38731 = AXIS2_PLACEMENT_3D ( 'NONE', #4191, #45528, #738 ) ;
#38732 = VERTEX_POINT ( 'NONE', #17164 ) ;
#38733 = ORIENTED_EDGE ( 'NONE', *, *, #28713, .T. ) ;
#38734 = DIRECTION ( 'NONE',  ( 1.000000000000000000, 0.000000000000000000, 0.000000000000000000 ) ) ;
#38735 = VERTEX_POINT ( 'NONE', #35545 ) ;
#38736 = DIRECTION ( 'NONE',  ( -1.000000000000000000, 0.000000000000000000, -0.000000000000000000 ) ) ;
#38737 = PRODUCT_CONTEXT ( 'NONE', #13219, 'mechanical' ) ;
#38738 = AXIS2_PLACEMENT_3D ( 'NONE', #7086, #11505, #26431 ) ;
#38739 = CARTESIAN_POINT ( 'NONE',  ( 10.00000000000000000, 37.58145647212455032, -0.6853352020786441789 ) ) ;
#38740 = ORIENTED_EDGE ( 'NONE', *, *, #38577, .F. ) ;
#38741 = CIRCLE ( 'NONE', #32512, 16.00000000000000000 ) ;
#38742 = ORIENTED_EDGE ( 'NONE', *, *, #42011, .F. ) ;
#38743 = DIRECTION ( 'NONE',  ( 0.000000000000000000, 0.4999999999999931166, -0.8660254037844427044 ) ) ;
#38744 = ORIENTED_EDGE ( 'NONE', *, *, #2909, .F. ) ;
#38745 = AXIS2_PLACEMENT_3D ( 'NONE', #10134, #48299, #43671 ) ;
#38746 = DIRECTION ( 'NONE',  ( 0.000000000000000000, 0.4539904997395479702, -0.8910065241883673437 ) ) ;
#38747 = VERTEX_POINT ( 'NONE', #6403 ) ;
#38748 = FACE_OUTER_BOUND ( 'NONE', #29562, .T. ) ;
#38749 = ORIENTED_EDGE ( 'NONE', *, *, #23369, .F. ) ;
#38750 = CARTESIAN_POINT ( 'NONE',  ( 24.95699195200416654, -110.9640411295978595, 5.500000000000000000 ) ) ;
#38751 = ORIENTED_EDGE ( 'NONE', *, *, #47268, .T. ) ;
#38752 = CIRCLE ( 'NONE', #41092, 31.99999999999998579 ) ;
#38753 = EDGE_CURVE ( 'NONE', #5836, #29992, #5940, .T. ) ;
#38754 = CARTESIAN_POINT ( 'NONE',  ( 0.000000000000000000, -17.80606268964516659, -33.00180498840066434 ) ) ;
#38755 = AXIS2_PLACEMENT_3D ( 'NONE', #47816, #29234, #14301 ) ;
#38756 = AXIS2_PLACEMENT_3D ( 'NONE', #20802, #42349, #23742 ) ;
#38757 = DIRECTION ( 'NONE',  ( -1.000000000000000000, -0.000000000000000000, -0.000000000000000000 ) ) ;
#38758 = DIRECTION ( 'NONE',  ( -0.1276937514489679404, -0.9918136447140103451, 0.000000000000000000 ) ) ;
#38759 = DIRECTION ( 'NONE',  ( -0.1276937514489679404, -0.9918136447140103451, 0.000000000000000000 ) ) ;
#38760 = EDGE_CURVE ( 'NONE', #26898, #12813, #16940, .T. ) ;
#38761 = CARTESIAN_POINT ( 'NONE',  ( 0.000000000000000000, -26.01480285779885904, 70.53064760720306481 ) ) ;
#38762 = ORIENTED_EDGE ( 'NONE', *, *, #11353, .F. ) ;
#38763 = DIRECTION ( 'NONE',  ( -1.000000000000000000, 0.000000000000000000, 0.000000000000000000 ) ) ;
#38764 = EDGE_LOOP ( 'NONE', ( #33363, #10748, #33643, #32311 ) ) ;
#38765 = VERTEX_POINT ( 'NONE', #13272 ) ;
#38766 = ADVANCED_FACE ( 'NONE', ( #39466 ), #32122, .F. ) ;
#38767 = LINE ( 'NONE', #8165, #20786 ) ;
#38768 = DIRECTION ( 'NONE',  ( 1.000000000000000000, -0.000000000000000000, 0.000000000000000000 ) ) ;
#38769 = VECTOR ( 'NONE', #13674, 1000.000000000000000 ) ;
#38770 = EDGE_CURVE ( 'NONE', #22704, #13285, #24263, .T. ) ;
#38771 = DIRECTION ( 'NONE',  ( 1.000000000000000000, -0.000000000000000000, -0.000000000000000000 ) ) ;
#38772 = DIRECTION ( 'NONE',  ( 1.000000000000000000, 0.000000000000000000, 0.000000000000000000 ) ) ;
#38773 = ORIENTED_EDGE ( 'NONE', *, *, #25228, .F. ) ;
#38774 = DIRECTION ( 'NONE',  ( 0.000000000000000000, 0.000000000000000000, -1.000000000000000000 ) ) ;
#38775 = VECTOR ( 'NONE', #2819, 1000.000000000000000 ) ;
#38776 = CARTESIAN_POINT ( 'NONE',  ( 11.99999999999999822, 26.01480285779933510, -70.53064760720289428 ) ) ;
#38777 = CARTESIAN_POINT ( 'NONE',  ( 10.00000000000000000, 80.28980883073779751, -16.65972982744850839 ) ) ;
#38778 = CARTESIAN_POINT ( 'NONE',  ( 10.00000000000000000, -73.44644590900078640, 24.73286445877676343 ) ) ;
#38779 = AXIS2_PLACEMENT_3D ( 'NONE', #7638, #22568, #33808 ) ;
#38780 = DIRECTION ( 'NONE',  ( 1.000000000000000000, 0.000000000000000000, -0.000000000000000000 ) ) ;
#38781 = DIRECTION ( 'NONE',  ( 1.000000000000000000, 0.000000000000000000, 0.000000000000000000 ) ) ;
#38782 = DIRECTION ( 'NONE',  ( 0.000000000000000000, 0.7071067811865487940, -0.7071067811865462405 ) ) ;
#38783 = CARTESIAN_POINT ( 'NONE',  ( 0.000000000000000000, -10.45096189432344147, 21.10159698893426494 ) ) ;
#38784 = CARTESIAN_POINT ( 'NONE',  ( 15.00000000000000000, -11.95096189432345746, -23.69967320028757030 ) ) ;
#38785 = DIRECTION ( 'NONE',  ( -1.000000000000000000, -0.000000000000000000, 0.000000000000000000 ) ) ;
#38786 = ORIENTED_EDGE ( 'NONE', *, *, #7642, .T. ) ;
#38787 = VECTOR ( 'NONE', #12984, 1000.000000000000000 ) ;
#38788 = CARTESIAN_POINT ( 'NONE',  ( 10.00000000000000000, -5.202137450156129717, -37.22597642581163768 ) ) ;
#38789 = ORIENTED_EDGE ( 'NONE', *, *, #20173, .T. ) ;
#38790 = DIRECTION ( 'NONE',  ( -1.000000000000000000, 0.000000000000000000, 0.000000000000000000 ) ) ;
#38791 = AXIS2_PLACEMENT_3D ( 'NONE', #33089, #22068, #37493 ) ;
#38792 = DIRECTION ( 'NONE',  ( -1.000000000000000000, -0.000000000000000000, 0.000000000000000000 ) ) ;
#38793 = AXIS2_PLACEMENT_3D ( 'NONE', #42126, #19831, #20088 ) ;
#38794 = EDGE_LOOP ( 'NONE', ( #14453, #2525, #27539, #9698 ) ) ;
#38795 = EDGE_CURVE ( 'NONE', #34997, #45805, #2720, .T. ) ;
#38796 = ADVANCED_FACE ( 'NONE', ( #13983 ), #31047, .T. ) ;
#38797 = ORIENTED_EDGE ( 'NONE', *, *, #26364, .F. ) ;
#38798 = AXIS2_PLACEMENT_3D ( 'NONE', #33346, #27696, #31135 ) ;
#38799 = ORIENTED_EDGE ( 'NONE', *, *, #11007, .T. ) ;
#38800 = VERTEX_POINT ( 'NONE', #45964 ) ;
#38801 = AXIS2_PLACEMENT_3D ( 'NONE', #2253, #28442, #17172 ) ;
#38802 = EDGE_LOOP ( 'NONE', ( #22085, #24451, #35926, #13910 ) ) ;
#38803 = EDGE_CURVE ( 'NONE', #2295, #31513, #19549, .T. ) ;
#38804 = VERTEX_POINT ( 'NONE', #21799 ) ;
#38805 = AXIS2_PLACEMENT_3D ( 'NONE', #16864, #43289, #20517 ) ;
#38806 = CARTESIAN_POINT ( 'NONE',  ( -26.53422223201112828, -120.6595836127786043, -5.500000000000000000 ) ) ;
#38807 = LINE ( 'NONE', #30983, #40636 ) ;
#38808 = CARTESIAN_POINT ( 'NONE',  ( 0.000000000000000000, 0.000000000000000000, 0.000000000000000000 ) ) ;
#38809 = EDGE_LOOP ( 'NONE', ( #41811, #40643, #11870, #18675 ) ) ;
#38810 = FACE_OUTER_BOUND ( 'NONE', #36684, .T. ) ;
#38811 = ORIENTED_EDGE ( 'NONE', *, *, #42885, .F. ) ;
#38812 = EDGE_CURVE ( 'NONE', #3154, #41890, #11949, .T. ) ;
#38813 = ORIENTED_EDGE ( 'NONE', *, *, #40179, .T. ) ;
#38814 = EDGE_CURVE ( 'NONE', #6843, #39485, #7053, .T. ) ;
#38815 = EDGE_CURVE ( 'NONE', #30126, #39866, #13326, .T. ) ;
#38816 = CYLINDRICAL_SURFACE ( 'NONE', #14742, 31.99999999999998579 ) ;
#38817 = CARTESIAN_POINT ( 'NONE',  ( 5.000000000000002665, -71.21200624218825226, 40.65526001592589722 ) ) ;
#38818 = CARTESIAN_POINT ( 'NONE',  ( -12.49999999999999645, 0.000000000000000000, -43.79999999999998295 ) ) ;
#38819 = ORIENTED_EDGE ( 'NONE', *, *, #27180, .F. ) ;
#38820 = ORIENTED_EDGE ( 'NONE', *, *, #7949, .T. ) ;
#38821 = ORIENTED_EDGE ( 'NONE', *, *, #40061, .T. ) ;
#38822 = LINE ( 'NONE', #13577, #8326 ) ;
#38823 = ORIENTED_EDGE ( 'NONE', *, *, #44797, .F. ) ;
#38824 = CARTESIAN_POINT ( 'NONE',  ( 10.00000000000000000, -71.91182617369207719, 28.89263327155721228 ) ) ;
#38825 = CARTESIAN_POINT ( 'NONE',  ( 0.000000000000000000, 75.11764819372149304, 29.05362095685338275 ) ) ;
#38826 = FACE_OUTER_BOUND ( 'NONE', #31051, .T. ) ;
#38827 = CARTESIAN_POINT ( 'NONE',  ( 10.00000000000000000, -37.01155633439063308, 6.555932627142289526 ) ) ;
#38828 = LINE ( 'NONE', #8946, #10982 ) ;
#38829 = PLANE ( 'NONE',  #39320 ) ;
#38830 = DIRECTION ( 'NONE',  ( 0.000000000000000000, 0.000000000000000000, 1.000000000000000000 ) ) ;
#38831 = VERTEX_POINT ( 'NONE', #907 ) ;
#38832 = CARTESIAN_POINT ( 'NONE',  ( 0.000000000000000000, -13.04903810567675038, 19.60159698893425428 ) ) ;
#38834 = EDGE_CURVE ( 'NONE', #31692, #30064, #46944, .T. ) ;
#38833 = DIRECTION ( 'NONE',  ( 0.000000000000000000, 0.000000000000000000, -1.000000000000000000 ) ) ;
#38835 = DIRECTION ( 'NONE',  ( -1.000000000000000000, -0.000000000000000000, 0.000000000000000000 ) ) ;
#38836 = DIRECTION ( 'NONE',  ( -0.8774505977381971134, -0.4796670183876317051, 0.000000000000000000 ) ) ;
#38837 = ORIENTED_EDGE ( 'NONE', *, *, #18559, .T. ) ;
#38838 = CIRCLE ( 'NONE', #45850, 35.50000000000001421 ) ;
#38839 = FACE_OUTER_BOUND ( 'NONE', #38343, .T. ) ;
#38840 = DIRECTION ( 'NONE',  ( 0.000000000000000000, 0.000000000000000000, 1.000000000000000000 ) ) ;
#38841 = DIRECTION ( 'NONE',  ( 0.000000000000000000, 0.9876883405951372152, 0.1564344650402347547 ) ) ;
#38842 = CIRCLE ( 'NONE', #29456, 77.49900000000000944 ) ;
#38843 = DIRECTION ( 'NONE',  ( -1.000000000000000000, -0.000000000000000000, 0.000000000000000000 ) ) ;
#38844 = DIRECTION ( 'NONE',  ( -1.000000000000000000, 0.000000000000000000, 0.000000000000000000 ) ) ;
#38845 = CIRCLE ( 'NONE', #2867, 31.99999999999999289 ) ;
#38846 = DIRECTION ( 'NONE',  ( -1.000000000000000000, 0.000000000000000000, 0.000000000000000000 ) ) ;
#38847 = DIRECTION ( 'NONE',  ( 0.000000000000000000, 0.000000000000000000, -1.000000000000000000 ) ) ;
#38848 = ORIENTED_EDGE ( 'NONE', *, *, #22823, .T. ) ;
#38849 = EDGE_LOOP ( 'NONE', ( #25610, #30663, #8454, #30709 ) ) ;
#38850 = CARTESIAN_POINT ( 'NONE',  ( 0.000000000000000000, -20.40083707022935400, 72.35432306680478121 ) ) ;
#38851 = ORIENTED_EDGE ( 'NONE', *, *, #35031, .T. ) ;
#38852 = EDGE_CURVE ( 'NONE', #41614, #2440, #8502, .T. ) ;
#38853 = VERTEX_POINT ( 'NONE', #23432 ) ;
#38854 = VERTEX_POINT ( 'NONE', #11701 ) ;
#38855 = EDGE_CURVE ( 'NONE', #2592, #47874, #38370, .T. ) ;
#38856 = VECTOR ( 'NONE', #31812, 1000.000000000000000 ) ;
#38857 = CARTESIAN_POINT ( 'NONE',  ( 15.00000000000000000, -20.55727247249748402, -16.78983467731284307 ) ) ;
#38858 = ORIENTED_EDGE ( 'NONE', *, *, #18228, .T. ) ;
#38859 = ADVANCED_FACE ( 'NONE', ( #680 ), #45235, .F. ) ;
#38860 = CIRCLE ( 'NONE', #33362, 31.99999999999998579 ) ;
#38861 = CARTESIAN_POINT ( 'NONE',  ( 0.000000000000000000, 80.55351364060589958, 15.33399622253512540 ) ) ;
#38862 = FACE_OUTER_BOUND ( 'NONE', #11100, .T. ) ;
#38863 = VERTEX_POINT ( 'NONE', #45000 ) ;
#38864 = ORIENTED_EDGE ( 'NONE', *, *, #40369, .T. ) ;
#38865 = ORIENTED_EDGE ( 'NONE', *, *, #38632, .T. ) ;
#38866 = AXIS2_PLACEMENT_3D ( 'NONE', #42985, #9434, #24371 ) ;
#38867 = EDGE_CURVE ( 'NONE', #30648, #36833, #44624, .T. ) ;
#38868 = EDGE_CURVE ( 'NONE', #11582, #12094, #3998, .T. ) ;
#38869 = DIRECTION ( 'NONE',  ( -0.9966891607226785466, -0.08130631524009969413, 0.000000000000000000 ) ) ;
#38871 = ORIENTED_EDGE ( 'NONE', *, *, #6209, .T. ) ;
#38870 = DIRECTION ( 'NONE',  ( -0.000000000000000000, -0.5877852522924789103, 0.8090169943749432324 ) ) ;
#38872 = VECTOR ( 'NONE', #20950, 1000.000000000000000 ) ;
#38873 = DIRECTION ( 'NONE',  ( 0.000000000000000000, 0.000000000000000000, 1.000000000000000000 ) ) ;
#38874 = ORIENTED_EDGE ( 'NONE', *, *, #37007, .F. ) ;
#38875 = VERTEX_POINT ( 'NONE', #19032 ) ;
#38876 = DIRECTION ( 'NONE',  ( -1.000000000000000000, 0.000000000000000000, 0.000000000000000000 ) ) ;
#38877 = EDGE_LOOP ( 'NONE', ( #45448, #11371, #57, #37139 ) ) ;
#38878 = EDGE_LOOP ( 'NONE', ( #37637, #47393, #24910, #32824 ) ) ;
#38879 = CARTESIAN_POINT ( 'NONE',  ( 10.00000000000000178, 12.24744871391589029, 2.500000000000004441 ) ) ;
#38880 = CARTESIAN_POINT ( 'NONE',  ( -7.572224309238338336, -145.4393675041377492, 5.500000000000000000 ) ) ;
#38881 = EDGE_LOOP ( 'NONE', ( #7283, #29867, #28064, #35944 ) ) ;
#38882 = DIRECTION ( 'NONE',  ( 1.000000000000000000, 0.000000000000000000, 0.000000000000000000 ) ) ;
#38883 = CARTESIAN_POINT ( 'NONE',  ( 0.000000000000000000, 0.000000000000000000, 0.000000000000000000 ) ) ;
#38884 = DIRECTION ( 'NONE',  ( -1.000000000000000000, 0.000000000000000000, 0.000000000000000000 ) ) ;
#38885 = ORIENTED_EDGE ( 'NONE', *, *, #7746, .T. ) ;
#38886 = VERTEX_POINT ( 'NONE', #19743 ) ;
#38887 = DIRECTION ( 'NONE',  ( 0.000000000000000000, 0.000000000000000000, 1.000000000000000000 ) ) ;
#38888 = EDGE_CURVE ( 'NONE', #42505, #9989, #22709, .T. ) ;
#38889 = CARTESIAN_POINT ( 'NONE',  ( 11.99999999999999822, -35.91791733033428358, -68.67312586195033930 ) ) ;
#38890 = VECTOR ( 'NONE', #15995, 1000.000000000000000 ) ;
#38891 = VERTEX_POINT ( 'NONE', #16115 ) ;
#38892 = CARTESIAN_POINT ( 'NONE',  ( 10.00000000000000000, 81.90746397400394585, -3.894527615416976118 ) ) ;
#38893 = ORIENTED_EDGE ( 'NONE', *, *, #20974, .T. ) ;
#38894 = DIRECTION ( 'NONE',  ( -1.000000000000000000, 0.000000000000000000, 0.000000000000000000 ) ) ;
#38895 = VECTOR ( 'NONE', #22925, 1000.000000000000000 ) ;
#38896 = CARTESIAN_POINT ( 'NONE',  ( 0.000000000000000000, 0.000000000000000000, 0.000000000000000000 ) ) ;
#38897 = LINE ( 'NONE', #41838, #15967 ) ;
#38898 = CARTESIAN_POINT ( 'NONE',  ( -3.000000000000000000, -23.29833615347104825, -3.418703333116803744 ) ) ;
#38899 = LINE ( 'NONE', #27630, #25981 ) ;
#38900 = DIRECTION ( 'NONE',  ( 0.000000000000000000, 0.3826834323650840086, 0.9238795325112891810 ) ) ;
#38901 = CIRCLE ( 'NONE', #12345, 42.00000000000000000 ) ;
#38902 = DIRECTION ( 'NONE',  ( 0.000000000000000000, 0.000000000000000000, 1.000000000000000000 ) ) ;
#38903 = CYLINDRICAL_SURFACE ( 'NONE', #34022, 31.99999999999999289 ) ;
#38904 = VERTEX_POINT ( 'NONE', #30068 ) ;
#38905 = CARTESIAN_POINT ( 'NONE',  ( 0.000000000000000000, -41.76106447765443619, -62.50884508063471401 ) ) ;
#38906 =( LENGTH_UNIT ( ) NAMED_UNIT ( * ) SI_UNIT ( .MILLI., .METRE. ) );
#38907 = ORIENTED_EDGE ( 'NONE', *, *, #33977, .F. ) ;
#38908 = CIRCLE ( 'NONE', #24049, 77.49899999999999523 ) ;
#38909 = PLANE ( 'NONE',  #33946 ) ;
#38910 = ORIENTED_EDGE ( 'NONE', *, *, #38021, .F. ) ;
#38911 = EDGE_CURVE ( 'NONE', #29613, #46719, #8017, .T. ) ;
#38912 = CYLINDRICAL_SURFACE ( 'NONE', #34281, 31.99999999999998579 ) ;
#38913 = DIRECTION ( 'NONE',  ( 0.000000000000000000, -0.5877852522924625900, -0.8090169943749551118 ) ) ;
#38914 = EDGE_CURVE ( 'NONE', #26793, #14170, #36785, .T. ) ;
#38915 = VERTEX_POINT ( 'NONE', #11477 ) ;
#38916 = EDGE_CURVE ( 'NONE', #42004, #12188, #837, .T. ) ;
#38917 = AXIS2_PLACEMENT_3D ( 'NONE', #28448, #38763, #13053 ) ;
#38918 = ADVANCED_FACE ( 'NONE', ( #15390 ), #4375, .F. ) ;
#38919 = CARTESIAN_POINT ( 'NONE',  ( 10.00000000000000000, -27.74655509720617275, -77.16300072079690153 ) ) ;
#38920 = VECTOR ( 'NONE', #9435, 1000.000000000000000 ) ;
#38921 = AXIS2_PLACEMENT_3D ( 'NONE', #20738, #35413, #12672 ) ;
#38922 = VERTEX_POINT ( 'NONE', #28085 ) ;
#38923 = ORIENTED_EDGE ( 'NONE', *, *, #16762, .F. ) ;
#38924 = VERTEX_POINT ( 'NONE', #34936 ) ;
#38925 = EDGE_CURVE ( 'NONE', #41627, #40068, #38624, .T. ) ;
#38926 = CARTESIAN_POINT ( 'NONE',  ( 0.000000000000000000, 55.20638768913760686, 51.02545421589343988 ) ) ;
#38927 = EDGE_LOOP ( 'NONE', ( #41892, #36059, #47452, #18012 ) ) ;
#38928 = ORIENTED_EDGE ( 'NONE', *, *, #19942, .F. ) ;
#38929 = LINE ( 'NONE', #733, #23920 ) ;
#38930 = EDGE_CURVE ( 'NONE', #11405, #43300, #8993, .T. ) ;
#38931 = ORIENTED_EDGE ( 'NONE', *, *, #12554, .F. ) ;
#38932 = CARTESIAN_POINT ( 'NONE',  ( 10.00000000000000000, -62.20884554313985149, -46.21855187248698371 ) ) ;
#38933 = LINE ( 'NONE', #5390, #11403 ) ;
#38934 = PRESENTATION_LAYER_ASSIGNMENT (  '', '', ( #41345 ) ) ;
#38935 = CARTESIAN_POINT ( 'NONE',  ( 10.00000000000000000, -0.8828120875898013420, -37.48860685352291711 ) ) ;
#38936 = ORIENTED_EDGE ( 'NONE', *, *, #35025, .T. ) ;
#38937 = DIRECTION ( 'NONE',  ( 0.000000000000000000, 0.000000000000000000, 1.000000000000000000 ) ) ;
#38938 = VERTEX_POINT ( 'NONE', #13152 ) ;
#38939 = VECTOR ( 'NONE', #37931, 1000.000000000000000 ) ;
#38940 = DIRECTION ( 'NONE',  ( 0.000000000000000000, 0.000000000000000000, 1.000000000000000000 ) ) ;
#38941 = ADVANCED_FACE ( 'NONE', ( #20739 ), #9708, .F. ) ;
#38942 = CARTESIAN_POINT ( 'NONE',  ( 10.00000000000000000, 0.000000000000000000, 0.000000000000000000 ) ) ;
#38943 = ORIENTED_EDGE ( 'NONE', *, *, #6865, .T. ) ;
#38944 = DIRECTION ( 'NONE',  ( -1.000000000000000000, -0.000000000000000000, 0.000000000000000000 ) ) ;
#38945 = ORIENTED_EDGE ( 'NONE', *, *, #1548, .F. ) ;
#38946 = ORIENTED_EDGE ( 'NONE', *, *, #43755, .F. ) ;
#38947 = DIRECTION ( 'NONE',  ( -1.000000000000000000, 0.000000000000000000, 0.000000000000000000 ) ) ;
#38948 = CARTESIAN_POINT ( 'NONE',  ( 0.000000000000000000, 41.19522573413826194, -65.64334221924865176 ) ) ;
#38949 = CARTESIAN_POINT ( 'NONE',  ( 0.000000000000000000, -59.03961581697367933, -46.53671651294010303 ) ) ;
#38950 = CARTESIAN_POINT ( 'NONE',  ( -3.000000000000000000, 22.07842321921481243, 8.187992925817422218 ) ) ;
#38951 = DIRECTION ( 'NONE',  ( 1.000000000000000000, 0.000000000000000000, 0.000000000000000000 ) ) ;
#38952 = DIRECTION ( 'NONE',  ( 0.000000000000000000, 0.000000000000000000, 1.000000000000000000 ) ) ;
#38953 = DIRECTION ( 'NONE',  ( -1.000000000000000000, -0.000000000000000000, 0.000000000000000000 ) ) ;
#38954 = DIRECTION ( 'NONE',  ( 0.000000000000000000, 0.1564344650402311743, -0.9876883405951377704 ) ) ;
#38955 = ADVANCED_FACE ( 'NONE', ( #12673 ), #2141, .T. ) ;
#38956 = AXIS2_PLACEMENT_3D ( 'NONE', #12508, #16414, #27439 ) ;
#38957 = DIRECTION ( 'NONE',  ( -0.000000000000000000, -0.000000000000000000, -1.000000000000000000 ) ) ;
#38958 = LINE ( 'NONE', #42867, #48280 ) ;
#38959 = LINE ( 'NONE', #16912, #18444 ) ;
#38960 = PRESENTATION_LAYER_ASSIGNMENT (  '', '', ( #17063 ) ) ;
#38961 = CARTESIAN_POINT ( 'NONE',  ( 15.00000000000000000, 5.835314593368470248, -22.81335362449854642 ) ) ;
#38962 = LINE ( 'NONE', #5419, #13653 ) ;
#38963 = CYLINDRICAL_SURFACE ( 'NONE', #10042, 82.00000000000000000 ) ;
#38964 = DIRECTION ( 'NONE',  ( -1.000000000000000000, 0.000000000000000000, -0.000000000000000000 ) ) ;
#38965 = VERTEX_POINT ( 'NONE', #24398 ) ;
#38966 = ORIENTED_EDGE ( 'NONE', *, *, #44310, .F. ) ;
#38967 = DIRECTION ( 'NONE',  ( 1.000000000000000000, 0.000000000000000000, 0.000000000000000000 ) ) ;
#38968 = ADVANCED_FACE ( 'NONE', ( #39336 ), #35669, .T. ) ;
#38969 = DIRECTION ( 'NONE',  ( 0.000000000000000000, 0.000000000000000000, 1.000000000000000000 ) ) ;
#38970 = EDGE_CURVE ( 'NONE', #2738, #12730, #5562, .T. ) ;
#38971 = AXIS2_PLACEMENT_3D ( 'NONE', #17931, #40952, #26002 ) ;
#38972 = DIRECTION ( 'NONE',  ( -1.000000000000000000, 0.000000000000000000, 0.000000000000000000 ) ) ;
#38973 = ORIENTED_EDGE ( 'NONE', *, *, #3201, .F. ) ;
#38974 = EDGE_CURVE ( 'NONE', #37711, #16641, #5817, .T. ) ;
#38975 = AXIS2_PLACEMENT_3D ( 'NONE', #40466, #44605, #14517 ) ;
#38976 = EDGE_CURVE ( 'NONE', #2457, #13396, #23931, .T. ) ;
#38977 = CARTESIAN_POINT ( 'NONE',  ( 0.000000000000000000, -120.0000000000000000, -2.500000000000000000 ) ) ;
#38978 = CARTESIAN_POINT ( 'NONE',  ( 26.09152095774781799, -124.8716048804687375, -5.500000000000000000 ) ) ;
#38979 = VERTEX_POINT ( 'NONE', #27861 ) ;
#38980 = LINE ( 'NONE', #17649, #46914 ) ;
#38981 = LINE ( 'NONE', #17163, #1072 ) ;
#38982 = CARTESIAN_POINT ( 'NONE',  ( 15.00000000000000000, -22.67460108101782978, -6.353146135317906840 ) ) ;
#38983 = ORIENTED_EDGE ( 'NONE', *, *, #29985, .F. ) ;
#38984 = CARTESIAN_POINT ( 'NONE',  ( -14.09999999999999964, 1.726751986797767995E-15, 0.000000000000000000 ) ) ;
#38985 = ORIENTED_EDGE ( 'NONE', *, *, #506, .T. ) ;
#38986 = VECTOR ( 'NONE', #12475, 1000.000000000000000 ) ;
#38987 = CIRCLE ( 'NONE', #43661, 77.49899999999999523 ) ;
#38988 = PLANE ( 'NONE',  #38450 ) ;
#38989 = CARTESIAN_POINT ( 'NONE',  ( -11.99999999999999645, 0.000000000000000000, -20.69999999999999929 ) ) ;
#38990 = CARTESIAN_POINT ( 'NONE',  ( 15.00000000000000000, 5.835314593368777558, 22.81335362449846471 ) ) ;
#38991 = DIRECTION ( 'NONE',  ( 0.000000000000000000, 0.7604059656000323741, -0.6494480483301819929 ) ) ;
#38992 = CARTESIAN_POINT ( 'NONE',  ( -2.977765906491215642, 0.000000000000000000, 0.000000000000000000 ) ) ;
#38993 = ORIENTED_EDGE ( 'NONE', *, *, #11424, .T. ) ;
#38994 = CYLINDRICAL_SURFACE ( 'NONE', #13129, 0.5000000000000004441 ) ;
#38995 = ORIENTED_EDGE ( 'NONE', *, *, #2270, .T. ) ;
#38996 = ORIENTED_EDGE ( 'NONE', *, *, #34515, .T. ) ;
#38997 = CARTESIAN_POINT ( 'NONE',  ( 6.782329983125267248, 10.49999999999999645, -105.0000000000000000 ) ) ;
#38998 = DIRECTION ( 'NONE',  ( -1.000000000000000000, -0.000000000000000000, -0.000000000000000000 ) ) ;
#38999 = CYLINDRICAL_SURFACE ( 'NONE', #48, 37.49900000000000233 ) ;
#39000 = DIRECTION ( 'NONE',  ( -0.8774505977381971134, -0.4796670183876317051, 0.000000000000000000 ) ) ;
#39001 = ORIENTED_EDGE ( 'NONE', *, *, #21571, .T. ) ;
#39002 = CARTESIAN_POINT ( 'NONE',  ( 10.00000000000000000, 0.000000000000000000, 0.000000000000000000 ) ) ;
#39003 = CARTESIAN_POINT ( 'NONE',  ( 0.000000000000000000, -0.8299999999999999600, -1.199999999999999956 ) ) ;
#39004 = CARTESIAN_POINT ( 'NONE',  ( 10.00000000000000000, 21.32104025579158701, -30.84782396557194772 ) ) ;
#39005 = DIRECTION ( 'NONE',  ( 1.000000000000000000, 0.000000000000000000, 0.000000000000000000 ) ) ;
#39006 = DIRECTION ( 'NONE',  ( -1.000000000000000000, -0.000000000000000000, 0.000000000000000000 ) ) ;
#39007 = EDGE_CURVE ( 'NONE', #35670, #7892, #20973, .T. ) ;
#39008 = DIRECTION ( 'NONE',  ( 1.000000000000000000, 0.000000000000000000, 0.000000000000000000 ) ) ;
#39009 = DIRECTION ( 'NONE',  ( 0.000000000000000000, 0.000000000000000000, 1.000000000000000000 ) ) ;
#39010 = CARTESIAN_POINT ( 'NONE',  ( 0.000000000000000000, -59.46389618801928378, -49.70050353004953791 ) ) ;
#39011 = DIRECTION ( 'NONE',  ( 0.000000000000000000, 0.000000000000000000, -1.000000000000000000 ) ) ;
#39012 = CARTESIAN_POINT ( 'NONE',  ( 10.00000000000000000, 0.000000000000000000, 0.000000000000000000 ) ) ;
#39013 = ORIENTED_EDGE ( 'NONE', *, *, #1455, .F. ) ;
#39014 = VERTEX_POINT ( 'NONE', #1906 ) ;
#39015 = DIRECTION ( 'NONE',  ( -0.000000000000000000, -0.000000000000000000, -1.000000000000000000 ) ) ;
#39016 = VECTOR ( 'NONE', #39148, 1000.000000000000114 ) ;
#39017 = ORIENTED_EDGE ( 'NONE', *, *, #24458, .F. ) ;
#39018 = EDGE_CURVE ( 'NONE', #15250, #9384, #38375, .T. ) ;
#39019 = CARTESIAN_POINT ( 'NONE',  ( 0.000000000000000000, -26.02418014898359289, 70.52718814184250107 ) ) ;
#39020 = AXIS2_PLACEMENT_3D ( 'NONE', #21437, #17272, #47146 ) ;
#39021 = ADVANCED_FACE ( 'NONE', ( #46926 ), #24168, .T. ) ;
#39022 = CARTESIAN_POINT ( 'NONE',  ( 0.000000000000000000, 65.59268652807210742, 36.72794159290264560 ) ) ;
#39023 = ORIENTED_EDGE ( 'NONE', *, *, #2379, .T. ) ;
#39024 = ADVANCED_FACE ( 'NONE', ( #47161 ), #5088, .T. ) ;
#39025 = DIRECTION ( 'NONE',  ( 0.000000000000000000, -0.9238795325112821866, -0.3826834323651008285 ) ) ;
#39027 = EDGE_CURVE ( 'NONE', #37662, #36450, #40706, .T. ) ;
#39026 = ORIENTED_EDGE ( 'NONE', *, *, #26687, .T. ) ;
#39028 = ORIENTED_EDGE ( 'NONE', *, *, #35331, .T. ) ;
#39029 = PRESENTATION_LAYER_ASSIGNMENT (  '', '', ( #11679 ) ) ;
#39030 = CARTESIAN_POINT ( 'NONE',  ( 5.000000000000000000, -77.16300072079681627, 27.74655509720641078 ) ) ;
#39031 = FACE_OUTER_BOUND ( 'NONE', #42707, .T. ) ;
#39033 = ORIENTED_EDGE ( 'NONE', *, *, #7150, .T. ) ;
#39032 = CARTESIAN_POINT ( 'NONE',  ( 10.00000000000000000, 28.89263327155746097, 71.91182617369197771 ) ) ;
#39034 = EDGE_CURVE ( 'NONE', #45238, #7713, #16341, .T. ) ;
#39035 = ORIENTED_EDGE ( 'NONE', *, *, #26244, .T. ) ;
#39036 = CARTESIAN_POINT ( 'NONE',  ( -6.880223345695647197, -142.5202692415819854, 5.500000000000000000 ) ) ;
#39037 = VERTEX_POINT ( 'NONE', #5331 ) ;
#39038 = EDGE_LOOP ( 'NONE', ( #42073, #29812, #33305, #8383 ) ) ;
#39039 = CARTESIAN_POINT ( 'NONE',  ( -8.452893869119503023, -12.51233732111638375, -1.199999999999999956 ) ) ;
#39040 = LINE ( 'NONE', #2086, #11408 ) ;
#39041 = CARTESIAN_POINT ( 'NONE',  ( 11.99999999999999822, -68.55367621811173251, 44.99326035066031437 ) ) ;
#39042 = VECTOR ( 'NONE', #39680, 1000.000000000000000 ) ;
#39043 = ORIENTED_EDGE ( 'NONE', *, *, #42753, .F. ) ;
#39044 = VERTEX_POINT ( 'NONE', #20247 ) ;
#39045 = VECTOR ( 'NONE', #27352, 1000.000000000000227 ) ;
#39046 = DIRECTION ( 'NONE',  ( -1.000000000000000000, 0.000000000000000000, 0.000000000000000000 ) ) ;
#39047 = ORIENTED_EDGE ( 'NONE', *, *, #10211, .F. ) ;
#39048 = CYLINDRICAL_SURFACE ( 'NONE', #35599, 77.49899999999999523 ) ;
#39049 = VECTOR ( 'NONE', #43370, 1000.000000000000000 ) ;
#39050 = DIRECTION ( 'NONE',  ( 0.000000000000000000, -0.8090169943749504489, 0.5877852522924689183 ) ) ;
#39051 = DIRECTION ( 'NONE',  ( -1.000000000000000000, -0.000000000000000000, -0.000000000000000000 ) ) ;
#39052 = CYLINDRICAL_SURFACE ( 'NONE', #5008, 77.49899999999999523 ) ;
#39053 = DIRECTION ( 'NONE',  ( -1.000000000000000000, -0.000000000000000000, 0.000000000000000000 ) ) ;
#39054 = CARTESIAN_POINT ( 'NONE',  ( 10.00000000000000000, 0.8261519478431083030, 77.49459641780886443 ) ) ;
#39055 = LINE ( 'NONE', #5771, #1894 ) ;
#39056 = ORIENTED_EDGE ( 'NONE', *, *, #26079, .F. ) ;
#39057 = CARTESIAN_POINT ( 'NONE',  ( -12.50000000000000000, -132.5000000000000000, 40.00000000000000000 ) ) ;
#39058 = PLANE ( 'NONE',  #14424 ) ;
#39059 = DIRECTION ( 'NONE',  ( 1.000000000000000000, 0.000000000000000000, -0.000000000000000000 ) ) ;
#39060 = CARTESIAN_POINT ( 'NONE',  ( 10.00000000000000000, -50.23322058963393033, 64.81221759200326460 ) ) ;
#39061 = EDGE_CURVE ( 'NONE', #23445, #45870, #41489, .T. ) ;
#39062 = VERTEX_POINT ( 'NONE', #12920 ) ;
#39063 = AXIS2_PLACEMENT_3D ( 'NONE', #48306, #10869, #25778 ) ;
#39064 = DIRECTION ( 'NONE',  ( 0.000000000000000000, -0.8526401643540860720, -0.5224985647159590130 ) ) ;
#39065 = EDGE_CURVE ( 'NONE', #41267, #34876, #18027, .T. ) ;
#39066 = DIRECTION ( 'NONE',  ( -1.000000000000000000, 0.000000000000000000, 0.000000000000000000 ) ) ;
#39067 = DIRECTION ( 'NONE',  ( -1.000000000000000000, -0.000000000000000000, -0.000000000000000000 ) ) ;
#39068 = EDGE_CURVE ( 'NONE', #43691, #34767, #40541, .T. ) ;
#39069 = PLANE ( 'NONE',  #41209 ) ;
#39070 = LINE ( 'NONE', #17922, #26407 ) ;
#39071 = CARTESIAN_POINT ( 'NONE',  ( 25.81725066941077529, -113.8380548628854854, -5.500000000000000000 ) ) ;
#39072 = CARTESIAN_POINT ( 'NONE',  ( 10.00000000000000000, 44.88180994100468268, -63.18004540532978552 ) ) ;
#39073 = VERTEX_POINT ( 'NONE', #32705 ) ;
#39074 = CARTESIAN_POINT ( 'NONE',  ( -16.06301359042743115, -102.7814171781257357, 5.500000000000000000 ) ) ;
#39075 = EDGE_LOOP ( 'NONE', ( #45661, #33170, #33432, #44317 ) ) ;
#39076 = ADVANCED_FACE ( 'NONE', ( #33196 ), #2404, .T. ) ;
#39077 = CARTESIAN_POINT ( 'NONE',  ( 10.00000000000000000, 0.000000000000000000, 0.000000000000000000 ) ) ;
#39078 = ADVANCED_FACE ( 'NONE', ( #29526 ), #3079, .T. ) ;
#39079 = EDGE_CURVE ( 'NONE', #7679, #38227, #6530, .T. ) ;
#39080 = ORIENTED_EDGE ( 'NONE', *, *, #39259, .T. ) ;
#39081 = VECTOR ( 'NONE', #33510, 1000.000000000000227 ) ;
#39082 = AXIS2_PLACEMENT_3D ( 'NONE', #7178, #29691, #29460 ) ;
#39083 = ORIENTED_EDGE ( 'NONE', *, *, #36476, .T. ) ;
#39084 = VECTOR ( 'NONE', #7354, 1000.000000000000000 ) ;
#39085 = FACE_OUTER_BOUND ( 'NONE', #36834, .T. ) ;
#39086 = ORIENTED_EDGE ( 'NONE', *, *, #16262, .F. ) ;
#39087 = VECTOR ( 'NONE', #7016, 1000.000000000000114 ) ;
#39088 = EDGE_LOOP ( 'NONE', ( #47724, #25342, #29986, #14955 ) ) ;
#39089 = AXIS2_PLACEMENT_3D ( 'NONE', #2488, #10082, #24534 ) ;
#39090 = CARTESIAN_POINT ( 'NONE',  ( -12.50000000000000000, -120.0000000000000000, -40.00000000000000711 ) ) ;
#39091 = DIRECTION ( 'NONE',  ( 0.000000000000000000, 0.000000000000000000, 1.000000000000000000 ) ) ;
#39092 = ORIENTED_EDGE ( 'NONE', *, *, #12606, .F. ) ;
#39093 = ORIENTED_EDGE ( 'NONE', *, *, #18240, .F. ) ;
#39094 = VERTEX_POINT ( 'NONE', #25357 ) ;
#39095 = DIRECTION ( 'NONE',  ( -1.000000000000000000, -0.000000000000000000, -0.000000000000000000 ) ) ;
#39097 = ORIENTED_EDGE ( 'NONE', *, *, #41350, .F. ) ;
#39096 = DIRECTION ( 'NONE',  ( -1.000000000000000000, -0.000000000000000000, 0.000000000000000000 ) ) ;
#39098 = CARTESIAN_POINT ( 'NONE',  ( 10.00000000000000000, 0.000000000000000000, 0.000000000000000000 ) ) ;
#39099 = ORIENTED_EDGE ( 'NONE', *, *, #6866, .T. ) ;
#39100 = VERTEX_POINT ( 'NONE', #17775 ) ;
#39101 = LINE ( 'NONE', #28090, #16144 ) ;
#39102 = ORIENTED_EDGE ( 'NONE', *, *, #15469, .T. ) ;
#39103 = ORIENTED_EDGE ( 'NONE', *, *, #13668, .T. ) ;
#39104 = DIRECTION ( 'NONE',  ( 0.000000000000000000, 0.9510565162951544194, -0.3090169943749447867 ) ) ;
#39105 = DIRECTION ( 'NONE',  ( 0.000000000000000000, 0.000000000000000000, 1.000000000000000000 ) ) ;
#39106 = ORIENTED_EDGE ( 'NONE', *, *, #6929, .T. ) ;
#39107 = FACE_OUTER_BOUND ( 'NONE', #230, .T. ) ;
#39108 = DIRECTION ( 'NONE',  ( -1.000000000000000000, -0.000000000000000000, 0.000000000000000000 ) ) ;
#39109 = DIRECTION ( 'NONE',  ( 0.000000000000000000, 0.9238795325112851842, 0.3826834323650938896 ) ) ;
#39110 = ORIENTED_EDGE ( 'NONE', *, *, #43649, .T. ) ;
#39111 = ORIENTED_EDGE ( 'NONE', *, *, #11412, .F. ) ;
#39112 = DIRECTION ( 'NONE',  ( -1.000000000000000000, 0.000000000000000000, 0.000000000000000000 ) ) ;
#39113 = AXIS2_PLACEMENT_3D ( 'NONE', #33431, #26086, #41034 ) ;
#39114 = CARTESIAN_POINT ( 'NONE',  ( 10.00000000000000000, 40.68715046381944234, -10.41901085202036192 ) ) ;
#39115 = EDGE_CURVE ( 'NONE', #7784, #24221, #36138, .T. ) ;
#39116 = ORIENTED_EDGE ( 'NONE', *, *, #40899, .F. ) ;
#39117 = AXIS2_PLACEMENT_3D ( 'NONE', #28192, #43609, #43131 ) ;
#39118 = CARTESIAN_POINT ( 'NONE',  ( 10.00000000000000000, -36.88895765772628010, -6.736453364083947015 ) ) ;
#39119 = ORIENTED_EDGE ( 'NONE', *, *, #36720, .T. ) ;
#39120 = CIRCLE ( 'NONE', #17221, 16.00000000000000000 ) ;
#39121 = EDGE_CURVE ( 'NONE', #9352, #16510, #36024, .T. ) ;
#39122 = DIRECTION ( 'NONE',  ( -1.000000000000000000, -0.000000000000000000, 0.000000000000000000 ) ) ;
#39123 = DIRECTION ( 'NONE',  ( 0.000000000000000000, -6.982962677686266711E-15, 1.000000000000000000 ) ) ;
#39124 = CARTESIAN_POINT ( 'NONE',  ( 16.30584220631899228, -140.9432449716519784, -5.500000000000000000 ) ) ;
#39125 = CARTESIAN_POINT ( 'NONE',  ( 24.95699195200416654, -110.9640411295978595, 2.500000000000000000 ) ) ;
#39126 = EDGE_CURVE ( 'NONE', #40831, #38630, #3322, .T. ) ;
#39127 = AXIS2_PLACEMENT_3D ( 'NONE', #33056, #48235, #43836 ) ;
#39128 = DIRECTION ( 'NONE',  ( 0.000000000000000000, 0.000000000000000000, -1.000000000000000000 ) ) ;
#39129 = DIRECTION ( 'NONE',  ( -1.000000000000000000, 0.000000000000000000, 0.000000000000000000 ) ) ;
#39130 = VERTEX_POINT ( 'NONE', #44218 ) ;
#39131 = CYLINDRICAL_SURFACE ( 'NONE', #38805, 1.000000000000000000 ) ;
#39132 = CIRCLE ( 'NONE', #14882, 31.99999999999998934 ) ;
#39133 = CARTESIAN_POINT ( 'NONE',  ( 10.00000000000000000, -16.23288003029473359, -33.80338159004301701 ) ) ;
#39134 = DIRECTION ( 'NONE',  ( 0.000000000000000000, 0.3090169943749560555, 0.9510565162951506446 ) ) ;
#39135 = CYLINDRICAL_SURFACE ( 'NONE', #36263, 82.00000000000000000 ) ;
#39136 = ORIENTED_EDGE ( 'NONE', *, *, #2230, .F. ) ;
#39137 = ADVANCED_FACE ( 'NONE', ( #10694 ), #25600, .F. ) ;
#39138 = EDGE_CURVE ( 'NONE', #13341, #28312, #34438, .T. ) ;
#39139 = ORIENTED_EDGE ( 'NONE', *, *, #25294, .T. ) ;
#39140 = ORIENTED_EDGE ( 'NONE', *, *, #22224, .F. ) ;
#39141 = ORIENTED_EDGE ( 'NONE', *, *, #45479, .T. ) ;
#39142 = DIRECTION ( 'NONE',  ( -1.000000000000000000, -0.000000000000000000, 0.000000000000000000 ) ) ;
#39143 = PLANE ( 'NONE',  #37021 ) ;
#39144 = ORIENTED_EDGE ( 'NONE', *, *, #21905, .F. ) ;
#39145 = EDGE_CURVE ( 'NONE', #18977, #29688, #6340, .T. ) ;
#39146 = VECTOR ( 'NONE', #31680, 1000.000000000000000 ) ;
#39147 = VECTOR ( 'NONE', #39096, 1000.000000000000000 ) ;
#39148 = DIRECTION ( 'NONE',  ( 0.000000000000000000, 0.3090169943749442316, 0.9510565162951545304 ) ) ;
#39149 = CIRCLE ( 'NONE', #3175, 31.99999999999998579 ) ;
#39150 = CIRCLE ( 'NONE', #19595, 32.00000000000000000 ) ;
#39151 = ORIENTED_EDGE ( 'NONE', *, *, #13915, .T. ) ;
#39152 = VERTEX_POINT ( 'NONE', #22178 ) ;
#39153 = ORIENTED_EDGE ( 'NONE', *, *, #30908, .T. ) ;
#39154 = ORIENTED_EDGE ( 'NONE', *, *, #3255, .F. ) ;
#39155 = CARTESIAN_POINT ( 'NONE',  ( 10.00000000000000000, 0.000000000000000000, 0.000000000000000000 ) ) ;
#39156 = ORIENTED_EDGE ( 'NONE', *, *, #26011, .T. ) ;
#39157 = CARTESIAN_POINT ( 'NONE',  ( -32.50000000000000000, -120.0000000000000000, -2.500000000000000000 ) ) ;
#39158 = VERTEX_POINT ( 'NONE', #36853 ) ;
#39159 = APPLICATION_CONTEXT ( 'automotive_design' ) ;
#39160 = DIRECTION ( 'NONE',  ( -1.000000000000000000, 0.000000000000000000, -0.000000000000000000 ) ) ;
#39161 = FACE_OUTER_BOUND ( 'NONE', #14486, .T. ) ;
#39162 = DIRECTION ( 'NONE',  ( 0.000000000000000000, 0.000000000000000000, 1.000000000000000000 ) ) ;
#39163 = EDGE_LOOP ( 'NONE', ( #32872, #12487, #32774, #5954 ) ) ;
#39164 = DIRECTION ( 'NONE',  ( 1.000000000000000000, 0.000000000000000000, 0.000000000000000000 ) ) ;
#39165 = EDGE_LOOP ( 'NONE', ( #31808, #18082, #9405, #2343 ) ) ;
#39166 = CARTESIAN_POINT ( 'NONE',  ( 0.000000000000000000, -32.34446384429951138, -26.79245525562750530 ) ) ;
#39167 = FACE_OUTER_BOUND ( 'NONE', #2854, .T. ) ;
#39168 = CYLINDRICAL_SURFACE ( 'NONE', #24854, 32.00000000000000000 ) ;
#39169 = ORIENTED_EDGE ( 'NONE', *, *, #2220, .F. ) ;
#39170 = ORIENTED_EDGE ( 'NONE', *, *, #47668, .F. ) ;
#39171 = CARTESIAN_POINT ( 'NONE',  ( 15.00000000000000000, -18.13022148937263012, -15.02647892043543898 ) ) ;
#39172 = DIRECTION ( 'NONE',  ( -1.000000000000000000, -0.000000000000000000, -0.000000000000000000 ) ) ;
#39173 = ORIENTED_EDGE ( 'NONE', *, *, #32184, .F. ) ;
#39174 = EDGE_CURVE ( 'NONE', #48128, #33667, #14611, .T. ) ;
#39175 = CARTESIAN_POINT ( 'NONE',  ( 11.99999999999999822, -34.44570377933647620, 69.42325613327427902 ) ) ;
#39176 = CARTESIAN_POINT ( 'NONE',  ( 0.000000000000000000, -31.47745569255189224, 68.26794271651249346 ) ) ;
#39177 = CARTESIAN_POINT ( 'NONE',  ( 0.000000000000000000, 55.38113227695858143, -54.21277698773617715 ) ) ;
#39178 = DIRECTION ( 'NONE',  ( -1.000000000000000000, 0.000000000000000000, -0.000000000000000000 ) ) ;
#39179 = ADVANCED_FACE ( 'NONE', ( #6774 ), #40779, .T. ) ;
#39180 = CARTESIAN_POINT ( 'NONE',  ( 0.000000000000000000, 2.956366410621684260, -75.11725578898465017 ) ) ;
#39182 = VECTOR ( 'NONE', #11321, 1000.000000000000000 ) ;
#39181 = DIRECTION ( 'NONE',  ( -1.000000000000000000, -0.000000000000000000, 0.000000000000000000 ) ) ;
#39183 = ORIENTED_EDGE ( 'NONE', *, *, #32927, .T. ) ;
#39184 = VECTOR ( 'NONE', #35356, 1000.000000000000000 ) ;
#39185 = FACE_OUTER_BOUND ( 'NONE', #3031, .T. ) ;
#39186 = EDGE_CURVE ( 'NONE', #21863, #40723, #43821, .T. ) ;
#39187 = DIRECTION ( 'NONE',  ( 0.000000000000000000, -0.6494480483301903195, 0.7604059656000252687 ) ) ;
#39188 = CARTESIAN_POINT ( 'NONE',  ( 0.000000000000000000, -0.9646360437372163421, -23.52805723605591126 ) ) ;
#39189 = CIRCLE ( 'NONE', #34482, 82.00000000000000000 ) ;
#39190 = AXIS2_PLACEMENT_3D ( 'NONE', #14115, #47632, #20741 ) ;
#39191 = CARTESIAN_POINT ( 'NONE',  ( 0.000000000000000000, 59.46389618802034960, -49.70050353004825894 ) ) ;
#39192 = PLANE ( 'NONE',  #44919 ) ;
#39193 = CARTESIAN_POINT ( 'NONE',  ( 0.000000000000000000, 27.74655509720780344, -77.16300072079631889 ) ) ;
#39194 = CARTESIAN_POINT ( 'NONE',  ( 15.00000000000000000, -18.13022148937242761, 15.02647892043569122 ) ) ;
#39195 = CARTESIAN_POINT ( 'NONE',  ( 0.000000000000000000, 14.60985201121704513, 18.46759930825707841 ) ) ;
#39196 = VECTOR ( 'NONE', #19049, 1000.000000000000000 ) ;
#39197 = ORIENTED_EDGE ( 'NONE', *, *, #32868, .T. ) ;
#39198 = EDGE_CURVE ( 'NONE', #13864, #24652, #16506, .T. ) ;
#39199 = AXIS2_PLACEMENT_3D ( 'NONE', #48433, #41355, #33992 ) ;
#39200 = ORIENTED_EDGE ( 'NONE', *, *, #46361, .T. ) ;
#39201 = DIRECTION ( 'NONE',  ( -1.000000000000000000, -0.000000000000000000, -0.000000000000000000 ) ) ;
#39202 = EDGE_CURVE ( 'NONE', #39316, #2713, #9959, .T. ) ;
#39203 = DIRECTION ( 'NONE',  ( 0.000000000000000000, 0.9969173337331281859, -0.07845909572784168229 ) ) ;
#39204 = CIRCLE ( 'NONE', #29057, 37.49900000000000233 ) ;
#39205 = ITEM_DEFINED_TRANSFORMATION ( 'NONE', 'NONE', #36601,  #11636 ) ;
#39206 = CARTESIAN_POINT ( 'NONE',  ( 11.99999999999999822, 0.000000000000000000, 0.000000000000000000 ) ) ;
#39207 = ORIENTED_EDGE ( 'NONE', *, *, #35646, .F. ) ;
#39208 = EDGE_CURVE ( 'NONE', #4907, #1534, #21199, .T. ) ;
#39209 = CARTESIAN_POINT ( 'NONE',  ( -10.00000000000000000, 0.000000000000000000, 0.000000000000000000 ) ) ;
#39210 = ORIENTED_EDGE ( 'NONE', *, *, #39391, .T. ) ;
#39211 = DIRECTION ( 'NONE',  ( -1.000000000000000000, -0.000000000000000000, -0.000000000000000000 ) ) ;
#39212 = ORIENTED_EDGE ( 'NONE', *, *, #33368, .F. ) ;
#39213 = DIRECTION ( 'NONE',  ( -1.000000000000000000, 0.000000000000000000, 0.000000000000000000 ) ) ;
#39214 = DIRECTION ( 'NONE',  ( 0.000000000000000000, -0.5877852522924802425, 0.8090169943749422332 ) ) ;
#39215 = CARTESIAN_POINT ( 'NONE',  ( -3.000000000000000000, -14.54903810567645195, -22.19967320028775504 ) ) ;
#39216 = ORIENTED_EDGE ( 'NONE', *, *, #46858, .T. ) ;
#39217 = CARTESIAN_POINT ( 'NONE',  ( 0.000000000000000000, -30.41916302227061664, -71.27951684758058093 ) ) ;
#39218 = AXIS2_PLACEMENT_3D ( 'NONE', #979, #30610, #15929 ) ;
#39219 = ORIENTED_EDGE ( 'NONE', *, *, #34986, .F. ) ;
#39220 = VECTOR ( 'NONE', #3039, 1000.000000000000000 ) ;
#39221 = CARTESIAN_POINT ( 'NONE',  ( 0.000000000000000000, -72.35160999960831418, 20.41045688087797672 ) ) ;
#39222 = CIRCLE ( 'NONE', #43139, 16.00000000000000000 ) ;
#39223 = CARTESIAN_POINT ( 'NONE',  ( 10.00000000000000000, -11.30684508768284680, -76.66974797899850103 ) ) ;
#39224 = DIRECTION ( 'NONE',  ( -0.000000000000000000, 0.3090169943749573878, 0.9510565162951503115 ) ) ;
#39226 = ORIENTED_EDGE ( 'NONE', *, *, #45630, .T. ) ;
#39225 = FACE_OUTER_BOUND ( 'NONE', #9990, .T. ) ;
#39227 = VERTEX_POINT ( 'NONE', #30487 ) ;
#39228 = DIRECTION ( 'NONE',  ( -1.000000000000000000, 0.000000000000000000, 0.000000000000000000 ) ) ;
#39229 = ORIENTED_EDGE ( 'NONE', *, *, #6098, .T. ) ;
#39230 = EDGE_CURVE ( 'NONE', #13774, #7495, #14842, .T. ) ;
#39231 = DIRECTION ( 'NONE',  ( 0.000000000000000000, 0.000000000000000000, 1.000000000000000000 ) ) ;
#39232 = VERTEX_POINT ( 'NONE', #26576 ) ;
#39233 = EDGE_CURVE ( 'NONE', #19393, #25961, #23378, .T. ) ;
#39234 = DIRECTION ( 'NONE',  ( 0.000000000000000000, 0.000000000000000000, 1.000000000000000000 ) ) ;
#39235 = DIRECTION ( 'NONE',  ( -1.000000000000000000, 0.000000000000000000, 0.000000000000000000 ) ) ;
#39236 = DIRECTION ( 'NONE',  ( 0.000000000000000000, -0.3090169943749349057, -0.9510565162951577500 ) ) ;
#39237 = ORIENTED_EDGE ( 'NONE', *, *, #20974, .F. ) ;
#39238 = LINE ( 'NONE', #20628, #13605 ) ;
#39239 = CARTESIAN_POINT ( 'NONE',  ( 11.99999999999999822, 12.93880638057315657, 76.41127070299278046 ) ) ;
#39240 = ADVANCED_FACE ( 'NONE', ( #38315 ), #4314, .F. ) ;
#39241 = CARTESIAN_POINT ( 'NONE',  ( 0.000000000000000000, 0.000000000000000000, 0.000000000000000000 ) ) ;
#39242 = DIRECTION ( 'NONE',  ( -1.000000000000000000, -2.889240119132116694E-16, 0.000000000000000000 ) ) ;
#39243 = DIRECTION ( 'NONE',  ( 0.000000000000000000, -8.881784197001252323E-16, 1.000000000000000000 ) ) ;
#39244 = DIRECTION ( 'NONE',  ( 0.000000000000000000, -0.2334453638559126354, 0.9723699203976748917 ) ) ;
#39246 = EDGE_CURVE ( 'NONE', #42000, #34549, #33715, .T. ) ;
#39245 = CARTESIAN_POINT ( 'NONE',  ( -43.60332556124591008, -133.0000000000000000, 102.9091629284897493 ) ) ;
#39247 = CARTESIAN_POINT ( 'NONE',  ( 5.000000000000000000, 60.67117009219135326, 55.16347631943062169 ) ) ;
#39248 = FACE_OUTER_BOUND ( 'NONE', #44763, .T. ) ;
#39249 = LINE ( 'NONE', #35817, #25299 ) ;
#39250 = ORIENTED_EDGE ( 'NONE', *, *, #11543, .T. ) ;
#39251 = AXIS2_PLACEMENT_3D ( 'NONE', #25319, #6739, #18218 ) ;
#39252 = DIRECTION ( 'NONE',  ( 0.000000000000000000, -1.000000000000000000, 0.000000000000000000 ) ) ;
#39253 = VERTEX_POINT ( 'NONE', #11646 ) ;
#39254 = DIRECTION ( 'NONE',  ( 0.000000000000000000, 0.7071067811865436870, 0.7071067811865512365 ) ) ;
#39255 = VECTOR ( 'NONE', #12266, 1000.000000000000000 ) ;
#39256 = CYLINDRICAL_SURFACE ( 'NONE', #43216, 11.59999999999999787 ) ;
#39257 = CIRCLE ( 'NONE', #8738, 16.00000000000000000 ) ;
#39258 = ORIENTED_EDGE ( 'NONE', *, *, #28519, .T. ) ;
#39259 = EDGE_CURVE ( 'NONE', #34495, #30209, #30581, .T. ) ;
#39260 = DIRECTION ( 'NONE',  ( -1.000000000000000000, 0.000000000000000000, 0.000000000000000000 ) ) ;
#39261 = ORIENTED_EDGE ( 'NONE', *, *, #36779, .T. ) ;
#39262 = EDGE_CURVE ( 'NONE', #25211, #40387, #627, .T. ) ;
#39263 = ORIENTED_EDGE ( 'NONE', *, *, #14765, .F. ) ;
#39264 = CIRCLE ( 'NONE', #43181, 31.99999999999998224 ) ;
#39265 = ADVANCED_FACE ( 'NONE', ( #45660 ), #23144, .T. ) ;
#39266 = DIRECTION ( 'NONE',  ( -1.000000000000000000, -0.000000000000000000, 0.000000000000000000 ) ) ;
#39267 = CARTESIAN_POINT ( 'NONE',  ( 12.00000000000000000, -1.278221433540145391, 26.51162292216073979 ) ) ;
#39268 = DIRECTION ( 'NONE',  ( -1.000000000000000000, 0.000000000000000000, 0.000000000000000000 ) ) ;
#39269 = AXIS2_PLACEMENT_3D ( 'NONE', #42072, #33988, #38395 ) ;
#39270 = ORIENTED_EDGE ( 'NONE', *, *, #2694, .F. ) ;
#39271 = PLANE ( 'NONE',  #32130 ) ;
#39272 = ORIENTED_EDGE ( 'NONE', *, *, #31512, .T. ) ;
#39273 = CARTESIAN_POINT ( 'NONE',  ( 0.000000000000000000, 50.95692526931414790, -58.39081064771693974 ) ) ;
#39274 = DIRECTION ( 'NONE',  ( 0.4279312458753000703, 0.9038112904824842087, -0.000000000000000000 ) ) ;
#39275 = CYLINDRICAL_SURFACE ( 'NONE', #31404, 77.49899999999999523 ) ;
#39276 = CIRCLE ( 'NONE', #19726, 15.99999999999999822 ) ;
#39277 = AXIS2_PLACEMENT_3D ( 'NONE', #18863, #10320, #47754 ) ;
#39278 = VERTEX_POINT ( 'NONE', #12150 ) ;
#39279 = EDGE_LOOP ( 'NONE', ( #37324, #10851, #9848, #44727 ) ) ;
#39280 = DIRECTION ( 'NONE',  ( -1.000000000000000000, 0.000000000000000000, -0.000000000000000000 ) ) ;
#39281 = VERTEX_POINT ( 'NONE', #34155 ) ;
#39282 = EDGE_CURVE ( 'NONE', #352, #5583, #36062, .T. ) ;
#39283 = CIRCLE ( 'NONE', #18164, 42.00000000000000000 ) ;
#39284 = DIRECTION ( 'NONE',  ( 0.000000000000000000, 0.6494480483301793283, 0.7604059656000345946 ) ) ;
#39285 = CARTESIAN_POINT ( 'NONE',  ( 0.000000000000000000, -8.830959090341869100, -74.65491531819127147 ) ) ;
#39286 = DIRECTION ( 'NONE',  ( 0.000000000000000000, 0.5877852522924685852, 0.8090169943749508930 ) ) ;
#39287 = CARTESIAN_POINT ( 'NONE',  ( 11.99999999999999822, -11.30684508768284680, -76.66974797899850103 ) ) ;
#39288 = ADVANCED_FACE ( 'NONE', ( #15801 ), #130, .T. ) ;
#39289 = CARTESIAN_POINT ( 'NONE',  ( 10.00000000000000000, -65.64334221924882229, -41.19522573413803457 ) ) ;
#39290 = CIRCLE ( 'NONE', #15051, 15.99999999999999645 ) ;
#39291 = DIRECTION ( 'NONE',  ( -1.000000000000000000, 0.000000000000000000, 0.000000000000000000 ) ) ;
#39292 = DIRECTION ( 'NONE',  ( 0.000000000000000000, 0.000000000000000000, 1.000000000000000000 ) ) ;
#39293 = CARTESIAN_POINT ( 'NONE',  ( 10.00000000000000000, 0.000000000000000000, 0.000000000000000000 ) ) ;
#39294 = LINE ( 'NONE', #9425, #25934 ) ;
#39295 = DIRECTION ( 'NONE',  ( -1.000000000000000000, 0.000000000000000000, 0.000000000000000000 ) ) ;
#39296 = VERTEX_POINT ( 'NONE', #44685 ) ;
#39297 = AXIS2_PLACEMENT_3D ( 'NONE', #46162, #20204, #12627 ) ;
#39298 = EDGE_LOOP ( 'NONE', ( #6231, #27815, #26289, #10032 ) ) ;
#39300 = EDGE_CURVE ( 'NONE', #11173, #21975, #44940, .T. ) ;
#39299 = DIRECTION ( 'NONE',  ( -1.000000000000000000, -0.000000000000000000, 0.000000000000000000 ) ) ;
#39301 = AXIS2_PLACEMENT_3D ( 'NONE', #12359, #8193, #16028 ) ;
#39302 = EDGE_CURVE ( 'NONE', #18, #22172, #8452, .T. ) ;
#39303 = CYLINDRICAL_SURFACE ( 'NONE', #37640, 77.49899999999999523 ) ;
#39304 = LINE ( 'NONE', #32451, #18242 ) ;
#39305 = CARTESIAN_POINT ( 'NONE',  ( 4.999999999999999112, -10.41901085202050581, -40.68715046381939970 ) ) ;
#39306 = CARTESIAN_POINT ( 'NONE',  ( 10.00000000000000000, -66.50666863322028632, 39.78640506895582973 ) ) ;
#39307 = DIRECTION ( 'NONE',  ( -1.000000000000000000, -0.000000000000000000, 0.000000000000000000 ) ) ;
#39308 = DIRECTION ( 'NONE',  ( 0.000000000000000000, -0.8090169943749531134, 0.5877852522924653655 ) ) ;
#39309 = ORIENTED_EDGE ( 'NONE', *, *, #30786, .T. ) ;
#39310 = DIRECTION ( 'NONE',  ( 0.000000000000000000, -0.5877852522924625900, -0.8090169943749551118 ) ) ;
#39311 = VERTEX_POINT ( 'NONE', #8213 ) ;
#39312 = AXIS2_PLACEMENT_3D ( 'NONE', #32161, #13551, #47080 ) ;
#39313 = CARTESIAN_POINT ( 'NONE',  ( 0.000000000000000000, 0.000000000000000000, 0.000000000000000000 ) ) ;
#39314 = CYLINDRICAL_SURFACE ( 'NONE', #47088, 82.00000000000000000 ) ;
#39315 = EDGE_LOOP ( 'NONE', ( #12588, #7358, #46080, #6781 ) ) ;
#39316 = VERTEX_POINT ( 'NONE', #19449 ) ;
#39317 = EDGE_CURVE ( 'NONE', #27585, #2609, #18733, .T. ) ;
#39318 = VERTEX_POINT ( 'NONE', #19688 ) ;
#39319 = VECTOR ( 'NONE', #30623, 1000.000000000000000 ) ;
#39320 = AXIS2_PLACEMENT_3D ( 'NONE', #12162, #35371, #23629 ) ;
#39321 = AXIS2_PLACEMENT_3D ( 'NONE', #5222, #38757, #12555 ) ;
#39322 = CIRCLE ( 'NONE', #3316, 31.99999999999999289 ) ;
#39323 = CARTESIAN_POINT ( 'NONE',  ( 0.000000000000000000, -18.89407956138310496, 75.16055320797023853 ) ) ;
#39324 = ORIENTED_EDGE ( 'NONE', *, *, #38666, .T. ) ;
#39325 = CIRCLE ( 'NONE', #13543, 37.49900000000000944 ) ;
#39326 = ORIENTED_EDGE ( 'NONE', *, *, #34640, .F. ) ;
#39327 = VECTOR ( 'NONE', #24794, 999.9999999999998863 ) ;
#39328 = DIRECTION ( 'NONE',  ( -0.000000000000000000, -0.000000000000000000, -1.000000000000000000 ) ) ;
#39329 = CIRCLE ( 'NONE', #29969, 82.00000000000000000 ) ;
#39331 = ORIENTED_EDGE ( 'NONE', *, *, #40417, .T. ) ;
#39330 = DIRECTION ( 'NONE',  ( -1.000000000000000000, 0.000000000000000000, 0.000000000000000000 ) ) ;
#39332 = ADVANCED_FACE ( 'NONE', ( #855 ), #11167, .T. ) ;
#39333 = ORIENTED_EDGE ( 'NONE', *, *, #44203, .T. ) ;
#39334 = EDGE_LOOP ( 'NONE', ( #21322, #40070, #39183, #5671 ) ) ;
#39335 = DIRECTION ( 'NONE',  ( 0.000000000000000000, -0.7071067811865389130, -0.7071067811865562325 ) ) ;
#39337 = VERTEX_POINT ( 'NONE', #7500 ) ;
#39336 = FACE_OUTER_BOUND ( 'NONE', #33314, .T. ) ;
#39338 = LINE ( 'NONE', #24653, #3213 ) ;
#39339 = ORIENTED_EDGE ( 'NONE', *, *, #9558, .T. ) ;
#39340 = VERTEX_POINT ( 'NONE', #22428 ) ;
#39341 = FACE_OUTER_BOUND ( 'NONE', #28805, .T. ) ;
#39342 = ORIENTED_EDGE ( 'NONE', *, *, #28471, .F. ) ;
#39343 = CARTESIAN_POINT ( 'NONE',  ( -23.30023580412278505, -123.4057321492263384, 5.500000000000000000 ) ) ;
#39344 = CARTESIAN_POINT ( 'NONE',  ( 11.99999999999999822, 0.000000000000000000, 0.000000000000000000 ) ) ;
#39345 = CARTESIAN_POINT ( 'NONE',  ( 0.000000000000000000, 27.75498641678786527, -31.52238457039571173 ) ) ;
#39346 = CARTESIAN_POINT ( 'NONE',  ( 10.00000000000000000, 62.20884554314020676, 46.21855187248652896 ) ) ;
#39347 = AXIS2_PLACEMENT_3D ( 'NONE', #39450, #6870, #13488 ) ;
#39348 = EDGE_CURVE ( 'NONE', #390, #37389, #19622, .T. ) ;
#39349 = CARTESIAN_POINT ( 'NONE',  ( 0.000000000000000000, -37.48860685352291711, 0.8828120875899322373 ) ) ;
#39350 = VERTEX_POINT ( 'NONE', #26340 ) ;
#39351 = EDGE_CURVE ( 'NONE', #40885, #16815, #41273, .T. ) ;
#39352 = EDGE_CURVE ( 'NONE', #23846, #40712, #24114, .T. ) ;
#39353 = EDGE_LOOP ( 'NONE', ( #18506, #36241, #27835, #31363 ) ) ;
#39354 = AXIS2_PLACEMENT_3D ( 'NONE', #21776, #36702, #40624 ) ;
#39355 = CARTESIAN_POINT ( 'NONE',  ( 10.00000000000000000, -50.95692526931286181, -58.39081064771806240 ) ) ;
#39356 = CARTESIAN_POINT ( 'NONE',  ( 0.000000000000000000, 0.000000000000000000, 0.000000000000000000 ) ) ;
#39357 = VERTEX_POINT ( 'NONE', #38818 ) ;
#39359 = ADVANCED_FACE ( 'NONE', ( #5755 ), #16773, .T. ) ;
#39358 = DIRECTION ( 'NONE',  ( -1.000000000000000000, -0.000000000000000000, 0.000000000000000000 ) ) ;
#39360 = ORIENTED_EDGE ( 'NONE', *, *, #43298, .T. ) ;
#39361 = AXIS2_PLACEMENT_3D ( 'NONE', #39785, #21160, #2554 ) ;
#39362 = VECTOR ( 'NONE', #13646, 1000.000000000000000 ) ;
#39363 = AXIS2_PLACEMENT_3D ( 'NONE', #37146, #14643, #33468 ) ;
#39364 = DIRECTION ( 'NONE',  ( 0.000000000000000000, 0.000000000000000000, 1.000000000000000000 ) ) ;
#39365 = CIRCLE ( 'NONE', #5749, 42.00000000000000000 ) ;
#39366 = DIRECTION ( 'NONE',  ( 0.3311129884571281101, 0.9435911131814402886, 0.000000000000000000 ) ) ;
#39367 = CARTESIAN_POINT ( 'NONE',  ( 10.00000000000000000, -30.00120703465222149, 22.64427369931158296 ) ) ;
#39368 = ADVANCED_FACE ( 'NONE', ( #46383 ), #42959, .T. ) ;
#39369 = CARTESIAN_POINT ( 'NONE',  ( 10.00000000000000000, 68.55367621811141987, 44.99326035066078333 ) ) ;
#39370 = VECTOR ( 'NONE', #23402, 1000.000000000000000 ) ;
#39371 = FILL_AREA_STYLE_COLOUR ( '', #35281 ) ;
#39372 = CARTESIAN_POINT ( 'NONE',  ( -3.000000000000000000, -0.9646360437375307573, 23.52805723605590060 ) ) ;
#39373 = VERTEX_POINT ( 'NONE', #1598 ) ;
#39374 = VECTOR ( 'NONE', #35775, 1000.000000000000114 ) ;
#39375 = CIRCLE ( 'NONE', #1064, 77.49900000000000944 ) ;
#39376 = CARTESIAN_POINT ( 'NONE',  ( 0.000000000000000000, 0.000000000000000000, 0.000000000000000000 ) ) ;
#39377 = FACE_OUTER_BOUND ( 'NONE', #12747, .T. ) ;
#39378 = DIRECTION ( 'NONE',  ( -1.000000000000000000, 0.000000000000000000, 0.000000000000000000 ) ) ;
#39379 = AXIS2_PLACEMENT_3D ( 'NONE', #36220, #21281, #43576 ) ;
#39380 = CIRCLE ( 'NONE', #37798, 37.49900000000001654 ) ;
#39381 = DIRECTION ( 'NONE',  ( 0.000000000000000000, 0.000000000000000000, 1.000000000000000000 ) ) ;
#39382 = FILL_AREA_STYLE ('',( #1694 ) ) ;
#39383 = CIRCLE ( 'NONE', #5770, 77.49899999999998101 ) ;
#39384 = ORIENTED_EDGE ( 'NONE', *, *, #3755, .F. ) ;
#39385 = ORIENTED_EDGE ( 'NONE', *, *, #27575, .F. ) ;
#39386 = LINE ( 'NONE', #1462, #38986 ) ;
#39387 = DIRECTION ( 'NONE',  ( -1.000000000000000000, -0.000000000000000000, 0.000000000000000000 ) ) ;
#39388 = VERTEX_POINT ( 'NONE', #23870 ) ;
#39389 = AXIS2_PLACEMENT_3D ( 'NONE', #45894, #23847, #12358 ) ;
#39390 = CIRCLE ( 'NONE', #3418, 77.49900000000000944 ) ;
#39391 = EDGE_CURVE ( 'NONE', #14588, #20955, #43096, .T. ) ;
#39392 = DIRECTION ( 'NONE',  ( -1.000000000000000000, 0.000000000000000000, -0.000000000000000000 ) ) ;
#39393 = AXIS2_PLACEMENT_3D ( 'NONE', #10934, #21468, #7255 ) ;
#39394 = FACE_OUTER_BOUND ( 'NONE', #3720, .T. ) ;
#39395 = AXIS2_PLACEMENT_3D ( 'NONE', #3290, #47838, #6499 ) ;
#39396 = EDGE_CURVE ( 'NONE', #18013, #25055, #17000, .T. ) ;
#39397 = ORIENTED_EDGE ( 'NONE', *, *, #30412, .F. ) ;
#39398 = VERTEX_POINT ( 'NONE', #28261 ) ;
#39399 = VERTEX_POINT ( 'NONE', #9649 ) ;
#39400 = EDGE_CURVE ( 'NONE', #42640, #45331, #4037, .T. ) ;
#39401 = CARTESIAN_POINT ( 'NONE',  ( -7.469491406282116053, 4.756046723998915482, -45.00000000000000000 ) ) ;
#39402 = EDGE_LOOP ( 'NONE', ( #3314, #27462, #39156, #48087 ) ) ;
#39403 = VECTOR ( 'NONE', #29069, 999.9999999999998863 ) ;
#39404 = AXIS2_PLACEMENT_3D ( 'NONE', #289, #23527, #15476 ) ;
#39405 = VERTEX_POINT ( 'NONE', #6009 ) ;
#39406 = CYLINDRICAL_SURFACE ( 'NONE', #3576, 82.00000000000000000 ) ;
#39407 = ORIENTED_EDGE ( 'NONE', *, *, #28339, .T. ) ;
#39408 = DIRECTION ( 'NONE',  ( 0.7273375899149812085, -0.6862798483830533369, 0.000000000000000000 ) ) ;
#39409 = AXIS2_PLACEMENT_3D ( 'NONE', #14214, #29617, #32344 ) ;
#39410 = AXIS2_PLACEMENT_3D ( 'NONE', #20436, #13113, #43206 ) ;
#39411 = LINE ( 'NONE', #28143, #27785 ) ;
#39412 = LINE ( 'NONE', #20301, #47830 ) ;
#39414 = ORIENTED_EDGE ( 'NONE', *, *, #39740, .T. ) ;
#39413 = VECTOR ( 'NONE', #44867, 1000.000000000000000 ) ;
#39415 = EDGE_CURVE ( 'NONE', #33470, #44331, #45433, .T. ) ;
#39416 = DIRECTION ( 'NONE',  ( -1.000000000000000000, -0.000000000000000000, -0.000000000000000000 ) ) ;
#39417 = EDGE_CURVE ( 'NONE', #28664, #47099, #21971, .T. ) ;
#39418 = ORIENTED_EDGE ( 'NONE', *, *, #11337, .F. ) ;
#39419 = DIRECTION ( 'NONE',  ( -1.000000000000000000, -0.000000000000000000, 0.000000000000000000 ) ) ;
#39420 = LINE ( 'NONE', #46996, #25864 ) ;
#39421 = DIRECTION ( 'NONE',  ( -1.000000000000000000, 0.000000000000000000, 0.000000000000000000 ) ) ;
#39422 = ORIENTED_EDGE ( 'NONE', *, *, #41984, .F. ) ;
#39423 = ORIENTED_EDGE ( 'NONE', *, *, #39068, .F. ) ;
#39424 = DIRECTION ( 'NONE',  ( 0.000000000000000000, 0.000000000000000000, 1.000000000000000000 ) ) ;
#39425 = DIRECTION ( 'NONE',  ( 0.000000000000000000, 0.000000000000000000, 1.000000000000000000 ) ) ;
#39426 = ORIENTED_EDGE ( 'NONE', *, *, #5687, .F. ) ;
#39427 = DIRECTION ( 'NONE',  ( -1.000000000000000000, 0.000000000000000000, 0.000000000000000000 ) ) ;
#39428 = CARTESIAN_POINT ( 'NONE',  ( -11.59999999999999964, -0.8299999999999986278, 0.000000000000000000 ) ) ;
#39429 = FACE_OUTER_BOUND ( 'NONE', #18968, .T. ) ;
#39430 = CARTESIAN_POINT ( 'NONE',  ( 15.00000000000000000, -22.32062822937469093, 14.36278369418830181 ) ) ;
#39431 = EDGE_CURVE ( 'NONE', #36936, #3893, #45912, .T. ) ;
#39432 = DIRECTION ( 'NONE',  ( -1.000000000000000000, 0.000000000000000000, 0.000000000000000000 ) ) ;
#39433 = AXIS2_PLACEMENT_3D ( 'NONE', #7575, #4145, #11972 ) ;
#39434 = DIRECTION ( 'NONE',  ( -1.000000000000000000, -0.000000000000000000, -0.000000000000000000 ) ) ;
#39435 = LINE ( 'NONE', #20101, #3628 ) ;
#39436 = CIRCLE ( 'NONE', #12050, 82.00000000000000000 ) ;
#39437 = AXIS2_PLACEMENT_3D ( 'NONE', #36540, #28724, #43650 ) ;
#39438 = CARTESIAN_POINT ( 'NONE',  ( 11.99999999999999822, -59.75363087400113926, 56.15606465354937171 ) ) ;
#39440 = AXIS2_PLACEMENT_3D ( 'NONE', #14233, #39948, #29153 ) ;
#39439 = DIRECTION ( 'NONE',  ( -1.000000000000000000, -0.000000000000000000, 0.000000000000000000 ) ) ;
#39441 = CARTESIAN_POINT ( 'NONE',  ( 12.00000000000000000, -10.45096189432344502, -21.10159698893425784 ) ) ;
#39442 = DIRECTION ( 'NONE',  ( 0.000000000000000000, 0.000000000000000000, 1.000000000000000000 ) ) ;
#39443 = CARTESIAN_POINT ( 'NONE',  ( 0.000000000000000000, -2.946379043145784582, -75.11764819372150725 ) ) ;
#39444 = EDGE_LOOP ( 'NONE', ( #744, #14492, #1892, #29443 ) ) ;
#39445 = ORIENTED_EDGE ( 'NONE', *, *, #5310, .F. ) ;
#39447 = FACE_OUTER_BOUND ( 'NONE', #17134, .T. ) ;
#39446 = VECTOR ( 'NONE', #32697, 1000.000000000000000 ) ;
#39448 = VECTOR ( 'NONE', #6618, 1000.000000000000114 ) ;
#39449 = AXIS2_PLACEMENT_3D ( 'NONE', #30034, #37375, #3343 ) ;
#39450 = CARTESIAN_POINT ( 'NONE',  ( -3.000000000000000000, -0.9646360437372163421, -23.52805723605591126 ) ) ;
#39451 = VECTOR ( 'NONE', #19023, 1000.000000000000000 ) ;
#39452 = DIRECTION ( 'NONE',  ( -1.000000000000000000, 0.000000000000000000, 0.000000000000000000 ) ) ;
#39453 = VECTOR ( 'NONE', #13118, 1000.000000000000000 ) ;
#39454 = EDGE_LOOP ( 'NONE', ( #45564, #44825, #6898, #16705 ) ) ;
#39455 = VERTEX_POINT ( 'NONE', #12379 ) ;
#39456 = EDGE_CURVE ( 'NONE', #45729, #30299, #42322, .T. ) ;
#39457 = CYLINDRICAL_SURFACE ( 'NONE', #31270, 31.99999999999998579 ) ;
#39458 = ORIENTED_EDGE ( 'NONE', *, *, #28786, .T. ) ;
#39459 = CARTESIAN_POINT ( 'NONE',  ( 10.00000000000000000, -27.05870788708250885, 26.08949754953014022 ) ) ;
#39460 = ADVANCED_FACE ( 'NONE', ( #46635 ), #39275, .T. ) ;
#39461 = VERTEX_POINT ( 'NONE', #13101 ) ;
#39462 = DIRECTION ( 'NONE',  ( 1.000000000000000000, -0.000000000000000000, -0.000000000000000000 ) ) ;
#39463 = EDGE_CURVE ( 'NONE', #23327, #32575, #7896, .T. ) ;
#39464 = AXIS2_PLACEMENT_3D ( 'NONE', #7322, #41354, #3655 ) ;
#39465 = CARTESIAN_POINT ( 'NONE',  ( 0.000000000000000000, 0.000000000000000000, 0.000000000000000000 ) ) ;
#39466 = FACE_OUTER_BOUND ( 'NONE', #17727, .T. ) ;
#39467 = ORIENTED_EDGE ( 'NONE', *, *, #2422, .F. ) ;
#39468 = AXIS2_PLACEMENT_3D ( 'NONE', #41028, #21686, #36605 ) ;
#39470 = ORIENTED_EDGE ( 'NONE', *, *, #27801, .F. ) ;
#39469 = CARTESIAN_POINT ( 'NONE',  ( 11.99999999999999822, 0.000000000000000000, 0.000000000000000000 ) ) ;
#39471 = CIRCLE ( 'NONE', #18350, 82.00000000000000000 ) ;
#39472 = ORIENTED_EDGE ( 'NONE', *, *, #5826, .T. ) ;
#39473 = DIRECTION ( 'NONE',  ( 0.000000000000000000, 0.000000000000000000, -1.000000000000000000 ) ) ;
#39474 = ADVANCED_FACE ( 'NONE', ( #38563 ), #9180, .F. ) ;
#39475 = DIRECTION ( 'NONE',  ( 1.000000000000000000, 0.000000000000000000, -0.000000000000000000 ) ) ;
#39476 = LINE ( 'NONE', #13514, #30202 ) ;
#39477 = EDGE_CURVE ( 'NONE', #6451, #16066, #38411, .T. ) ;
#39478 = CYLINDRICAL_SURFACE ( 'NONE', #28153, 31.99999999999998579 ) ;
#39479 = FACE_OUTER_BOUND ( 'NONE', #24774, .T. ) ;
#39480 = AXIS2_PLACEMENT_3D ( 'NONE', #7179, #3508, #14286 ) ;
#39481 = CIRCLE ( 'NONE', #13687, 82.00000000000000000 ) ;
#39482 = ORIENTED_EDGE ( 'NONE', *, *, #19197, .T. ) ;
#39483 = FACE_OUTER_BOUND ( 'NONE', #42087, .T. ) ;
#39484 = ORIENTED_EDGE ( 'NONE', *, *, #5850, .F. ) ;
#39485 = VERTEX_POINT ( 'NONE', #39041 ) ;
#39486 = EDGE_CURVE ( 'NONE', #40640, #20736, #12615, .T. ) ;
#39487 = CARTESIAN_POINT ( 'NONE',  ( -3.000000000000000000, 20.85821328998756385, -10.92862929874494959 ) ) ;
#39488 = CYLINDRICAL_SURFACE ( 'NONE', #47211, 77.49899999999999523 ) ;
#39489 = CARTESIAN_POINT ( 'NONE',  ( 10.00000000000000000, -80.28980883073744224, -16.65972982745018882 ) ) ;
#39490 = DIRECTION ( 'NONE',  ( -1.000000000000000000, 0.000000000000000000, -0.000000000000000000 ) ) ;
#39491 = ORIENTED_EDGE ( 'NONE', *, *, #5988, .T. ) ;
#39492 = DIRECTION ( 'NONE',  ( 1.000000000000000000, 0.000000000000000000, 0.000000000000000000 ) ) ;
#39493 = CIRCLE ( 'NONE', #1182, 82.00000000000000000 ) ;
#39494 = CYLINDRICAL_SURFACE ( 'NONE', #11980, 77.49899999999999523 ) ;
#39495 = FACE_OUTER_BOUND ( 'NONE', #39672, .T. ) ;
#39496 = FACE_OUTER_BOUND ( 'NONE', #37353, .T. ) ;
#39497 = ADVANCED_FACE ( 'NONE', ( #42470 ), #14293, .T. ) ;
#39498 = CARTESIAN_POINT ( 'NONE',  ( 2.047646702416564768, -96.54137380445985173, 5.500000000000000000 ) ) ;
#39499 = LINE ( 'NONE', #2056, #1980 ) ;
#39500 = DIRECTION ( 'NONE',  ( -1.000000000000000000, 0.000000000000000000, 0.000000000000000000 ) ) ;
#39501 = CYLINDRICAL_SURFACE ( 'NONE', #36493, 82.00000000000000000 ) ;
#39502 = DIRECTION ( 'NONE',  ( -0.3853207896976533764, 0.9227826878668546895, 0.000000000000000000 ) ) ;
#39503 = AXIS2_PLACEMENT_3D ( 'NONE', #17143, #25444, #36226 ) ;
#39504 = ORIENTED_EDGE ( 'NONE', *, *, #7567, .T. ) ;
#39505 = CARTESIAN_POINT ( 'NONE',  ( -10.00000000000000000, 0.000000000000000000, 0.000000000000000000 ) ) ;
#39506 = CARTESIAN_POINT ( 'NONE',  ( 10.00000000000000000, 15.48615015657582283, 39.04073710021349797 ) ) ;
#39507 = ORIENTED_EDGE ( 'NONE', *, *, #6737, .T. ) ;
#39508 = ORIENTED_EDGE ( 'NONE', *, *, #42083, .T. ) ;
#39509 = VECTOR ( 'NONE', #35812, 1000.000000000000000 ) ;
#39510 = CARTESIAN_POINT ( 'NONE',  ( 4.999999999999999112, 40.68715046381927891, 10.41901085202092858 ) ) ;
#39511 = EDGE_LOOP ( 'NONE', ( #45274, #16852, #3820, #45597 ) ) ;
#39512 = CARTESIAN_POINT ( 'NONE',  ( 11.99999999999999822, 73.73191006444572793, -14.66109333815486515 ) ) ;
#39513 = CIRCLE ( 'NONE', #21500, 31.99999999999999289 ) ;
#39514 = CARTESIAN_POINT ( 'NONE',  ( -21.67772167707813935, -110.8034581014852762, 5.500000000000000000 ) ) ;
#39515 = ORIENTED_EDGE ( 'NONE', *, *, #48228, .T. ) ;
#39516 = AXIS2_PLACEMENT_3D ( 'NONE', #23802, #9349, #20128 ) ;
#39517 = DIRECTION ( 'NONE',  ( -1.000000000000000000, 0.000000000000000000, 0.000000000000000000 ) ) ;
#39518 = EDGE_CURVE ( 'NONE', #36114, #34421, #875, .T. ) ;
#39519 = CIRCLE ( 'NONE', #30896, 31.99999999999999289 ) ;
#39520 = ORIENTED_EDGE ( 'NONE', *, *, #41461, .F. ) ;
#39521 = ORIENTED_EDGE ( 'NONE', *, *, #6048, .F. ) ;
#39522 = EDGE_CURVE ( 'NONE', #11209, #21073, #29004, .T. ) ;
#39523 = ORIENTED_EDGE ( 'NONE', *, *, #35324, .T. ) ;
#39524 = CIRCLE ( 'NONE', #19975, 15.99999999999999822 ) ;
#39525 = EDGE_CURVE ( 'NONE', #5144, #41422, #10378, .T. ) ;
#39526 = CIRCLE ( 'NONE', #45774, 15.99999999999999822 ) ;
#39527 = EDGE_CURVE ( 'NONE', #39726, #22743, #13394, .T. ) ;
#39528 = AXIS2_PLACEMENT_3D ( 'NONE', #45879, #25509, #32153 ) ;
#39529 = CARTESIAN_POINT ( 'NONE',  ( 10.00000000000000000, -34.44570377933649041, 69.42325613327427902 ) ) ;
#39530 = EDGE_LOOP ( 'NONE', ( #20971, #3208, #47563, #29529 ) ) ;
#39531 = EDGE_CURVE ( 'NONE', #21412, #39579, #48068, .T. ) ;
#39532 = LINE ( 'NONE', #3256, #10141 ) ;
#39533 = CARTESIAN_POINT ( 'NONE',  ( 11.99999999999999822, 41.76106447765580043, -62.50884508063379741 ) ) ;
#39534 = VERTEX_POINT ( 'NONE', #36330 ) ;
#39535 = CYLINDRICAL_SURFACE ( 'NONE', #20335, 16.00000000000000000 ) ;
#39536 = AXIS2_PLACEMENT_3D ( 'NONE', #13907, #17809, #36419 ) ;
#39537 = ORIENTED_EDGE ( 'NONE', *, *, #29303, .F. ) ;
#39538 = ORIENTED_EDGE ( 'NONE', *, *, #187, .F. ) ;
#39539 = DIRECTION ( 'NONE',  ( -0.000000000000000000, -0.000000000000000000, -1.000000000000000000 ) ) ;
#39540 = DIRECTION ( 'NONE',  ( 0.000000000000000000, 0.000000000000000000, 1.000000000000000000 ) ) ;
#39541 = EDGE_CURVE ( 'NONE', #21082, #35343, #10636, .T. ) ;
#39542 = DIRECTION ( 'NONE',  ( 0.000000000000000000, -0.5224985647159560154, 0.8526401643540879594 ) ) ;
#39543 = AXIS2_PLACEMENT_3D ( 'NONE', #19130, #8586, #34058 ) ;
#39544 = VERTEX_POINT ( 'NONE', #32886 ) ;
#39545 = ORIENTED_EDGE ( 'NONE', *, *, #44199, .T. ) ;
#39546 = DIRECTION ( 'NONE',  ( 0.000000000000000000, 0.000000000000000000, 1.000000000000000000 ) ) ;
#39547 = ORIENTED_EDGE ( 'NONE', *, *, #46732, .F. ) ;
#39548 = ADVANCED_FACE ( 'NONE', ( #44160 ), #44398, .T. ) ;
#39549 = PLANE ( 'NONE',  #48103 ) ;
#39550 = LINE ( 'NONE', #14560, #19151 ) ;
#39551 = DIRECTION ( 'NONE',  ( 0.000000000000000000, 0.5224985647159500202, -0.8526401643540915121 ) ) ;
#39552 = DIRECTION ( 'NONE',  ( -1.000000000000000000, -0.000000000000000000, -0.000000000000000000 ) ) ;
#39553 = DIRECTION ( 'NONE',  ( 0.000000000000000000, 0.000000000000000000, 1.000000000000000000 ) ) ;
#39554 = DIRECTION ( 'NONE',  ( 1.000000000000000000, -0.000000000000000000, -0.000000000000000000 ) ) ;
#39555 = CARTESIAN_POINT ( 'NONE',  ( 0.000000000000000000, -0.8261519478436571973, 77.49459641780886443 ) ) ;
#39556 = DIRECTION ( 'NONE',  ( 0.000000000000000000, 0.8910065241883657894, 0.4539904997395510788 ) ) ;
#39557 = CARTESIAN_POINT ( 'NONE',  ( 0.000000000000000000, 12.42422080174638310, 35.38097989696515810 ) ) ;
#39558 = EDGE_CURVE ( 'NONE', #23195, #22033, #2446, .T. ) ;
#39559 = CARTESIAN_POINT ( 'NONE',  ( 0.000000000000000000, 0.000000000000000000, 0.000000000000000000 ) ) ;
#39560 = AXIS2_PLACEMENT_3D ( 'NONE', #13216, #28138, #24461 ) ;
#39561 = EDGE_LOOP ( 'NONE', ( #1190, #22766, #45185, #28687 ) ) ;
#39562 = CARTESIAN_POINT ( 'NONE',  ( 0.000000000000000000, 0.000000000000000000, 0.000000000000000000 ) ) ;
#39563 = VECTOR ( 'NONE', #39790, 1000.000000000000000 ) ;
#39564 = CARTESIAN_POINT ( 'NONE',  ( 10.00000000000000000, -65.59268652807183742, -36.72794159290312166 ) ) ;
#39565 = FACE_OUTER_BOUND ( 'NONE', #22973, .T. ) ;
#39566 = VECTOR ( 'NONE', #43625, 1000.000000000000000 ) ;
#39567 = DIRECTION ( 'NONE',  ( 1.000000000000000000, 0.000000000000000000, -0.000000000000000000 ) ) ;
#39568 = EDGE_CURVE ( 'NONE', #30063, #4413, #17288, .T. ) ;
#39569 = EDGE_LOOP ( 'NONE', ( #13557, #39491, #9019, #45763 ) ) ;
#39570 = DIRECTION ( 'NONE',  ( 0.000000000000000000, 0.000000000000000000, 1.000000000000000000 ) ) ;
#39571 = CARTESIAN_POINT ( 'NONE',  ( -12.49999999999999645, 0.000000000000000000, 53.20000000000001705 ) ) ;
#39572 = ORIENTED_EDGE ( 'NONE', *, *, #18760, .T. ) ;
#39573 = CARTESIAN_POINT ( 'NONE',  ( -21.33958957442910886, -129.9559990355020034, 5.500000000000000000 ) ) ;
#39574 = VECTOR ( 'NONE', #37735, 1000.000000000000000 ) ;
#39575 = ORIENTED_EDGE ( 'NONE', *, *, #22772, .F. ) ;
#39576 = CIRCLE ( 'NONE', #3602, 42.00000000000000000 ) ;
#39577 = CARTESIAN_POINT ( 'NONE',  ( 1.474095553543393056, -119.7224350544041869, 2.500000000000000000 ) ) ;
#39578 = EDGE_LOOP ( 'NONE', ( #41025, #104, #26973, #2029 ) ) ;
#39579 = VERTEX_POINT ( 'NONE', #25775 ) ;
#39580 = EDGE_CURVE ( 'NONE', #41107, #13266, #42359, .T. ) ;
#39581 = CIRCLE ( 'NONE', #2832, 42.00000000000000000 ) ;
#39582 = EDGE_CURVE ( 'NONE', #31175, #17149, #17950, .T. ) ;
#39583 = VERTEX_POINT ( 'NONE', #32188 ) ;
#39584 = DIRECTION ( 'NONE',  ( 0.000000000000000000, -0.8090169943749532244, 0.5877852522924652545 ) ) ;
#39585 = VERTEX_POINT ( 'NONE', #7187 ) ;
#39586 = EDGE_CURVE ( 'NONE', #6313, #18371, #18092, .T. ) ;
#39587 = ORIENTED_EDGE ( 'NONE', *, *, #20229, .T. ) ;
#39588 = CIRCLE ( 'NONE', #16933, 16.00000000000000000 ) ;
#39589 = ADVANCED_FACE ( 'NONE', ( #6950 ), #21391, .T. ) ;
#39590 = DIRECTION ( 'NONE',  ( 0.000000000000000000, 0.000000000000000000, -1.000000000000000000 ) ) ;
#39592 = VERTEX_POINT ( 'NONE', #21867 ) ;
#39591 = LINE ( 'NONE', #10189, #3477 ) ;
#39593 = ORIENTED_EDGE ( 'NONE', *, *, #42204, .F. ) ;
#39594 = CIRCLE ( 'NONE', #9081, 16.00000000000000000 ) ;
#39595 = EDGE_LOOP ( 'NONE', ( #15962, #31091, #5504, #19339 ) ) ;
#39596 = VERTEX_POINT ( 'NONE', #3264 ) ;
#39597 = CYLINDRICAL_SURFACE ( 'NONE', #38921, 16.00000000000000000 ) ;
#39599 = ORIENTED_EDGE ( 'NONE', *, *, #1036, .T. ) ;
#39598 = DIRECTION ( 'NONE',  ( 0.000000000000000000, 0.000000000000000000, 1.000000000000000000 ) ) ;
#39600 = CYLINDRICAL_SURFACE ( 'NONE', #21974, 42.00000000000000000 ) ;
#39601 = ORIENTED_EDGE ( 'NONE', *, *, #4365, .F. ) ;
#39602 = ORIENTED_EDGE ( 'NONE', *, *, #26536, .T. ) ;
#39603 = VECTOR ( 'NONE', #46477, 1000.000000000000000 ) ;
#39604 = AXIS2_PLACEMENT_3D ( 'NONE', #6652, #25958, #29149 ) ;
#39605 = VERTEX_POINT ( 'NONE', #18189 ) ;
#39606 = DIRECTION ( 'NONE',  ( -1.000000000000000000, 0.000000000000000000, -0.000000000000000000 ) ) ;
#39607 = ORIENTED_EDGE ( 'NONE', *, *, #48286, .F. ) ;
#39608 = CARTESIAN_POINT ( 'NONE',  ( 10.00000000000000000, -22.48208911017474065, -35.47612816024548721 ) ) ;
#39609 = CYLINDRICAL_SURFACE ( 'NONE', #44429, 16.00000000000000000 ) ;
#39610 = CIRCLE ( 'NONE', #41077, 77.49900000000000944 ) ;
#39611 = DIRECTION ( 'NONE',  ( 0.000000000000000000, 0.000000000000000000, -1.000000000000000000 ) ) ;
#39612 = DIRECTION ( 'NONE',  ( -1.000000000000000000, 0.000000000000000000, -0.000000000000000000 ) ) ;
#39613 = DIRECTION ( 'NONE',  ( -1.000000000000000000, 0.000000000000000000, 0.000000000000000000 ) ) ;
#39614 = VECTOR ( 'NONE', #19106, 1000.000000000000000 ) ;
#39615 = DIRECTION ( 'NONE',  ( 0.000000000000000000, 0.000000000000000000, 1.000000000000000000 ) ) ;
#39616 = VECTOR ( 'NONE', #36166, 1000.000000000000000 ) ;
#39617 = DIRECTION ( 'NONE',  ( -1.000000000000000000, -0.000000000000000000, -0.000000000000000000 ) ) ;
#39618 = ORIENTED_EDGE ( 'NONE', *, *, #36630, .F. ) ;
#39619 = CARTESIAN_POINT ( 'NONE',  ( 0.000000000000000000, -29.81001611430991360, -22.74946021919165418 ) ) ;
#39620 = ORIENTED_EDGE ( 'NONE', *, *, #36413, .T. ) ;
#39621 = LINE ( 'NONE', #9736, #16821 ) ;
#39622 = DIRECTION ( 'NONE',  ( -1.000000000000000000, -0.000000000000000000, -0.000000000000000000 ) ) ;
#39623 = DIRECTION ( 'NONE',  ( -1.000000000000000000, 0.000000000000000000, 0.000000000000000000 ) ) ;
#39624 = DIRECTION ( 'NONE',  ( -1.000000000000000000, 0.000000000000000000, -0.000000000000000000 ) ) ;
#39625 = DIRECTION ( 'NONE',  ( 0.000000000000000000, 0.000000000000000000, 1.000000000000000000 ) ) ;
#39626 = LINE ( 'NONE', #28109, #20074 ) ;
#39627 = AXIS2_PLACEMENT_3D ( 'NONE', #17235, #42728, #36089 ) ;
#39628 = EDGE_LOOP ( 'NONE', ( #30508, #43555, #11224, #43438 ) ) ;
#39629 = CARTESIAN_POINT ( 'NONE',  ( 0.000000000000000000, -18.13022148937263012, 15.02647892043544608 ) ) ;
#39630 = CARTESIAN_POINT ( 'NONE',  ( 0.000000000000000000, 2.543863470249533965, -81.96053171279901051 ) ) ;
#39631 = CYLINDRICAL_SURFACE ( 'NONE', #4384, 77.49899999999999523 ) ;
#39632 = ORIENTED_EDGE ( 'NONE', *, *, #2858, .T. ) ;
#39633 = VECTOR ( 'NONE', #12756, 1000.000000000000000 ) ;
#39634 = CARTESIAN_POINT ( 'NONE',  ( 0.000000000000000000, 8.966570791701863996, -81.50828551894218776 ) ) ;
#39635 = SHAPE_REPRESENTATION_RELATIONSHIP ( 'NONE' , 'NONE' ,  #29385, #47339 ) ;
#39636 = ORIENTED_EDGE ( 'NONE', *, *, #20789, .T. ) ;
#39637 = EDGE_LOOP ( 'NONE', ( #2593, #44070, #784, #19992 ) ) ;
#39638 = EDGE_CURVE ( 'NONE', #13990, #29283, #34511, .T. ) ;
#39639 = CIRCLE ( 'NONE', #13849, 37.49900000000000944 ) ;
#39640 = EDGE_CURVE ( 'NONE', #43899, #17111, #2791, .T. ) ;
#39641 = EDGE_LOOP ( 'NONE', ( #12982, #16527 ) ) ;
#39642 = CARTESIAN_POINT ( 'NONE',  ( 12.00000000000000000, 23.59884966291538078, 12.14883922797231008 ) ) ;
#39643 = ADVANCED_FACE ( 'NONE', ( #13573 ), #14052, .T. ) ;
#39644 = CIRCLE ( 'NONE', #9930, 42.00000000000000000 ) ;
#39645 = DIRECTION ( 'NONE',  ( -1.000000000000000000, -0.000000000000000000, -0.000000000000000000 ) ) ;
#39646 = ORIENTED_EDGE ( 'NONE', *, *, #5301, .T. ) ;
#39647 = AXIS2_PLACEMENT_3D ( 'NONE', #41480, #37075, #105 ) ;
#39648 = VERTEX_POINT ( 'NONE', #76 ) ;
#39649 = EDGE_CURVE ( 'NONE', #28383, #28563, #7441, .T. ) ;
#39650 = DIRECTION ( 'NONE',  ( -1.000000000000000000, 0.000000000000000000, 0.000000000000000000 ) ) ;
#39651 = ORIENTED_EDGE ( 'NONE', *, *, #317, .F. ) ;
#39652 = ORIENTED_EDGE ( 'NONE', *, *, #22024, .F. ) ;
#39653 = ORIENTED_EDGE ( 'NONE', *, *, #8180, .F. ) ;
#39654 = EDGE_CURVE ( 'NONE', #36243, #43300, #44690, .T. ) ;
#39655 = ORIENTED_EDGE ( 'NONE', *, *, #42451, .F. ) ;
#39656 = CIRCLE ( 'NONE', #18538, 42.00000000000000000 ) ;
#39657 = DIRECTION ( 'NONE',  ( 0.9580045777625456616, 0.2867529058022021404, 0.000000000000000000 ) ) ;
#39658 = VERTEX_POINT ( 'NONE', #45347 ) ;
#39659 = ORIENTED_EDGE ( 'NONE', *, *, #19067, .T. ) ;
#39660 = DIRECTION ( 'NONE',  ( 0.000000000000000000, 0.7071067811865487940, -0.7071067811865462405 ) ) ;
#39661 = ORIENTED_EDGE ( 'NONE', *, *, #35049, .F. ) ;
#39662 = CARTESIAN_POINT ( 'NONE',  ( 10.00000000000000000, 59.03342792756263435, 46.54456581323825048 ) ) ;
#39663 = AXIS2_PLACEMENT_3D ( 'NONE', #15174, #30099, #45027 ) ;
#39664 = CARTESIAN_POINT ( 'NONE',  ( 0.000000000000000000, -76.69515212745996280, -29.01471420065643869 ) ) ;
#39665 = CARTESIAN_POINT ( 'NONE',  ( 0.000000000000000000, 75.54627589209944460, 17.28742895386110945 ) ) ;
#39666 = ORIENTED_EDGE ( 'NONE', *, *, #27208, .F. ) ;
#39667 = CARTESIAN_POINT ( 'NONE',  ( -2.977765906491215642, 0.000000000000000000, 0.000000000000000000 ) ) ;
#39668 = ORIENTED_EDGE ( 'NONE', *, *, #5724, .T. ) ;
#39669 = CARTESIAN_POINT ( 'NONE',  ( 0.000000000000000000, -81.50828551894234408, 8.966570791700414489 ) ) ;
#39670 = CARTESIAN_POINT ( 'NONE',  ( 0.000000000000000000, 37.22597642581158084, 10.79786254984347593 ) ) ;
#39671 = CIRCLE ( 'NONE', #21685, 31.99999999999998579 ) ;
#39672 = EDGE_LOOP ( 'NONE', ( #37352, #8320, #31720, #9524 ) ) ;
#39673 = EDGE_LOOP ( 'NONE', ( #2202, #45393, #45664, #26458 ) ) ;
#39674 = CARTESIAN_POINT ( 'NONE',  ( 12.49999999999999645, 1.530808498934191127E-15, 53.20000000000001705 ) ) ;
#39675 = CARTESIAN_POINT ( 'NONE',  ( 0.000000000000000000, -31.52238457039579345, -27.75498641678775158 ) ) ;
#39676 = ORIENTED_EDGE ( 'NONE', *, *, #13886, .T. ) ;
#39677 = DIRECTION ( 'NONE',  ( 0.000000000000000000, 0.9876883405951382144, -0.1564344650402276493 ) ) ;
#39678 = DIRECTION ( 'NONE',  ( -1.000000000000000000, 0.000000000000000000, -0.000000000000000000 ) ) ;
#39679 = FACE_OUTER_BOUND ( 'NONE', #5194, .T. ) ;
#39680 = DIRECTION ( 'NONE',  ( 0.2306669878475637314, 0.9730327541852493711, -0.000000000000000000 ) ) ;
#39681 = CIRCLE ( 'NONE', #35779, 31.99999999999999289 ) ;
#39682 = DIRECTION ( 'NONE',  ( 0.000000000000000000, 0.000000000000000000, -1.000000000000000000 ) ) ;
#39683 = ADVANCED_FACE ( 'NONE', ( #30433 ), #26027, .T. ) ;
#39684 = CARTESIAN_POINT ( 'NONE',  ( 0.000000000000000000, 22.48208911017551515, -35.47612816024499693 ) ) ;
#39685 = DIRECTION ( 'NONE',  ( -1.000000000000000000, 0.000000000000000000, -0.000000000000000000 ) ) ;
#39686 = ADVANCED_FACE ( 'NONE', ( #11594 ), #33847, .F. ) ;
#39687 = DIRECTION ( 'NONE',  ( -1.000000000000000000, -0.000000000000000000, 0.000000000000000000 ) ) ;
#39688 = DIRECTION ( 'NONE',  ( -1.000000000000000000, 0.000000000000000000, -0.000000000000000000 ) ) ;
#39689 = LINE ( 'NONE', #13732, #11589 ) ;
#39690 = DIRECTION ( 'NONE',  ( -1.000000000000000000, -0.000000000000000000, -0.000000000000000000 ) ) ;
#39691 = EDGE_CURVE ( 'NONE', #15851, #21692, #17325, .T. ) ;
#39692 = CARTESIAN_POINT ( 'NONE',  ( 10.00000000000000000, 0.000000000000000000, 0.000000000000000000 ) ) ;
#39693 = VERTEX_POINT ( 'NONE', #572 ) ;
#39694 = ORIENTED_EDGE ( 'NONE', *, *, #21984, .T. ) ;
#39695 = VECTOR ( 'NONE', #45300, 1000.000000000000000 ) ;
#39696 = DIRECTION ( 'NONE',  ( 1.000000000000000000, -0.000000000000000000, -0.000000000000000000 ) ) ;
#39697 = CARTESIAN_POINT ( 'NONE',  ( 5.999999999999999112, -40.65526001592663619, 71.21200624218782593 ) ) ;
#39698 = AXIS2_PLACEMENT_3D ( 'NONE', #31256, #14263, #35384 ) ;
#39699 = EDGE_CURVE ( 'NONE', #16099, #19725, #29698, .T. ) ;
#39700 = DIRECTION ( 'NONE',  ( -1.000000000000000000, 0.000000000000000000, -0.000000000000000000 ) ) ;
#39701 = ORIENTED_EDGE ( 'NONE', *, *, #8610, .T. ) ;
#39702 = ADVANCED_FACE ( 'NONE', ( #3759 ), #29944, .T. ) ;
#39703 = EDGE_CURVE ( 'NONE', #23034, #13690, #7169, .T. ) ;
#39704 = EDGE_LOOP ( 'NONE', ( #28671, #7242, #47736, #13431 ) ) ;
#39705 = AXIS2_PLACEMENT_3D ( 'NONE', #27105, #12895, #5787 ) ;
#39706 = LINE ( 'NONE', #21069, #46115 ) ;
#39707 = DIRECTION ( 'NONE',  ( -1.000000000000000000, 0.000000000000000000, 0.000000000000000000 ) ) ;
#39708 = VERTEX_POINT ( 'NONE', #26285 ) ;
#39709 = DIRECTION ( 'NONE',  ( -1.000000000000000000, -0.000000000000000000, -0.000000000000000000 ) ) ;
#39710 = PRODUCT_RELATED_PRODUCT_CATEGORY ( 'part', '', ( #21428 ) ) ;
#39711 = AXIS2_PLACEMENT_3D ( 'NONE', #41600, #8057, #30353 ) ;
#39712 = LINE ( 'NONE', #2475, #12567 ) ;
#39713 = DIRECTION ( 'NONE',  ( 0.000000000000000000, 0.9135454576426055295, 0.4067366430757899387 ) ) ;
#39714 = ORIENTED_EDGE ( 'NONE', *, *, #497, .F. ) ;
#39715 = FACE_OUTER_BOUND ( 'NONE', #45159, .T. ) ;
#39716 = ORIENTED_EDGE ( 'NONE', *, *, #13211, .T. ) ;
#39717 = PLANE ( 'NONE',  #16569 ) ;
#39718 = VERTEX_POINT ( 'NONE', #18449 ) ;
#39719 = DIRECTION ( 'NONE',  ( 1.000000000000000000, -0.000000000000000000, -0.000000000000000000 ) ) ;
#39720 = DIRECTION ( 'NONE',  ( 0.000000000000000000, 0.4539904997395479702, -0.8910065241883673437 ) ) ;
#39721 = DIRECTION ( 'NONE',  ( -1.000000000000000000, 0.000000000000000000, 0.000000000000000000 ) ) ;
#39722 = DIRECTION ( 'NONE',  ( -1.000000000000000000, 0.000000000000000000, 0.000000000000000000 ) ) ;
#39723 = ORIENTED_EDGE ( 'NONE', *, *, #41282, .F. ) ;
#39724 = CYLINDRICAL_SURFACE ( 'NONE', #38917, 32.00000000000000000 ) ;
#39725 = VERTEX_POINT ( 'NONE', #41217 ) ;
#39726 = VERTEX_POINT ( 'NONE', #7674 ) ;
#39727 = DIRECTION ( 'NONE',  ( -1.000000000000000000, 0.000000000000000000, -0.000000000000000000 ) ) ;
#39728 = VERTEX_POINT ( 'NONE', #37771 ) ;
#39729 = VECTOR ( 'NONE', #31496, 1000.000000000000000 ) ;
#39730 = DIRECTION ( 'NONE',  ( 0.000000000000000000, 0.5877852522924743583, -0.8090169943749465631 ) ) ;
#39731 = DIRECTION ( 'NONE',  ( -1.000000000000000000, -0.000000000000000000, 0.000000000000000000 ) ) ;
#39732 = DIRECTION ( 'NONE',  ( -1.000000000000000000, -0.000000000000000000, 0.000000000000000000 ) ) ;
#39733 = ORIENTED_EDGE ( 'NONE', *, *, #25183, .F. ) ;
#39734 = DIRECTION ( 'NONE',  ( -1.000000000000000000, 0.000000000000000000, -0.000000000000000000 ) ) ;
#39735 = VECTOR ( 'NONE', #9707, 1000.000000000000000 ) ;
#39736 = DIRECTION ( 'NONE',  ( 0.000000000000000000, 0.000000000000000000, 1.000000000000000000 ) ) ;
#39737 = CYLINDRICAL_SURFACE ( 'NONE', #28240, 31.99999999999998579 ) ;
#39738 = CARTESIAN_POINT ( 'NONE',  ( 0.000000000000000000, -10.74501242461307982, 35.92658777277507198 ) ) ;
#39739 = LINE ( 'NONE', #17687, #27078 ) ;
#39740 = EDGE_CURVE ( 'NONE', #14155, #8812, #37528, .T. ) ;
#39741 = CARTESIAN_POINT ( 'NONE',  ( 12.00000000000000000, 16.61724383029390140, 20.69703378468902955 ) ) ;
#39742 = DIRECTION ( 'NONE',  ( 0.000000000000000000, 0.000000000000000000, -1.000000000000000000 ) ) ;
#39743 = DIRECTION ( 'NONE',  ( 1.000000000000000000, -0.000000000000000000, -0.000000000000000000 ) ) ;
#39744 = CARTESIAN_POINT ( 'NONE',  ( 6.000000000000000000, 78.73519480814985627, -22.90783923731547489 ) ) ;
#39745 = ADVANCED_FACE ( 'NONE', ( #38024 ), #321, .T. ) ;
#39746 = CARTESIAN_POINT ( 'NONE',  ( 11.99999999999999822, 50.95692526931414790, -58.39081064771693974 ) ) ;
#39747 = DIRECTION ( 'NONE',  ( -1.000000000000000000, 0.000000000000000000, -0.000000000000000000 ) ) ;
#39748 = MECHANICAL_DESIGN_GEOMETRIC_PRESENTATION_REPRESENTATION (  '', ( #2997 ), #46795 ) ;
#39749 = ADVANCED_FACE ( 'NONE', ( #41449 ), #4492, .F. ) ;
#39750 = ORIENTED_EDGE ( 'NONE', *, *, #23213, .T. ) ;
#39751 = VECTOR ( 'NONE', #12158, 1000.000000000000000 ) ;
#39752 = EDGE_LOOP ( 'NONE', ( #38685, #5956, #43573, #45706 ) ) ;
#39753 = DIRECTION ( 'NONE',  ( 0.1276937514489679681, 0.9918136447140103451, 0.000000000000000000 ) ) ;
#39754 = EDGE_LOOP ( 'NONE', ( #32143, #26690, #38383, #28965 ) ) ;
#39755 = CARTESIAN_POINT ( 'NONE',  ( -0.8815729230226008184, -93.47222532549339746, 2.500000000000000000 ) ) ;
#39756 = CARTESIAN_POINT ( 'NONE',  ( 10.00000000000000000, 41.81611651403867569, -3.925862922255714871 ) ) ;
#39757 = VERTEX_POINT ( 'NONE', #34323 ) ;
#39758 = EDGE_CURVE ( 'NONE', #28940, #47865, #797, .T. ) ;
#39759 = EDGE_CURVE ( 'NONE', #22715, #42340, #41944, .T. ) ;
#39760 = CARTESIAN_POINT ( 'NONE',  ( 0.000000000000000000, 68.27212725128275395, 31.46837873495001503 ) ) ;
#39761 = ORIENTED_EDGE ( 'NONE', *, *, #36433, .F. ) ;
#39762 = VECTOR ( 'NONE', #39358, 1000.000000000000000 ) ;
#39763 = AXIS2_PLACEMENT_3D ( 'NONE', #24597, #28512, #37769 ) ;
#39764 = VERTEX_POINT ( 'NONE', #37046 ) ;
#39765 = VERTEX_POINT ( 'NONE', #48305 ) ;
#39766 = ADVANCED_FACE ( 'NONE', ( #14783 ), #11107, .T. ) ;
#39767 = DIRECTION ( 'NONE',  ( 0.000000000000000000, -0.3090169943749549453, 0.9510565162951511997 ) ) ;
#39768 = ORIENTED_EDGE ( 'NONE', *, *, #9485, .F. ) ;
#39769 = CARTESIAN_POINT ( 'NONE',  ( 10.00000000000000000, -37.22597642581153821, -5.202137450156795850 ) ) ;
#39770 = CARTESIAN_POINT ( 'NONE',  ( 10.00000000000000000, 39.04073710021366139, -15.48615015657542848 ) ) ;
#39771 = ORIENTED_EDGE ( 'NONE', *, *, #11398, .T. ) ;
#39772 = DIRECTION ( 'NONE',  ( 1.000000000000000000, -0.000000000000000000, -0.000000000000000000 ) ) ;
#39773 = ORIENTED_EDGE ( 'NONE', *, *, #9674, .F. ) ;
#39774 = LINE ( 'NONE', #40009, #40555 ) ;
#39775 = CARTESIAN_POINT ( 'NONE',  ( 0.000000000000000000, 71.21200624218795383, 40.65526001592638039 ) ) ;
#39776 = CARTESIAN_POINT ( 'NONE',  ( 10.00000000000000000, 62.20884554314086046, -46.21855187248561236 ) ) ;
#39777 = AXIS2_PLACEMENT_3D ( 'NONE', #8837, #38729, #291 ) ;
#39778 = ORIENTED_EDGE ( 'NONE', *, *, #46384, .T. ) ;
#39779 = DIRECTION ( 'NONE',  ( 0.000000000000000000, 0.6494480483301793283, 0.7604059656000345946 ) ) ;
#39780 = VERTEX_POINT ( 'NONE', #30934 ) ;
#39781 = DIRECTION ( 'NONE',  ( -1.000000000000000000, -0.000000000000000000, -0.000000000000000000 ) ) ;
#39782 = DIRECTION ( 'NONE',  ( 0.4279312458753000703, 0.9038112904824842087, -0.000000000000000000 ) ) ;
#39783 = DIRECTION ( 'NONE',  ( -1.000000000000000000, 0.000000000000000000, -0.000000000000000000 ) ) ;
#39784 = DIRECTION ( 'NONE',  ( 0.000000000000000000, 0.5224985647159500202, -0.8526401643540915121 ) ) ;
#39785 = CARTESIAN_POINT ( 'NONE',  ( 15.00000000000000000, 14.60985201121729737, 18.46759930825687235 ) ) ;
#39786 = DIRECTION ( 'NONE',  ( 0.000000000000000000, 0.000000000000000000, 1.000000000000000000 ) ) ;
#39787 = DIRECTION ( 'NONE',  ( 0.000000000000000000, 0.8090169943749486725, -0.5877852522924714718 ) ) ;
#39788 = CARTESIAN_POINT ( 'NONE',  ( 11.99999999999999822, -5.256550761632340141, -77.32052557432847095 ) ) ;
#39789 = DIRECTION ( 'NONE',  ( 1.000000000000000000, 0.000000000000000000, 0.000000000000000000 ) ) ;
#39790 = DIRECTION ( 'NONE',  ( -1.000000000000000000, 0.000000000000000000, -0.000000000000000000 ) ) ;
#39791 = EDGE_LOOP ( 'NONE', ( #12744, #27791, #18645, #16122 ) ) ;
#39792 = VECTOR ( 'NONE', #29805, 1000.000000000000000 ) ;
#39793 = DIRECTION ( 'NONE',  ( -8.090853898039828715E-17, 9.269810975720166919E-17, -1.000000000000000000 ) ) ;
#39795 = ADVANCED_FACE ( 'NONE', ( #27495 ), #32206, .F. ) ;
#39794 = CIRCLE ( 'NONE', #21011, 16.00000000000000355 ) ;
#39796 = AXIS2_PLACEMENT_3D ( 'NONE', #30758, #37612, #4804 ) ;
#39797 = CARTESIAN_POINT ( 'NONE',  ( -11.99999999999999645, 0.000000000000000000, 12.85999999999999943 ) ) ;
#39798 = CARTESIAN_POINT ( 'NONE',  ( 0.000000000000000000, 46.11716303203186840, 67.80270845531904911 ) ) ;
#39799 = VECTOR ( 'NONE', #4255, 1000.000000000000000 ) ;
#39800 = EDGE_CURVE ( 'NONE', #5216, #23160, #1542, .T. ) ;
#39801 = LINE ( 'NONE', #21172, #38775 ) ;
#39802 = CARTESIAN_POINT ( 'NONE',  ( 12.00000000000000000, -22.67460108101782978, -6.353146135317906840 ) ) ;
#39803 = CARTESIAN_POINT ( 'NONE',  ( 10.00000000000000000, -27.75498641678764855, 31.52238457039589647 ) ) ;
#39805 = EDGE_CURVE ( 'NONE', #46337, #26870, #22009, .T. ) ;
#39804 = ORIENTED_EDGE ( 'NONE', *, *, #3191, .F. ) ;
#39806 = DIRECTION ( 'NONE',  ( 0.000000000000000000, 0.000000000000000000, 1.000000000000000000 ) ) ;
#39807 = CARTESIAN_POINT ( 'NONE',  ( 0.000000000000000000, -28.89263327155795480, 71.91182617369177876 ) ) ;
#39808 = VERTEX_POINT ( 'NONE', #38499 ) ;
#39809 = ORIENTED_EDGE ( 'NONE', *, *, #42494, .T. ) ;
#39810 = EDGE_CURVE ( 'NONE', #4186, #23327, #899, .T. ) ;
#39811 = STYLED_ITEM ( 'NONE', ( #7819 ), #20448 ) ;
#39812 = EDGE_CURVE ( 'NONE', #25548, #31823, #5611, .T. ) ;
#39813 = EDGE_LOOP ( 'NONE', ( #22956, #1161, #6777, #25436 ) ) ;
#39814 = CARTESIAN_POINT ( 'NONE',  ( 21.85433023846371370, -135.0628101570779620, 5.500000000000000000 ) ) ;
#39815 = ORIENTED_EDGE ( 'NONE', *, *, #36034, .T. ) ;
#39816 = ORIENTED_EDGE ( 'NONE', *, *, #27474, .T. ) ;
#39817 = ADVANCED_FACE ( 'NONE', ( #46326 ), #1039, .T. ) ;
#39818 = VECTOR ( 'NONE', #46340, 1000.000000000000000 ) ;
#39819 = CIRCLE ( 'NONE', #17882, 77.49900000000000944 ) ;
#39820 = DIRECTION ( 'NONE',  ( -1.000000000000000000, 0.000000000000000000, 0.000000000000000000 ) ) ;
#39822 = VERTEX_POINT ( 'NONE', #34823 ) ;
#39821 = CARTESIAN_POINT ( 'NONE',  ( 0.000000000000000000, 30.41916302227113178, 71.27951684758036777 ) ) ;
#39823 = AXIS2_PLACEMENT_3D ( 'NONE', #43001, #20725, #17043 ) ;
#39824 = VERTEX_POINT ( 'NONE', #8621 ) ;
#39825 = VERTEX_POINT ( 'NONE', #23560 ) ;
#39826 = ORIENTED_EDGE ( 'NONE', *, *, #29087, .T. ) ;
#39827 = CARTESIAN_POINT ( 'NONE',  ( 10.00000000000000000, -37.48860685352291711, 0.8828120875899322373 ) ) ;
#39828 = DIRECTION ( 'NONE',  ( -1.000000000000000000, 0.000000000000000000, 0.000000000000000000 ) ) ;
#39829 = EDGE_CURVE ( 'NONE', #26069, #40081, #32946, .T. ) ;
#39830 = CARTESIAN_POINT ( 'NONE',  ( -2.977765906491215642, 0.000000000000000000, 0.000000000000000000 ) ) ;
#39831 = ORIENTED_EDGE ( 'NONE', *, *, #882, .T. ) ;
#39832 = ORIENTED_EDGE ( 'NONE', *, *, #34856, .T. ) ;
#39833 = CIRCLE ( 'NONE', #24206, 16.00000000000000000 ) ;
#39834 = DIRECTION ( 'NONE',  ( 1.000000000000000000, 0.000000000000000000, 0.000000000000000000 ) ) ;
#39835 = VERTEX_POINT ( 'NONE', #19880 ) ;
#39836 = DIRECTION ( 'NONE',  ( -1.000000000000000000, -0.000000000000000000, 0.000000000000000000 ) ) ;
#39837 = DIRECTION ( 'NONE',  ( 0.000000000000000000, 0.000000000000000000, 1.000000000000000000 ) ) ;
#39838 = CARTESIAN_POINT ( 'NONE',  ( 0.000000000000000000, 0.000000000000000000, 2.500000000000000000 ) ) ;
#39839 = DIRECTION ( 'NONE',  ( -1.000000000000000000, 0.000000000000000000, 0.000000000000000000 ) ) ;
#39840 = DIRECTION ( 'NONE',  ( 0.000000000000000000, 0.000000000000000000, 1.000000000000000000 ) ) ;
#39841 = CARTESIAN_POINT ( 'NONE',  ( 7.468086116107294004, -12.33868914344945189, -1.199999999999999956 ) ) ;
#39842 = CARTESIAN_POINT ( 'NONE',  ( 0.000000000000000000, -21.40280677340398086, 36.13751322684410638 ) ) ;
#39843 = ORIENTED_EDGE ( 'NONE', *, *, #19034, .F. ) ;
#39844 = ADVANCED_FACE ( 'NONE', ( #31170 ), #9124, .T. ) ;
#39845 = LINE ( 'NONE', #10942, #31165 ) ;
#39846 = ORIENTED_EDGE ( 'NONE', *, *, #44723, .T. ) ;
#39847 = DIRECTION ( 'NONE',  ( 0.000000000000000000, 0.9969173337331276308, 0.07845909572784864894 ) ) ;
#39848 = ADVANCED_FACE ( 'NONE', ( #12558 ), #20363, .F. ) ;
#39849 = DIRECTION ( 'NONE',  ( 1.000000000000000000, -0.000000000000000000, 0.000000000000000000 ) ) ;
#39850 = CARTESIAN_POINT ( 'NONE',  ( 10.00000000000000000, 0.000000000000000000, 0.000000000000000000 ) ) ;
#39851 = CARTESIAN_POINT ( 'NONE',  ( 0.000000000000000000, -6.903761155837269570, -77.19088730480530103 ) ) ;
#39852 = EDGE_CURVE ( 'NONE', #17581, #36114, #23811, .T. ) ;
#39853 = CARTESIAN_POINT ( 'NONE',  ( 0.000000000000000000, 0.000000000000000000, 0.000000000000000000 ) ) ;
#39854 = AXIS2_PLACEMENT_3D ( 'NONE', #17854, #32780, #40393 ) ;
#39855 = CARTESIAN_POINT ( 'NONE',  ( 11.99999999999999822, 0.000000000000000000, 0.000000000000000000 ) ) ;
#39856 = DIRECTION ( 'NONE',  ( 0.6575728627325957421, -0.7533909544171993877, -1.230411769795008318E-16 ) ) ;
#39857 = AXIS2_PLACEMENT_3D ( 'NONE', #45399, #8206, #11416 ) ;
#39858 = CARTESIAN_POINT ( 'NONE',  ( 10.00000000000000000, 0.000000000000000000, 0.000000000000000000 ) ) ;
#39859 = ADVANCED_FACE ( 'NONE', ( #46091 ), #34563, .F. ) ;
#39860 = VECTOR ( 'NONE', #6989, 1000.000000000000000 ) ;
#39861 = DIRECTION ( 'NONE',  ( 0.7533909544171998318, 0.6575728627325954090, 0.000000000000000000 ) ) ;
#39862 =( NAMED_UNIT ( * ) PLANE_ANGLE_UNIT ( ) SI_UNIT ( $, .RADIAN. ) );
#39863 = CIRCLE ( 'NONE', #46223, 77.49899999999998101 ) ;
#39864 = ORIENTED_EDGE ( 'NONE', *, *, #34557, .T. ) ;
#39865 = ORIENTED_EDGE ( 'NONE', *, *, #9505, .T. ) ;
#39866 = VERTEX_POINT ( 'NONE', #27980 ) ;
#39867 = CIRCLE ( 'NONE', #13311, 32.00000000000000000 ) ;
#39868 = DIRECTION ( 'NONE',  ( 0.000000000000000000, 0.000000000000000000, 1.000000000000000000 ) ) ;
#39869 = FACE_OUTER_BOUND ( 'NONE', #14307, .T. ) ;
#39870 = VERTEX_POINT ( 'NONE', #9356 ) ;
#39871 = EDGE_CURVE ( 'NONE', #45060, #6106, #8396, .T. ) ;
#39872 = CARTESIAN_POINT ( 'NONE',  ( 5.000000000000002665, 71.87247863392414615, 39.47590169984871267 ) ) ;
#39873 = ORIENTED_EDGE ( 'NONE', *, *, #27187, .T. ) ;
#39874 = ORIENTED_EDGE ( 'NONE', *, *, #35204, .T. ) ;
#39875 = ORIENTED_EDGE ( 'NONE', *, *, #10281, .T. ) ;
#39876 = EDGE_CURVE ( 'NONE', #4851, #18715, #41373, .T. ) ;
#39877 = VECTOR ( 'NONE', #3568, 1000.000000000000000 ) ;
#39878 = DIRECTION ( 'NONE',  ( -1.000000000000000000, 0.000000000000000000, 0.000000000000000000 ) ) ;
#39880 = ORIENTED_EDGE ( 'NONE', *, *, #38868, .T. ) ;
#39879 = AXIS2_PLACEMENT_3D ( 'NONE', #24335, #27788, #23609 ) ;
#39881 = DIRECTION ( 'NONE',  ( -1.000000000000000000, 0.000000000000000000, -0.000000000000000000 ) ) ;
#39882 = VERTEX_POINT ( 'NONE', #15427 ) ;
#39883 = DIRECTION ( 'NONE',  ( -0.000000000000000000, -0.6691306063588670083, -0.7431448254773863615 ) ) ;
#39884 = VECTOR ( 'NONE', #47502, 1000.000000000000114 ) ;
#39885 = CARTESIAN_POINT ( 'NONE',  ( 10.00000000000000000, -23.16143007188481207, 73.95703589263968070 ) ) ;
#39886 = CARTESIAN_POINT ( 'NONE',  ( 16.84844760790522855, -103.5491698323862124, 2.500000000000000000 ) ) ;
#39887 = ORIENTED_EDGE ( 'NONE', *, *, #27844, .F. ) ;
#39888 = AXIS2_PLACEMENT_3D ( 'NONE', #2714, #10797, #6643 ) ;
#39889 = DIRECTION ( 'NONE',  ( 0.000000000000000000, 0.000000000000000000, -1.000000000000000000 ) ) ;
#39890 = VERTEX_POINT ( 'NONE', #38179 ) ;
#39891 = CIRCLE ( 'NONE', #4818, 82.00000000000000000 ) ;
#39892 = DIRECTION ( 'NONE',  ( 0.000000000000000000, 0.8660254037844363761, 0.5000000000000039968 ) ) ;
#39893 = DIRECTION ( 'NONE',  ( -1.000000000000000000, -0.000000000000000000, -0.000000000000000000 ) ) ;
#39894 = ORIENTED_EDGE ( 'NONE', *, *, #1090, .T. ) ;
#39895 = AXIS2_PLACEMENT_3D ( 'NONE', #45070, #30615, #26956 ) ;
#39896 = ORIENTED_EDGE ( 'NONE', *, *, #46710, .T. ) ;
#39897 = EDGE_CURVE ( 'NONE', #36121, #36422, #1028, .T. ) ;
#39898 = CARTESIAN_POINT ( 'NONE',  ( 5.000000000000000000, 3.925862922256160736, 41.81611651403863306 ) ) ;
#39899 = DIRECTION ( 'NONE',  ( 0.000000000000000000, 0.000000000000000000, 1.000000000000000000 ) ) ;
#39900 = ORIENTED_EDGE ( 'NONE', *, *, #4810, .F. ) ;
#39901 = VERTEX_POINT ( 'NONE', #33762 ) ;
#39902 = CARTESIAN_POINT ( 'NONE',  ( 0.000000000000000000, 11.30684508768339569, 76.66974797899841576 ) ) ;
#39903 = DIRECTION ( 'NONE',  ( 1.000000000000000000, 0.000000000000000000, 0.000000000000000000 ) ) ;
#39904 = CARTESIAN_POINT ( 'NONE',  ( -3.000000000000000000, 0.000000000000000000, 0.000000000000000000 ) ) ;
#39905 = ORIENTED_EDGE ( 'NONE', *, *, #6812, .F. ) ;
#39906 = ADVANCED_FACE ( 'NONE', ( #8543 ), #19321, .F. ) ;
#39907 = DIRECTION ( 'NONE',  ( -1.000000000000000000, -0.000000000000000000, 0.000000000000000000 ) ) ;
#39908 = CARTESIAN_POINT ( 'NONE',  ( 0.000000000000000000, 70.53064760720278059, 26.01480285779964774 ) ) ;
#39909 = DIRECTION ( 'NONE',  ( -1.000000000000000000, 0.000000000000000000, -0.000000000000000000 ) ) ;
#39910 = CARTESIAN_POINT ( 'NONE',  ( 15.00000000000000000, 6.762365576493310826, -25.66652317338401090 ) ) ;
#39911 = ADVANCED_FACE ( 'NONE', ( #23247 ), #45770, .T. ) ;
#39912 = ADVANCED_FACE ( 'NONE', ( #41139 ), #30118, .T. ) ;
#39913 = CARTESIAN_POINT ( 'NONE',  ( 0.000000000000000000, 31.47745569255237896, -68.26794271651228030 ) ) ;
#39914 = LINE ( 'NONE', #36228, #44117 ) ;
#39915 = DIRECTION ( 'NONE',  ( -0.000000000000000000, -0.000000000000000000, -1.000000000000000000 ) ) ;
#39916 = CARTESIAN_POINT ( 'NONE',  ( 0.000000000000000000, -120.0000000000000000, 2.500000000000000000 ) ) ;
#39917 = CARTESIAN_POINT ( 'NONE',  ( -10.00000000000000000, 0.000000000000000000, 0.000000000000000000 ) ) ;
#39918 = ORIENTED_EDGE ( 'NONE', *, *, #43427, .F. ) ;
#39919 = ORIENTED_EDGE ( 'NONE', *, *, #29700, .T. ) ;
#39920 = AXIS2_PLACEMENT_3D ( 'NONE', #19651, #816, #35078 ) ;
#39921 = VECTOR ( 'NONE', #11820, 1000.000000000000000 ) ;
#39922 = PLANE ( 'NONE',  #18998 ) ;
#39923 = VECTOR ( 'NONE', #14008, 1000.000000000000000 ) ;
#39924 = AXIS2_PLACEMENT_3D ( 'NONE', #37219, #3688, #14953 ) ;
#39925 = CONTEXT_DEPENDENT_SHAPE_REPRESENTATION ( #46027, #1162 ) ;
#39926 = CARTESIAN_POINT ( 'NONE',  ( 0.000000000000000000, -35.91791733033525702, 68.67312586194982771 ) ) ;
#39927 = ORIENTED_EDGE ( 'NONE', *, *, #1900, .T. ) ;
#39928 = AXIS2_PLACEMENT_3D ( 'NONE', #29140, #2951, #36005 ) ;
#39929 = CIRCLE ( 'NONE', #9410, 32.00000000000000000 ) ;
#39930 = ORIENTED_EDGE ( 'NONE', *, *, #2941, .T. ) ;
#39931 = AXIS2_PLACEMENT_3D ( 'NONE', #6791, #13892, #35911 ) ;
#39932 = CARTESIAN_POINT ( 'NONE',  ( 5.000000000000002665, -16.65972982744877484, -80.28980883073775487 ) ) ;
#39933 = ORIENTED_EDGE ( 'NONE', *, *, #12074, .T. ) ;
#39934 = DIRECTION ( 'NONE',  ( 1.000000000000000000, 0.000000000000000000, 0.000000000000000000 ) ) ;
#39935 = EDGE_LOOP ( 'NONE', ( #10965, #9428, #3868, #41455 ) ) ;
#39936 = CARTESIAN_POINT ( 'NONE',  ( 10.00000000000000000, 21.53537804866126137, -30.80686688396986028 ) ) ;
#39937 = EDGE_CURVE ( 'NONE', #7735, #1412, #26867, .T. ) ;
#39938 = ORIENTED_EDGE ( 'NONE', *, *, #44436, .T. ) ;
#39939 = CARTESIAN_POINT ( 'NONE',  ( 10.00000000000000000, 31.46837873495072913, -68.27212725128242710 ) ) ;
#39940 = CARTESIAN_POINT ( 'NONE',  ( -48.80839716909612491, -10.37454508288793065, -5.500000000000000000 ) ) ;
#39941 = EDGE_LOOP ( 'NONE', ( #32669, #38871, #1765, #18131 ) ) ;
#39942 = DIRECTION ( 'NONE',  ( 0.000000000000000000, -0.8526401643540859610, -0.5224985647159591240 ) ) ;
#39943 = EDGE_CURVE ( 'NONE', #10918, #1493, #25273, .T. ) ;
#39944 = ORIENTED_EDGE ( 'NONE', *, *, #13158, .F. ) ;
#39945 = ORIENTED_EDGE ( 'NONE', *, *, #12231, .F. ) ;
#39946 = DIRECTION ( 'NONE',  ( 0.000000000000000000, 0.000000000000000000, -1.000000000000000000 ) ) ;
#39947 = EDGE_CURVE ( 'NONE', #4851, #38433, #39383, .T. ) ;
#39948 = DIRECTION ( 'NONE',  ( 1.000000000000000000, 0.000000000000000000, 0.000000000000000000 ) ) ;
#39949 = DIRECTION ( 'NONE',  ( 0.000000000000000000, -0.7431448254773954654, -0.6691306063588569053 ) ) ;
#39950 = AXIS2_PLACEMENT_3D ( 'NONE', #25249, #5967, #35573 ) ;
#39952 = ORIENTED_EDGE ( 'NONE', *, *, #4805, .T. ) ;
#39951 = DIRECTION ( 'NONE',  ( -1.000000000000000000, 0.000000000000000000, -0.000000000000000000 ) ) ;
#39953 = DIRECTION ( 'NONE',  ( 0.000000000000000000, 0.5877852522924742473, -0.8090169943749466741 ) ) ;
#39954 = VERTEX_POINT ( 'NONE', #952 ) ;
#39955 = AXIS2_PLACEMENT_3D ( 'NONE', #10195, #33438, #48361 ) ;
#39956 = CARTESIAN_POINT ( 'NONE',  ( 10.00000000000000000, 22.48208911017500355, 35.47612816024531668 ) ) ;
#39957 = VERTEX_POINT ( 'NONE', #23003 ) ;
#39958 = ORIENTED_EDGE ( 'NONE', *, *, #35603, .F. ) ;
#39959 = FACE_OUTER_BOUND ( 'NONE', #36289, .T. ) ;
#39960 = FACE_OUTER_BOUND ( 'NONE', #24945, .T. ) ;
#39961 = AXIS2_PLACEMENT_3D ( 'NONE', #9069, #23746, #982 ) ;
#39962 = EDGE_LOOP ( 'NONE', ( #1629, #16558, #7040, #18109 ) ) ;
#39963 = AXIS2_PLACEMENT_3D ( 'NONE', #12257, #27179, #23492 ) ;
#39964 = FACE_OUTER_BOUND ( 'NONE', #37201, .T. ) ;
#39965 = LINE ( 'NONE', #28457, #26617 ) ;
#39966 = CARTESIAN_POINT ( 'NONE',  ( 10.00000000000000000, -27.13269053701114331, 25.88420570971391754 ) ) ;
#39967 = ORIENTED_EDGE ( 'NONE', *, *, #1344, .F. ) ;
#39968 = DIRECTION ( 'NONE',  ( -0.4279312458752990711, -0.9038112904824846527, 0.000000000000000000 ) ) ;
#39969 = EDGE_CURVE ( 'NONE', #28791, #41996, #722, .T. ) ;
#39970 = CYLINDRICAL_SURFACE ( 'NONE', #35886, 32.00000000000000000 ) ;
#39971 = VECTOR ( 'NONE', #30559, 1000.000000000000000 ) ;
#39972 = EDGE_CURVE ( 'NONE', #26898, #14427, #41862, .T. ) ;
#39973 = EDGE_CURVE ( 'NONE', #18975, #3694, #12024, .T. ) ;
#39974 = FACE_OUTER_BOUND ( 'NONE', #19452, .T. ) ;
#39975 = AXIS2_PLACEMENT_3D ( 'NONE', #31368, #46283, #1990 ) ;
#39976 = DIRECTION ( 'NONE',  ( 0.000000000000000000, -0.7071067811865536790, 0.7071067811865414665 ) ) ;
#39977 = ORIENTED_EDGE ( 'NONE', *, *, #38291, .F. ) ;
#39978 = FACE_OUTER_BOUND ( 'NONE', #6276, .T. ) ;
#39979 = CARTESIAN_POINT ( 'NONE',  ( 10.00000000000000000, 0.000000000000000000, 0.000000000000000000 ) ) ;
#39980 = DIRECTION ( 'NONE',  ( -1.000000000000000000, -0.000000000000000000, -0.000000000000000000 ) ) ;
#39981 = CARTESIAN_POINT ( 'NONE',  ( 12.50000000000000000, -107.5000000000000000, -40.00000000000000000 ) ) ;
#39982 = ADVANCED_FACE ( 'NONE', ( #7594 ), #34484, .T. ) ;
#39983 = DIRECTION ( 'NONE',  ( -1.000000000000000000, 0.000000000000000000, -0.000000000000000000 ) ) ;
#39984 = LINE ( 'NONE', #47325, #26126 ) ;
#39985 = ORIENTED_EDGE ( 'NONE', *, *, #10236, .F. ) ;
#39986 = CARTESIAN_POINT ( 'NONE',  ( 0.000000000000000000, 0.000000000000000000, 53.20000000000001705 ) ) ;
#39987 = EDGE_LOOP ( 'NONE', ( #32016, #26357, #7110, #32382 ) ) ;
#39988 = LINE ( 'NONE', #14030, #40961 ) ;
#39989 = DIRECTION ( 'NONE',  ( 0.000000000000000000, -0.8090169943749531134, 0.5877852522924653655 ) ) ;
#39990 = ORIENTED_EDGE ( 'NONE', *, *, #17977, .T. ) ;
#39991 = VECTOR ( 'NONE', #38107, 1000.000000000000000 ) ;
#39992 = AXIS2_PLACEMENT_3D ( 'NONE', #37349, #15080, #30010 ) ;
#39993 = AXIS2_PLACEMENT_3D ( 'NONE', #5090, #35171, #5565 ) ;
#39994 = DIRECTION ( 'NONE',  ( 0.000000000000000000, 0.000000000000000000, 1.000000000000000000 ) ) ;
#39995 = ORIENTED_EDGE ( 'NONE', *, *, #26918, .F. ) ;
#39996 = AXIS2_PLACEMENT_3D ( 'NONE', #16069, #8469, #23393 ) ;
#39997 = EDGE_CURVE ( 'NONE', #7892, #10144, #3675, .T. ) ;
#39998 = ADVANCED_FACE ( 'NONE', ( #22754 ), #227, .T. ) ;
#39999 = LINE ( 'NONE', #40705, #44813 ) ;
#40000 = VERTEX_POINT ( 'NONE', #34010 ) ;
#40001 = PLANE ( 'NONE',  #32800 ) ;
#40002 = DIRECTION ( 'NONE',  ( -1.000000000000000000, 0.000000000000000000, 0.000000000000000000 ) ) ;
#40003 = VECTOR ( 'NONE', #40187, 1000.000000000000114 ) ;
#40004 = EDGE_CURVE ( 'NONE', #17292, #6288, #494, .T. ) ;
#40005 = ORIENTED_EDGE ( 'NONE', *, *, #30133, .F. ) ;
#40006 = CARTESIAN_POINT ( 'NONE',  ( 11.99999999999999822, -76.41127070299280888, 12.93880638057290788 ) ) ;
#40007 = ADVANCED_FACE ( 'NONE', ( #45277 ), #27532, .F. ) ;
#40008 = ORIENTED_EDGE ( 'NONE', *, *, #11608, .F. ) ;
#40009 = CARTESIAN_POINT ( 'NONE',  ( 15.00000000000000000, -19.89357724625003598, -12.59942793731059041 ) ) ;
#40010 = CARTESIAN_POINT ( 'NONE',  ( 15.00000000000000000, -18.13022148937263012, -15.02647892043543898 ) ) ;
#40011 = DIRECTION ( 'NONE',  ( -1.000000000000000000, -0.000000000000000000, -0.000000000000000000 ) ) ;
#40012 = EDGE_LOOP ( 'NONE', ( #40601, #4731, #16924, #11035 ) ) ;
#40013 = LINE ( 'NONE', #19637, #16968 ) ;
#40014 = EDGE_LOOP ( 'NONE', ( #35191, #6886, #44256, #36376 ) ) ;
#40015 = VERTEX_POINT ( 'NONE', #31458 ) ;
#40016 = LINE ( 'NONE', #25069, #5915 ) ;
#40017 = LINE ( 'NONE', #48075, #46528 ) ;
#40018 = DIRECTION ( 'NONE',  ( 0.000000000000000000, 0.000000000000000000, 1.000000000000000000 ) ) ;
#40019 = LINE ( 'NONE', #40269, #39220 ) ;
#40020 = LINE ( 'NONE', #13842, #16718 ) ;
#40021 = DIRECTION ( 'NONE',  ( 0.000000000000000000, 0.5877852522924742473, -0.8090169943749466741 ) ) ;
#40022 = ADVANCED_FACE ( 'NONE', ( #47093 ), #1586, .F. ) ;
#40023 = CARTESIAN_POINT ( 'NONE',  ( 0.000000000000000000, -75.11764819372145041, -2.946379043147127064 ) ) ;
#40024 = DIRECTION ( 'NONE',  ( 0.000000000000000000, 0.1564344650402242631, 0.9876883405951387696 ) ) ;
#40025 = CARTESIAN_POINT ( 'NONE',  ( 10.00000000000000000, -77.32052557432845674, 5.256550761632577284 ) ) ;
#40026 = CARTESIAN_POINT ( 'NONE',  ( 0.000000000000000000, 0.6853352020790449695, 37.58145647212454321 ) ) ;
#40027 = VERTEX_POINT ( 'NONE', #34870 ) ;
#40028 = VECTOR ( 'NONE', #47810, 1000.000000000000000 ) ;
#40029 = ORIENTED_EDGE ( 'NONE', *, *, #29500, .F. ) ;
#40030 = CARTESIAN_POINT ( 'NONE',  ( 0.000000000000000000, 22.64427369931169309, 30.00120703465213623 ) ) ;
#40031 = AXIS2_PLACEMENT_3D ( 'NONE', #33318, #13764, #12023 ) ;
#40032 = DIRECTION ( 'NONE',  ( -1.000000000000000000, 0.000000000000000000, 0.000000000000000000 ) ) ;
#40033 = DIRECTION ( 'NONE',  ( -1.000000000000000000, 0.000000000000000000, 0.000000000000000000 ) ) ;
#40034 = VECTOR ( 'NONE', #9146, 1000.000000000000000 ) ;
#40035 = CIRCLE ( 'NONE', #37683, 31.99999999999999289 ) ;
#40036 = CARTESIAN_POINT ( 'NONE',  ( 11.99999999999999822, -18.89407956138310496, 75.16055320797023853 ) ) ;
#40037 = ADVANCED_FACE ( 'NONE', ( #43182 ), #46859, .F. ) ;
#40038 = DIRECTION ( 'NONE',  ( -1.000000000000000000, -0.000000000000000000, -0.000000000000000000 ) ) ;
#40039 = DIRECTION ( 'NONE',  ( -1.000000000000000000, 0.000000000000000000, 0.000000000000000000 ) ) ;
#40040 = ORIENTED_EDGE ( 'NONE', *, *, #47311, .T. ) ;
#40041 = CARTESIAN_POINT ( 'NONE',  ( 10.00000000000000000, -40.98264845739743834, -9.188173127307738497 ) ) ;
#40042 = CIRCLE ( 'NONE', #36116, 31.99999999999998579 ) ;
#40043 = VERTEX_POINT ( 'NONE', #39529 ) ;
#40044 = CARTESIAN_POINT ( 'NONE',  ( 11.99999999999999822, -66.50666863321974631, -39.78640506895675344 ) ) ;
#40045 = EDGE_LOOP ( 'NONE', ( #31743, #2777, #1931, #30312 ) ) ;
#40046 = ORIENTED_EDGE ( 'NONE', *, *, #3914, .T. ) ;
#40047 = ORIENTED_EDGE ( 'NONE', *, *, #20633, .T. ) ;
#40048 = DIRECTION ( 'NONE',  ( -1.000000000000000000, 0.000000000000000000, 0.000000000000000000 ) ) ;
#40049 = ORIENTED_EDGE ( 'NONE', *, *, #30411, .F. ) ;
#40050 = ORIENTED_EDGE ( 'NONE', *, *, #32488, .T. ) ;
#40051 = AXIS2_PLACEMENT_3D ( 'NONE', #35381, #34904, #31747 ) ;
#40052 = EDGE_CURVE ( 'NONE', #2104, #18905, #10438, .T. ) ;
#40053 = CARTESIAN_POINT ( 'NONE',  ( 11.99999999999999822, -46.53671651293907274, -59.03961581697448935 ) ) ;
#40054 = VECTOR ( 'NONE', #44030, 1000.000000000000000 ) ;
#40055 = CARTESIAN_POINT ( 'NONE',  ( 0.000000000000000000, 12.93880638057315302, 76.41127070299275204 ) ) ;
#40056 = EDGE_CURVE ( 'NONE', #30905, #28317, #28022, .T. ) ;
#40057 = VERTEX_POINT ( 'NONE', #42711 ) ;
#40058 = LINE ( 'NONE', #25111, #41424 ) ;
#40059 = ORIENTED_EDGE ( 'NONE', *, *, #45510, .F. ) ;
#40060 = ORIENTED_EDGE ( 'NONE', *, *, #15599, .F. ) ;
#40061 = EDGE_CURVE ( 'NONE', #18610, #17380, #1828, .T. ) ;
#40062 = CIRCLE ( 'NONE', #18938, 32.00000000000000000 ) ;
#40063 = DIRECTION ( 'NONE',  ( -1.000000000000000000, 0.000000000000000000, -0.000000000000000000 ) ) ;
#40065 = VERTEX_POINT ( 'NONE', #31946 ) ;
#40064 = DIRECTION ( 'NONE',  ( 0.000000000000000000, 0.9876883405951371042, 0.1564344650402346437 ) ) ;
#40066 = DIRECTION ( 'NONE',  ( -1.000000000000000000, -0.000000000000000000, 0.000000000000000000 ) ) ;
#40067 = ORIENTED_EDGE ( 'NONE', *, *, #35683, .F. ) ;
#40068 = VERTEX_POINT ( 'NONE', #38806 ) ;
#40069 = FACE_OUTER_BOUND ( 'NONE', #47585, .T. ) ;
#40070 = ORIENTED_EDGE ( 'NONE', *, *, #43663, .F. ) ;
#40071 = DIRECTION ( 'NONE',  ( -1.000000000000000000, 0.000000000000000000, 0.000000000000000000 ) ) ;
#40072 = CIRCLE ( 'NONE', #35380, 82.00000000000000000 ) ;
#40073 = DIRECTION ( 'NONE',  ( 0.000000000000000000, 0.5877852522924685852, 0.8090169943749507819 ) ) ;
#40074 = ORIENTED_EDGE ( 'NONE', *, *, #21864, .T. ) ;
#40075 = DIRECTION ( 'NONE',  ( 0.000000000000000000, 0.000000000000000000, 1.000000000000000000 ) ) ;
#40076 = CARTESIAN_POINT ( 'NONE',  ( 0.000000000000000000, 0.000000000000000000, 0.000000000000000000 ) ) ;
#40077 = EDGE_CURVE ( 'NONE', #20184, #7124, #31713, .T. ) ;
#40078 = EDGE_CURVE ( 'NONE', #46205, #45324, #13325, .T. ) ;
#40079 = PRESENTATION_STYLE_ASSIGNMENT (( #28814 ) ) ;
#40080 = CARTESIAN_POINT ( 'NONE',  ( 10.00000000000000000, 21.53537804866081373, 30.80686688397018358 ) ) ;
#40081 = VERTEX_POINT ( 'NONE', #24586 ) ;
#40082 = ADVANCED_FACE ( 'NONE', ( #13089 ), #20664, .F. ) ;
#40083 = FACE_OUTER_BOUND ( 'NONE', #22683, .T. ) ;
#40084 = ORIENTED_EDGE ( 'NONE', *, *, #7125, .F. ) ;
#40085 = CARTESIAN_POINT ( 'NONE',  ( 10.00000000000000000, -12.42422080174614862, -35.38097989696524337 ) ) ;
#40086 = FACE_OUTER_BOUND ( 'NONE', #47001, .T. ) ;
#40087 = VECTOR ( 'NONE', #44133, 1000.000000000000114 ) ;
#40088 = CYLINDRICAL_SURFACE ( 'NONE', #15887, 31.99999999999998579 ) ;
#40089 = CARTESIAN_POINT ( 'NONE',  ( 22.94323693612312809, -114.6983135802921083, 5.500000000000000000 ) ) ;
#40091 = CIRCLE ( 'NONE', #40848, 32.00000000000000000 ) ;
#40090 = CARTESIAN_POINT ( 'NONE',  ( 6.000000000000000000, 74.18225833017937987, -34.94270380257559339 ) ) ;
#40092 = EDGE_CURVE ( 'NONE', #42537, #14617, #29203, .T. ) ;
#40094 = EDGE_LOOP ( 'NONE', ( #32277, #1785, #33862, #13946 ) ) ;
#40093 = AXIS2_PLACEMENT_3D ( 'NONE', #14002, #1607, #28921 ) ;
#40095 = DIRECTION ( 'NONE',  ( -1.000000000000000000, 0.000000000000000000, 0.000000000000000000 ) ) ;
#40096 = CARTESIAN_POINT ( 'NONE',  ( 11.99999999999999822, 3.894527615417885169, 81.90746397400390322 ) ) ;
#40097 = DIRECTION ( 'NONE',  ( -1.000000000000000000, 0.000000000000000000, 0.000000000000000000 ) ) ;
#40098 = APPLICATION_CONTEXT ( 'automotive_design' ) ;
#40099 = AXIS2_PLACEMENT_3D ( 'NONE', #14901, #22492, #26644 ) ;
#40100 = AXIS2_PLACEMENT_3D ( 'NONE', #19756, #26162, #34697 ) ;
#40101 = DIRECTION ( 'NONE',  ( -0.000000000000000000, 0.1045284632676569680, 0.9945218953682730678 ) ) ;
#40102 = VECTOR ( 'NONE', #8298, 1000.000000000000227 ) ;
#40103 = EDGE_LOOP ( 'NONE', ( #23674, #43857, #23259, #30751 ) ) ;
#40104 = VERTEX_POINT ( 'NONE', #5267 ) ;
#40105 = AXIS2_PLACEMENT_3D ( 'NONE', #14311, #3532, #36578 ) ;
#40106 = VERTEX_POINT ( 'NONE', #42947 ) ;
#40107 = AXIS2_PLACEMENT_3D ( 'NONE', #12591, #41484, #30970 ) ;
#40108 = DIRECTION ( 'NONE',  ( -1.000000000000000000, -0.000000000000000000, 0.000000000000000000 ) ) ;
#40109 = LINE ( 'NONE', #6570, #26131 ) ;
#40110 = ORIENTED_EDGE ( 'NONE', *, *, #8115, .T. ) ;
#40111 = CARTESIAN_POINT ( 'NONE',  ( 11.99999999999999822, 0.000000000000000000, 0.000000000000000000 ) ) ;
#40112 = EDGE_CURVE ( 'NONE', #31521, #10773, #20181, .T. ) ;
#40113 = ORIENTED_EDGE ( 'NONE', *, *, #37069, .T. ) ;
#40114 = ORIENTED_EDGE ( 'NONE', *, *, #35704, .F. ) ;
#40115 = ORIENTED_EDGE ( 'NONE', *, *, #13963, .F. ) ;
#40116 = AXIS2_PLACEMENT_3D ( 'NONE', #40878, #14459, #45276 ) ;
#40117 = EDGE_CURVE ( 'NONE', #23147, #40294, #35602, .T. ) ;
#40118 = EDGE_CURVE ( 'NONE', #11188, #8273, #13554, .T. ) ;
#40119 = AXIS2_PLACEMENT_3D ( 'NONE', #27952, #5187, #45824 ) ;
#40120 = ADVANCED_FACE ( 'NONE', ( #24821 ), #5015, .T. ) ;
#40121 = CARTESIAN_POINT ( 'NONE',  ( 10.00000000000000000, 3.925862922256160736, 41.81611651403863306 ) ) ;
#40122 = EDGE_CURVE ( 'NONE', #17270, #27718, #37802, .T. ) ;
#40123 = ORIENTED_EDGE ( 'NONE', *, *, #31252, .F. ) ;
#40124 = DIRECTION ( 'NONE',  ( -1.000000000000000000, -0.000000000000000000, -0.000000000000000000 ) ) ;
#40125 = ADVANCED_FACE ( 'NONE', ( #5495 ), #21634, .T. ) ;
#40126 = VERTEX_POINT ( 'NONE', #43665 ) ;
#40127 = DIRECTION ( 'NONE',  ( 0.000000000000000000, 0.9723699203976756689, 0.2334453638559093047 ) ) ;
#40128 = CIRCLE ( 'NONE', #17437, 32.00000000000000000 ) ;
#40129 = CIRCLE ( 'NONE', #2583, 77.49899999999999523 ) ;
#40130 = FACE_OUTER_BOUND ( 'NONE', #22724, .T. ) ;
#40131 = LINE ( 'NONE', #47230, #9569 ) ;
#40132 = AXIS2_PLACEMENT_3D ( 'NONE', #36108, #10162, #6262 ) ;
#40133 = DIRECTION ( 'NONE',  ( -0.08130631524010117905, 0.9966891607226784355, 0.000000000000000000 ) ) ;
#40134 = EDGE_LOOP ( 'NONE', ( #5350, #33194, #14613, #47340 ) ) ;
#40135 = DIRECTION ( 'NONE',  ( -1.000000000000000000, -0.000000000000000000, 0.000000000000000000 ) ) ;
#40136 = DIRECTION ( 'NONE',  ( 0.000000000000000000, 0.000000000000000000, 1.000000000000000000 ) ) ;
#40137 = AXIS2_PLACEMENT_3D ( 'NONE', #20653, #5490, #24815 ) ;
#40138 = VECTOR ( 'NONE', #13596, 1000.000000000000000 ) ;
#40139 = ORIENTED_EDGE ( 'NONE', *, *, #33329, .T. ) ;
#40140 = EDGE_LOOP ( 'NONE', ( #35170, #23827, #28364, #4016 ) ) ;
#40141 = ADVANCED_FACE ( 'NONE', ( #33370 ), #48053, .T. ) ;
#40142 = DIRECTION ( 'NONE',  ( 0.000000000000000000, 0.000000000000000000, 1.000000000000000000 ) ) ;
#40143 = DIRECTION ( 'NONE',  ( -1.000000000000000000, -0.000000000000000000, -0.000000000000000000 ) ) ;
#40144 = ORIENTED_EDGE ( 'NONE', *, *, #8189, .F. ) ;
#40145 = VERTEX_POINT ( 'NONE', #48292 ) ;
#40146 = CIRCLE ( 'NONE', #26862, 42.00000000000000000 ) ;
#40147 = LINE ( 'NONE', #36462, #26921 ) ;
#40148 = DIRECTION ( 'NONE',  ( 0.5687579148473744795, -0.8225049752423790883, 0.000000000000000000 ) ) ;
#40149 = PLANE ( 'NONE',  #12018 ) ;
#40150 = FACE_OUTER_BOUND ( 'NONE', #47333, .T. ) ;
#40151 = VECTOR ( 'NONE', #43437, 1000.000000000000000 ) ;
#40152 = DIRECTION ( 'NONE',  ( -1.000000000000000000, 0.000000000000000000, 0.000000000000000000 ) ) ;
#40153 = EDGE_CURVE ( 'NONE', #13467, #15723, #15930, .T. ) ;
#40154 = VERTEX_POINT ( 'NONE', #44387 ) ;
#40155 = DIRECTION ( 'NONE',  ( 0.000000000000000000, 0.000000000000000000, -1.000000000000000000 ) ) ;
#40156 = PLANE ( 'NONE',  #18372 ) ;
#40157 = DIRECTION ( 'NONE',  ( 0.000000000000000000, 0.000000000000000000, 1.000000000000000000 ) ) ;
#40158 = CYLINDRICAL_SURFACE ( 'NONE', #38681, 77.49899999999999523 ) ;
#40159 = CARTESIAN_POINT ( 'NONE',  ( 10.00000000000000000, -6.736453364083817341, 36.88895765772630142 ) ) ;
#40160 = ORIENTED_EDGE ( 'NONE', *, *, #6098, .F. ) ;
#40161 = ORIENTED_EDGE ( 'NONE', *, *, #3815, .F. ) ;
#40162 = VERTEX_POINT ( 'NONE', #14774 ) ;
#40163 = ADVANCED_FACE ( 'NONE', ( #25047 ), #38578, .F. ) ;
#40164 = CYLINDRICAL_SURFACE ( 'NONE', #35428, 82.00000000000000000 ) ;
#40165 = AXIS2_PLACEMENT_3D ( 'NONE', #34836, #35076, #1556 ) ;
#40166 = CIRCLE ( 'NONE', #7342, 20.99999999999999645 ) ;
#40167 = AXIS2_PLACEMENT_3D ( 'NONE', #32981, #25634, #26133 ) ;
#40168 = CYLINDRICAL_SURFACE ( 'NONE', #18292, 77.49899999999999523 ) ;
#40169 = ORIENTED_EDGE ( 'NONE', *, *, #41835, .F. ) ;
#40170 = EDGE_CURVE ( 'NONE', #34957, #9900, #43249, .T. ) ;
#40171 = VECTOR ( 'NONE', #40176, 1000.000000000000000 ) ;
#40172 = AXIS2_PLACEMENT_3D ( 'NONE', #44367, #3231, #18421 ) ;
#40173 = EDGE_CURVE ( 'NONE', #6771, #35343, #28399, .T. ) ;
#40174 = CARTESIAN_POINT ( 'NONE',  ( 4.999999999999999112, -41.81611651403859042, -3.925862922256606602 ) ) ;
#40175 = VECTOR ( 'NONE', #25692, 1000.000000000000000 ) ;
#40176 = DIRECTION ( 'NONE',  ( -1.000000000000000000, 0.000000000000000000, 0.000000000000000000 ) ) ;
#40177 = VERTEX_POINT ( 'NONE', #3015 ) ;
#40179 = EDGE_CURVE ( 'NONE', #44958, #14299, #47159, .T. ) ;
#40178 = DIRECTION ( 'NONE',  ( -1.000000000000000000, -0.000000000000000000, 0.000000000000000000 ) ) ;
#40180 = AXIS2_PLACEMENT_3D ( 'NONE', #30196, #45116, #22359 ) ;
#40181 = EDGE_CURVE ( 'NONE', #14655, #19593, #39999, .T. ) ;
#40182 = EDGE_LOOP ( 'NONE', ( #21570, #17082, #20245, #21660 ) ) ;
#40183 = DIRECTION ( 'NONE',  ( 0.000000000000000000, 0.000000000000000000, 1.000000000000000000 ) ) ;
#40184 = ADVANCED_FACE ( 'NONE', ( #47562 ), #43901, .T. ) ;
#40185 = FACE_OUTER_BOUND ( 'NONE', #15458, .T. ) ;
#40186 = ORIENTED_EDGE ( 'NONE', *, *, #41925, .T. ) ;
#40187 = DIRECTION ( 'NONE',  ( -0.000000000000000000, 0.4999999999999921174, -0.8660254037844432595 ) ) ;
#40188 = VERTEX_POINT ( 'NONE', #17940 ) ;
#40189 = CARTESIAN_POINT ( 'NONE',  ( -10.00000000000000000, 0.000000000000000000, 0.000000000000000000 ) ) ;
#40190 = ORIENTED_EDGE ( 'NONE', *, *, #5426, .F. ) ;
#40191 = DIRECTION ( 'NONE',  ( 0.6691306063588569053, 0.7431448254773954654, 0.000000000000000000 ) ) ;
#40192 = CARTESIAN_POINT ( 'NONE',  ( -3.000000000000000000, 16.61724383029390140, -20.69703378468903665 ) ) ;
#40193 = CARTESIAN_POINT ( 'NONE',  ( 21.07894319797337346, -103.8699611390234878, 2.500000000000000000 ) ) ;
#40194 = CIRCLE ( 'NONE', #306, 37.49900000000000233 ) ;
#40195 = DIRECTION ( 'NONE',  ( -1.000000000000000000, -0.000000000000000000, -0.000000000000000000 ) ) ;
#40196 = CIRCLE ( 'NONE', #34684, 82.00000000000000000 ) ;
#40197 = CARTESIAN_POINT ( 'NONE',  ( 10.00000000000000000, 72.35160999960844208, -20.41045688087747223 ) ) ;
#40198 = ORIENTED_EDGE ( 'NONE', *, *, #6328, .T. ) ;
#40199 = DIRECTION ( 'NONE',  ( 0.000000000000000000, 0.000000000000000000, 1.000000000000000000 ) ) ;
#40200 = ORIENTED_EDGE ( 'NONE', *, *, #7571, .F. ) ;
#40201 = ORIENTED_EDGE ( 'NONE', *, *, #17633, .T. ) ;
#40202 = CARTESIAN_POINT ( 'NONE',  ( -3.000000000000000000, 16.83928648764945279, -16.46020748918028076 ) ) ;
#40203 = CIRCLE ( 'NONE', #32375, 77.49899999999999523 ) ;
#40204 = LINE ( 'NONE', #47755, #16810 ) ;
#40205 = AXIS2_PLACEMENT_3D ( 'NONE', #40517, #33169, #26062 ) ;
#40206 = LINE ( 'NONE', #40924, #11265 ) ;
#40207 = LINE ( 'NONE', #47307, #23491 ) ;
#40208 = DIRECTION ( 'NONE',  ( -0.08130631524009862554, 0.9966891607226787686, 0.000000000000000000 ) ) ;
#40209 = EDGE_LOOP ( 'NONE', ( #27500, #669, #44400, #8235 ) ) ;
#40210 = AXIS2_PLACEMENT_3D ( 'NONE', #2036, #43846, #24531 ) ;
#40211 = PRODUCT ( 'Sliding Dog Clutch Collar', 'Sliding Dog Clutch Collar', '', ( #46303 ) ) ;
#40212 = DIRECTION ( 'NONE',  ( 1.000000000000000000, -0.000000000000000000, -0.000000000000000000 ) ) ;
#40213 = CARTESIAN_POINT ( 'NONE',  ( -0.7800914985199643992, -121.2811936832255100, 2.500000000000000000 ) ) ;
#40214 = DIRECTION ( 'NONE',  ( -1.000000000000000000, 0.000000000000000000, 0.000000000000000000 ) ) ;
#40215 = VERTEX_POINT ( 'NONE', #17462 ) ;
#40216 = AXIS2_PLACEMENT_3D ( 'NONE', #7363, #23922, #33773 ) ;
#40217 = AXIS2_PLACEMENT_3D ( 'NONE', #17376, #32327, #47257 ) ;
#40218 = DIRECTION ( 'NONE',  ( 0.000000000000000000, 0.000000000000000000, 1.000000000000000000 ) ) ;
#40219 = CARTESIAN_POINT ( 'NONE',  ( 10.00000000000000000, -49.70050353004846500, -59.46389618802017907 ) ) ;
#40220 = CARTESIAN_POINT ( 'NONE',  ( 10.00000000000000000, -24.73286445877757345, 73.44644590900053061 ) ) ;
#40222 = AXIS2_PLACEMENT_3D ( 'NONE', #45748, #24190, #43750 ) ;
#40221 = CARTESIAN_POINT ( 'NONE',  ( 0.000000000000000000, 0.000000000000000000, 0.000000000000000000 ) ) ;
#40223 = DIRECTION ( 'NONE',  ( -0.6064928550163533050, -0.7950889364178781449, 0.000000000000000000 ) ) ;
#40224 = CARTESIAN_POINT ( 'NONE',  ( 10.00000000000000000, -8.840884882374576037, -74.65374052328658649 ) ) ;
#40225 = DIRECTION ( 'NONE',  ( -1.000000000000000000, 0.000000000000000000, 0.000000000000000000 ) ) ;
#40226 = CARTESIAN_POINT ( 'NONE',  ( 0.000000000000000000, 0.000000000000000000, 0.000000000000000000 ) ) ;
#40227 = EDGE_LOOP ( 'NONE', ( #14403, #16777, #44983, #27027 ) ) ;
#40228 = ORIENTED_EDGE ( 'NONE', *, *, #48290, .T. ) ;
#40229 = CARTESIAN_POINT ( 'NONE',  ( -10.21100092698785033, -95.54625877152835756, 2.500000000000000000 ) ) ;
#40230 = VERTEX_POINT ( 'NONE', #18179 ) ;
#40231 = CARTESIAN_POINT ( 'NONE',  ( 11.99999999999999822, -23.16143007188376757, -73.95703589263997912 ) ) ;
#40232 =( LENGTH_UNIT ( ) NAMED_UNIT ( * ) SI_UNIT ( .MILLI., .METRE. ) );
#40233 = ORIENTED_EDGE ( 'NONE', *, *, #12711, .F. ) ;
#40234 = FACE_OUTER_BOUND ( 'NONE', #9600, .T. ) ;
#40235 = VERTEX_POINT ( 'NONE', #10130 ) ;
#40236 = AXIS2_PLACEMENT_3D ( 'NONE', #32084, #13468, #35503 ) ;
#40237 = EDGE_CURVE ( 'NONE', #14950, #26390, #29972, .T. ) ;
#40238 = VECTOR ( 'NONE', #18243, 1000.000000000000000 ) ;
#40239 = AXIS2_PLACEMENT_3D ( 'NONE', #42930, #40695, #32857 ) ;
#40240 = FACE_OUTER_BOUND ( 'NONE', #32599, .T. ) ;
#40241 = ORIENTED_EDGE ( 'NONE', *, *, #45523, .F. ) ;
#40242 = EDGE_CURVE ( 'NONE', #18493, #41154, #2527, .T. ) ;
#40243 = EDGE_CURVE ( 'NONE', #28195, #46892, #27641, .T. ) ;
#40244 = AXIS2_PLACEMENT_3D ( 'NONE', #24391, #39330, #24644 ) ;
#40245 = VECTOR ( 'NONE', #40288, 1000.000000000000000 ) ;
#40246 = DIRECTION ( 'NONE',  ( -1.000000000000000000, 0.000000000000000000, 0.000000000000000000 ) ) ;
#40247 = EDGE_LOOP ( 'NONE', ( #44756, #43772, #42813, #47551 ) ) ;
#40248 = AXIS2_PLACEMENT_3D ( 'NONE', #34903, #35815, #9613 ) ;
#40249 = EDGE_CURVE ( 'NONE', #27199, #38067, #37034, .T. ) ;
#40250 = CARTESIAN_POINT ( 'NONE',  ( 5.999999999999999112, 67.80270845531956070, -46.11716303203111522 ) ) ;
#40251 = AXIS2_PLACEMENT_3D ( 'NONE', #31704, #46619, #43178 ) ;
#40252 = FACE_OUTER_BOUND ( 'NONE', #1848, .T. ) ;
#40253 = ORIENTED_EDGE ( 'NONE', *, *, #31577, .T. ) ;
#40254 = DIRECTION ( 'NONE',  ( -1.000000000000000000, 0.000000000000000000, -0.000000000000000000 ) ) ;
#40255 = VECTOR ( 'NONE', #23037, 1000.000000000000000 ) ;
#40256 = EDGE_CURVE ( 'NONE', #38765, #37954, #29458, .T. ) ;
#40257 = ORIENTED_EDGE ( 'NONE', *, *, #46212, .F. ) ;
#40258 = AXIS2_PLACEMENT_3D ( 'NONE', #47823, #47374, #43926 ) ;
#40259 = CARTESIAN_POINT ( 'NONE',  ( 10.00000000000000000, 0.000000000000000000, 0.000000000000000000 ) ) ;
#40260 = DIRECTION ( 'NONE',  ( -1.000000000000000000, -0.000000000000000000, 0.000000000000000000 ) ) ;
#40261 = DIRECTION ( 'NONE',  ( -1.000000000000000000, -0.000000000000000000, 0.000000000000000000 ) ) ;
#40262 = ORIENTED_EDGE ( 'NONE', *, *, #4232, .F. ) ;
#40263 = DIRECTION ( 'NONE',  ( 1.000000000000000000, 0.000000000000000000, 0.000000000000000000 ) ) ;
#40264 = ORIENTED_EDGE ( 'NONE', *, *, #33696, .F. ) ;
#40265 = EDGE_LOOP ( 'NONE', ( #38751, #31535, #5751, #39716, #12029, #45250 ) ) ;
#40266 = CARTESIAN_POINT ( 'NONE',  ( 11.99999999999999822, -73.44644590900077219, 24.73286445877677764 ) ) ;
#40267 = CARTESIAN_POINT ( 'NONE',  ( 10.00000000000000000, -36.73666225445845157, -65.58780272294114866 ) ) ;
#40268 = DIRECTION ( 'NONE',  ( -1.000000000000000000, -0.000000000000000000, 0.000000000000000000 ) ) ;
#40269 = CARTESIAN_POINT ( 'NONE',  ( 5.000000000000000000, 22.48208911017551870, -35.47612816024499693 ) ) ;
#40270 = ORIENTED_EDGE ( 'NONE', *, *, #5732, .T. ) ;
#40271 = FACE_OUTER_BOUND ( 'NONE', #20792, .T. ) ;
#40272 = FACE_OUTER_BOUND ( 'NONE', #1821, .T. ) ;
#40273 = CARTESIAN_POINT ( 'NONE',  ( 0.000000000000000000, 69.42325613327440692, 34.44570377933622041 ) ) ;
#40274 = PLANE ( 'NONE',  #43175 ) ;
#40275 = CARTESIAN_POINT ( 'NONE',  ( 0.000000000000000000, -33.00180498840035170, -17.80606268964575278 ) ) ;
#40276 = ORIENTED_EDGE ( 'NONE', *, *, #34875, .T. ) ;
#40277 = DIRECTION ( 'NONE',  ( 0.000000000000000000, 0.000000000000000000, 1.000000000000000000 ) ) ;
#40278 = AXIS2_PLACEMENT_3D ( 'NONE', #35800, #13523, #28456 ) ;
#40279 = DIRECTION ( 'NONE',  ( -1.000000000000000000, 0.000000000000000000, 0.000000000000000000 ) ) ;
#40280 = DIRECTION ( 'NONE',  ( 0.000000000000000000, 0.9135454576426003115, 0.4067366430758017071 ) ) ;
#40281 = CARTESIAN_POINT ( 'NONE',  ( 10.00000000000000000, -21.53537804866058991, -30.80686688397033635 ) ) ;
#40282 = ADVANCED_FACE ( 'NONE', ( #28738 ), #29211, .F. ) ;
#40283 = AXIS2_PLACEMENT_3D ( 'NONE', #39533, #35105, #16516 ) ;
#40284 = AXIS2_PLACEMENT_3D ( 'NONE', #29694, #14779, #22108 ) ;
#40285 = DIRECTION ( 'NONE',  ( -1.000000000000000000, 0.000000000000000000, 0.000000000000000000 ) ) ;
#40286 = DIRECTION ( 'NONE',  ( 0.000000000000000000, 0.9135454576426010886, -0.4067366430757998752 ) ) ;
#40287 = VERTEX_POINT ( 'NONE', #22103 ) ;
#40288 = DIRECTION ( 'NONE',  ( -1.000000000000000000, 0.000000000000000000, 0.000000000000000000 ) ) ;
#40289 = EDGE_CURVE ( 'NONE', #41512, #46575, #27670, .T. ) ;
#40290 = AXIS2_PLACEMENT_3D ( 'NONE', #27326, #12880, #4564 ) ;
#40291 = ADVANCED_FACE ( 'NONE', ( #18902 ), #41439, .F. ) ;
#40292 = CARTESIAN_POINT ( 'NONE',  ( 0.000000000000000000, -0.8299999999999999600, -1.199999999999999956 ) ) ;
#40293 = VECTOR ( 'NONE', #21156, 1000.000000000000000 ) ;
#40294 = VERTEX_POINT ( 'NONE', #34552 ) ;
#40295 = EDGE_LOOP ( 'NONE', ( #17153, #16997, #18656, #25771 ) ) ;
#40296 = ORIENTED_EDGE ( 'NONE', *, *, #30016, .F. ) ;
#40297 = VECTOR ( 'NONE', #43411, 1000.000000000000000 ) ;
#40298 = EDGE_LOOP ( 'NONE', ( #25730, #44512, #34981, #6820 ) ) ;
#40299 = CIRCLE ( 'NONE', #9777, 82.00000000000000000 ) ;
#40300 = DIRECTION ( 'NONE',  ( 1.000000000000000000, -0.000000000000000000, -0.000000000000000000 ) ) ;
#40301 = EDGE_CURVE ( 'NONE', #12455, #9769, #24568, .T. ) ;
#40302 = ORIENTED_EDGE ( 'NONE', *, *, #47145, .F. ) ;
#40303 = EDGE_CURVE ( 'NONE', #19987, #6884, #38250, .T. ) ;
#40304 = EDGE_CURVE ( 'NONE', #29847, #41768, #308, .T. ) ;
#40305 = ORIENTED_EDGE ( 'NONE', *, *, #7021, .F. ) ;
#40306 = AXIS2_PLACEMENT_3D ( 'NONE', #5972, #1802, #46837 ) ;
#40307 = DIRECTION ( 'NONE',  ( 0.000000000000000000, 0.9135454576426063067, -0.4067366430757881068 ) ) ;
#40308 = CYLINDRICAL_SURFACE ( 'NONE', #46877, 16.00000000000000000 ) ;
#40309 = DIRECTION ( 'NONE',  ( -1.000000000000000000, 0.000000000000000000, 0.000000000000000000 ) ) ;
#40310 = ORIENTED_EDGE ( 'NONE', *, *, #39061, .F. ) ;
#40311 = DIRECTION ( 'NONE',  ( -0.5687579148473752566, 0.8225049752423786442, 0.000000000000000000 ) ) ;
#40312 = ORIENTED_EDGE ( 'NONE', *, *, #17548, .F. ) ;
#40313 = ORIENTED_EDGE ( 'NONE', *, *, #12334, .T. ) ;
#40314 = ORIENTED_EDGE ( 'NONE', *, *, #6149, .F. ) ;
#40315 = DIRECTION ( 'NONE',  ( 0.000000000000000000, 0.000000000000000000, 1.000000000000000000 ) ) ;
#40316 = EDGE_CURVE ( 'NONE', #42776, #43483, #9699, .T. ) ;
#40318 = ORIENTED_EDGE ( 'NONE', *, *, #23190, .F. ) ;
#40317 = CARTESIAN_POINT ( 'NONE',  ( 0.000000000000000000, 0.000000000000000000, 40.80000000000001847 ) ) ;
#40319 = CARTESIAN_POINT ( 'NONE',  ( 15.00000000000000000, 8.688484142253932063, -21.88630264137371029 ) ) ;
#40320 = CIRCLE ( 'NONE', #19199, 31.99999999999998579 ) ;
#40322 = ORIENTED_EDGE ( 'NONE', *, *, #13723, .F. ) ;
#40321 = AXIS2_PLACEMENT_3D ( 'NONE', #5627, #21259, #36194 ) ;
#40323 = ORIENTED_EDGE ( 'NONE', *, *, #38855, .T. ) ;
#40324 = ORIENTED_EDGE ( 'NONE', *, *, #41446, .T. ) ;
#40325 = LINE ( 'NONE', #25364, #6011 ) ;
#40326 = EDGE_LOOP ( 'NONE', ( #15554, #42997, #21672, #48036 ) ) ;
#40327 = DIRECTION ( 'NONE',  ( -1.000000000000000000, -0.000000000000000000, -0.000000000000000000 ) ) ;
#40328 = AXIS2_PLACEMENT_3D ( 'NONE', #6969, #29962, #94 ) ;
#40329 = CARTESIAN_POINT ( 'NONE',  ( 15.00000000000000000, 9.615535125378766423, -24.73947219025917121 ) ) ;
#40330 = FACE_BOUND ( 'NONE', #4398, .T. ) ;
#40331 = EDGE_LOOP ( 'NONE', ( #34076, #17538, #29931, #12504 ) ) ;
#40332 = CARTESIAN_POINT ( 'NONE',  ( 11.99999999999999822, 0.000000000000000000, 0.000000000000000000 ) ) ;
#40333 = DIRECTION ( 'NONE',  ( -1.000000000000000000, 0.000000000000000000, -0.000000000000000000 ) ) ;
#40334 = VECTOR ( 'NONE', #16955, 1000.000000000000000 ) ;
#40335 = CARTESIAN_POINT ( 'NONE',  ( 0.000000000000000000, -35.92658777277517856, 10.74501242461269257 ) ) ;
#40336 = LINE ( 'NONE', #18268, #22730 ) ;
#40337 = LINE ( 'NONE', #21712, #17300 ) ;
#40338 = ORIENTED_EDGE ( 'NONE', *, *, #40061, .F. ) ;
#40339 = DIRECTION ( 'NONE',  ( 0.000000000000000000, 0.4539904997395413644, 0.8910065241883706744 ) ) ;
#40340 = DIRECTION ( 'NONE',  ( -1.000000000000000000, 0.000000000000000000, -0.000000000000000000 ) ) ;
#40341 = AXIS2_PLACEMENT_3D ( 'NONE', #46147, #27541, #42469 ) ;
#40342 = DIRECTION ( 'NONE',  ( -1.000000000000000000, -0.000000000000000000, 0.000000000000000000 ) ) ;
#40343 = LINE ( 'NONE', #36411, #18208 ) ;
#40344 = CARTESIAN_POINT ( 'NONE',  ( 11.99999999999999822, -81.90746397400386059, -3.894527615418766242 ) ) ;
#40345 = DIRECTION ( 'NONE',  ( 0.000000000000000000, -0.3090169943749551673, -0.9510565162951510887 ) ) ;
#40346 = CONICAL_SURFACE ( 'NONE', #34869, 17.30399999999999849, 0.2094395102393129815 ) ;
#40347 = EDGE_CURVE ( 'NONE', #22027, #38915, #22986, .T. ) ;
#40348 = CARTESIAN_POINT ( 'NONE',  ( 0.000000000000000000, 80.28980883073781172, -16.65972982744850839 ) ) ;
#40349 = CARTESIAN_POINT ( 'NONE',  ( 0.000000000000000000, -59.46389618801999433, 49.70050353004867816 ) ) ;
#40350 = EDGE_CURVE ( 'NONE', #3813, #39835, #42523, .T. ) ;
#40351 = DIRECTION ( 'NONE',  ( -1.000000000000000000, 0.000000000000000000, -0.000000000000000000 ) ) ;
#40352 = AXIS2_PLACEMENT_3D ( 'NONE', #19710, #34647, #45204 ) ;
#40353 = ADVANCED_FACE ( 'NONE', ( #33601 ), #790, .T. ) ;
#40354 = ORIENTED_EDGE ( 'NONE', *, *, #10622, .T. ) ;
#40355 = VERTEX_POINT ( 'NONE', #30425 ) ;
#40356 = AXIS2_PLACEMENT_3D ( 'NONE', #2906, #2194, #13929 ) ;
#40357 = ORIENTED_EDGE ( 'NONE', *, *, #12757, .F. ) ;
#40358 = AXIS2_PLACEMENT_3D ( 'NONE', #14255, #29175, #44114 ) ;
#40359 = DIRECTION ( 'NONE',  ( 0.000000000000000000, -1.000000000000000000, -1.047444401652940007E-14 ) ) ;
#40360 = DIRECTION ( 'NONE',  ( -1.000000000000000000, 0.000000000000000000, -0.000000000000000000 ) ) ;
#40361 = VERTEX_POINT ( 'NONE', #4713 ) ;
#40362 = EDGE_CURVE ( 'NONE', #35973, #36385, #12831, .T. ) ;
#40363 = EDGE_CURVE ( 'NONE', #47876, #8701, #37061, .T. ) ;
#40364 = CLOSED_SHELL ( 'NONE', ( #13492, #16975, #35364, #34016, #6907, #26534, #15704, #39137, #45267, #25686, #3816, #21704, #44257, #15386, #9949, #35850, #17512, #5114 ) ) ;
#40365 = DIRECTION ( 'NONE',  ( 0.000000000000000000, -0.5877852522924624790, -0.8090169943749550008 ) ) ;
#40366 = EDGE_LOOP ( 'NONE', ( #20194, #36013, #6069, #24981 ) ) ;
#40367 = VERTEX_POINT ( 'NONE', #11584 ) ;
#40368 = CIRCLE ( 'NONE', #20020, 42.00000000000000000 ) ;
#40369 = EDGE_CURVE ( 'NONE', #17350, #23067, #7895, .T. ) ;
#40370 = CIRCLE ( 'NONE', #5195, 82.00000000000000000 ) ;
#40371 = CARTESIAN_POINT ( 'NONE',  ( 0.000000000000000000, -70.52718814184277107, 26.02418014898285037 ) ) ;
#40372 = ORIENTED_EDGE ( 'NONE', *, *, #28878, .T. ) ;
#40373 = ORIENTED_EDGE ( 'NONE', *, *, #8183, .F. ) ;
#40374 = DIRECTION ( 'NONE',  ( -1.000000000000000000, -0.000000000000000000, -0.000000000000000000 ) ) ;
#40375 = DIRECTION ( 'NONE',  ( 1.000000000000000000, -0.000000000000000000, 0.000000000000000000 ) ) ;
#40376 = DIRECTION ( 'NONE',  ( -1.000000000000000000, 0.000000000000000000, 0.000000000000000000 ) ) ;
#40377 = CARTESIAN_POINT ( 'NONE',  ( 10.00000000000000000, 14.66109333815460225, 73.73191006444577056 ) ) ;
#40378 = ORIENTED_EDGE ( 'NONE', *, *, #3179, .T. ) ;
#40379 = ORIENTED_EDGE ( 'NONE', *, *, #36623, .F. ) ;
#40380 = DIRECTION ( 'NONE',  ( 0.000000000000000000, 0.000000000000000000, 1.000000000000000000 ) ) ;
#40381 = FACE_OUTER_BOUND ( 'NONE', #18026, .T. ) ;
#40382 = AXIS2_PLACEMENT_3D ( 'NONE', #33488, #48414, #20251 ) ;
#40383 = EDGE_LOOP ( 'NONE', ( #4760, #31349 ) ) ;
#40384 = ORIENTED_EDGE ( 'NONE', *, *, #1034, .T. ) ;
#40385 = DIRECTION ( 'NONE',  ( -1.000000000000000000, 0.000000000000000000, -0.000000000000000000 ) ) ;
#40386 = FACE_OUTER_BOUND ( 'NONE', #1922, .T. ) ;
#40387 = VERTEX_POINT ( 'NONE', #1029 ) ;
#40388 = EDGE_LOOP ( 'NONE', ( #30645, #26449, #6082, #18003 ) ) ;
#40389 = DIRECTION ( 'NONE',  ( 8.090853898039833646E-17, -9.269810975720164453E-17, 1.000000000000000000 ) ) ;
#40390 = AXIS2_PLACEMENT_3D ( 'NONE', #39908, #1741, #16666 ) ;
#40391 = FACE_OUTER_BOUND ( 'NONE', #30917, .T. ) ;
#40392 = FACE_OUTER_BOUND ( 'NONE', #2907, .T. ) ;
#40393 = DIRECTION ( 'NONE',  ( 0.000000000000000000, 0.000000000000000000, 1.000000000000000000 ) ) ;
#40394 = DIRECTION ( 'NONE',  ( -1.000000000000000000, 0.000000000000000000, -0.000000000000000000 ) ) ;
#40395 = VECTOR ( 'NONE', #14573, 1000.000000000000000 ) ;
#40396 = DIRECTION ( 'NONE',  ( 0.6575728627325957421, -0.7533909544171993877, -1.230411769795008318E-16 ) ) ;
#40397 = CARTESIAN_POINT ( 'NONE',  ( 12.00000000000000000, -13.04903810567646971, 19.60159698893442126 ) ) ;
#40398 = EDGE_CURVE ( 'NONE', #39130, #40215, #302, .T. ) ;
#40399 = CARTESIAN_POINT ( 'NONE',  ( 0.000000000000000000, -80.55351364060578589, -15.33399622253570094 ) ) ;
#40400 = CARTESIAN_POINT ( 'NONE',  ( 15.00000000000000000, -0.9646360437372099028, 23.52805723605590771 ) ) ;
#40401 = ADVANCED_FACE ( 'NONE', ( #30659 ), #45579, .F. ) ;
#40402 =( NAMED_UNIT ( * ) PLANE_ANGLE_UNIT ( ) SI_UNIT ( $, .RADIAN. ) );
#40403 = DIRECTION ( 'NONE',  ( -1.000000000000000000, -0.000000000000000000, -0.000000000000000000 ) ) ;
#40404 = EDGE_CURVE ( 'NONE', #44810, #11885, #41679, .T. ) ;
#40405 = ORIENTED_EDGE ( 'NONE', *, *, #1219, .F. ) ;
#40406 = VERTEX_POINT ( 'NONE', #27003 ) ;
#40407 = ORIENTED_EDGE ( 'NONE', *, *, #13322, .F. ) ;
#40408 = AXIS2_PLACEMENT_3D ( 'NONE', #12958, #17089, #8771 ) ;
#40410 = EDGE_CURVE ( 'NONE', #42331, #45054, #15978, .T. ) ;
#40409 = UNCERTAINTY_MEASURE_WITH_UNIT (LENGTH_MEASURE( 1.000000000000000082E-05 ), #16559, 'distance_accuracy_value', 'NONE');
#40411 = FACE_OUTER_BOUND ( 'NONE', #31727, .T. ) ;
#40412 = FACE_OUTER_BOUND ( 'NONE', #20787, .T. ) ;
#40413 = ORIENTED_EDGE ( 'NONE', *, *, #44995, .T. ) ;
#40414 = EDGE_CURVE ( 'NONE', #34957, #15686, #26014, .T. ) ;
#40415 = VERTEX_POINT ( 'NONE', #3746 ) ;
#40416 = AXIS2_PLACEMENT_3D ( 'NONE', #14360, #22433, #7505 ) ;
#40417 = EDGE_CURVE ( 'NONE', #12661, #43656, #6564, .T. ) ;
#40418 = CARTESIAN_POINT ( 'NONE',  ( 10.00000000000000000, 0.000000000000000000, 0.000000000000000000 ) ) ;
#40419 = VERTEX_POINT ( 'NONE', #13269 ) ;
#40420 = CARTESIAN_POINT ( 'NONE',  ( 10.00000000000000000, 55.16347631943041563, 60.67117009219156643 ) ) ;
#40421 = CIRCLE ( 'NONE', #37303, 31.99999999999999645 ) ;
#40422 = ORIENTED_EDGE ( 'NONE', *, *, #9196, .F. ) ;
#40423 = ORIENTED_EDGE ( 'NONE', *, *, #28175, .T. ) ;
#40424 = ADVANCED_FACE ( 'NONE', ( #28191 ), #16701, .T. ) ;
#40425 = CYLINDRICAL_SURFACE ( 'NONE', #25052, 31.99999999999998579 ) ;
#40426 = VECTOR ( 'NONE', #2058, 1000.000000000000000 ) ;
#40427 = DIRECTION ( 'NONE',  ( 0.000000000000000000, 0.07845909572784530439, -0.9969173337331279638 ) ) ;
#40428 = ORIENTED_EDGE ( 'NONE', *, *, #17515, .F. ) ;
#40429 = CARTESIAN_POINT ( 'NONE',  ( 10.00000000000000000, 0.000000000000000000, 0.000000000000000000 ) ) ;
#40430 = ORIENTED_EDGE ( 'NONE', *, *, #38501, .T. ) ;
#40431 = CARTESIAN_POINT ( 'NONE',  ( 10.00000000000000000, -25.88420570971419821, 27.13269053701087330 ) ) ;
#40432 = CARTESIAN_POINT ( 'NONE',  ( -10.00000000000000000, 0.000000000000000000, 0.000000000000000000 ) ) ;
#40433 = VERTEX_POINT ( 'NONE', #8861 ) ;
#40434 = CARTESIAN_POINT ( 'NONE',  ( 0.7800914985199594032, -118.7188063167744900, -2.500000000000000000 ) ) ;
#40435 = CARTESIAN_POINT ( 'NONE',  ( 10.00000000000000000, 35.91791733033475253, 68.67312586195009771 ) ) ;
#40436 = EDGE_CURVE ( 'NONE', #7287, #10250, #10479, .T. ) ;
#40438 = ORIENTED_EDGE ( 'NONE', *, *, #47420, .F. ) ;
#40437 = CARTESIAN_POINT ( 'NONE',  ( 12.13205353604972991, -140.1820037904669789, 5.500000000000000000 ) ) ;
#40439 = DIRECTION ( 'NONE',  ( 0.000000000000000000, -0.1564344650402381687, 0.9876883405951365491 ) ) ;
#40440 = VERTEX_POINT ( 'NONE', #9345 ) ;
#40441 = CYLINDRICAL_SURFACE ( 'NONE', #30316, 37.49900000000000233 ) ;
#40442 = ORIENTED_EDGE ( 'NONE', *, *, #5158, .F. ) ;
#40443 = ORIENTED_EDGE ( 'NONE', *, *, #25841, .F. ) ;
#40444 = DIRECTION ( 'NONE',  ( -0.000000000000000000, -0.000000000000000000, -1.000000000000000000 ) ) ;
#40445 = CARTESIAN_POINT ( 'NONE',  ( 0.000000000000000000, -74.65491531819111515, -8.830959090343204920 ) ) ;
#40446 = ORIENTED_EDGE ( 'NONE', *, *, #3239, .F. ) ;
#40447 = CARTESIAN_POINT ( 'NONE',  ( 10.00000000000000000, 0.000000000000000000, 0.000000000000000000 ) ) ;
#40448 = CARTESIAN_POINT ( 'NONE',  ( 10.00000000000000000, -70.53064760720297954, -26.01480285779911839 ) ) ;
#40449 = CARTESIAN_POINT ( 'NONE',  ( 10.00000000000000000, 0.000000000000000000, 0.000000000000000000 ) ) ;
#40450 = ORIENTED_EDGE ( 'NONE', *, *, #19829, .T. ) ;
#40451 = CARTESIAN_POINT ( 'NONE',  ( 10.00000000000000000, -78.73519480814971416, 22.90783923731600069 ) ) ;
#40452 = CARTESIAN_POINT ( 'NONE',  ( 18.80329974962065265, -105.8248132807389084, 5.500000000000000000 ) ) ;
#40453 = DIRECTION ( 'NONE',  ( 0.000000000000000000, 0.9510565162951544194, -0.3090169943749447867 ) ) ;
#40454 = VECTOR ( 'NONE', #10639, 1000.000000000000000 ) ;
#40455 = ORIENTED_EDGE ( 'NONE', *, *, #36950, .F. ) ;
#40456 = DIRECTION ( 'NONE',  ( 0.000000000000000000, -0.5877852522924802425, 0.8090169943749422332 ) ) ;
#40457 = DIRECTION ( 'NONE',  ( 0.000000000000000000, 0.1564344650402311743, -0.9876883405951377704 ) ) ;
#40458 = LINE ( 'NONE', #21109, #9154 ) ;
#40459 = LINE ( 'NONE', #2994, #45041 ) ;
#40460 = ADVANCED_FACE ( 'NONE', ( #12316 ), #42892, .T. ) ;
#40462 = EDGE_CURVE ( 'NONE', #36114, #4419, #47201, .T. ) ;
#40461 = CIRCLE ( 'NONE', #5272, 77.49899999999999523 ) ;
#40463 = DIRECTION ( 'NONE',  ( -1.000000000000000000, 0.000000000000000000, 0.000000000000000000 ) ) ;
#40464 = CARTESIAN_POINT ( 'NONE',  ( 11.99999999999999822, 76.69515212746057387, -29.01471420065479379 ) ) ;
#40465 = CARTESIAN_POINT ( 'NONE',  ( 11.99999999999999822, 0.000000000000000000, 0.000000000000000000 ) ) ;
#40466 = CARTESIAN_POINT ( 'NONE',  ( 10.00000000000000000, 0.000000000000000000, 0.000000000000000000 ) ) ;
#40467 = ADVANCED_FACE ( 'NONE', ( #5681 ), #5441, .T. ) ;
#40468 = ORIENTED_EDGE ( 'NONE', *, *, #29559, .F. ) ;
#40469 = ORIENTED_EDGE ( 'NONE', *, *, #22695, .F. ) ;
#40470 = CARTESIAN_POINT ( 'NONE',  ( 10.00000000000000000, 33.80338159004283938, 16.23288003029508886 ) ) ;
#40471 = AXIS2_PLACEMENT_3D ( 'NONE', #12759, #1268, #19591 ) ;
#40472 = ORIENTED_EDGE ( 'NONE', *, *, #33598, .T. ) ;
#40473 = EDGE_CURVE ( 'NONE', #19987, #44730, #31158, .T. ) ;
#40474 = CARTESIAN_POINT ( 'NONE',  ( 10.00000000000000000, 68.26794271651307611, -31.47745569255064169 ) ) ;
#40475 = CARTESIAN_POINT ( 'NONE',  ( 1.257674520083185143E-13, -3.848917712323540741E-15, 36.50000000000000711 ) ) ;
#40476 = LINE ( 'NONE', #48041, #40869 ) ;
#40477 = ORIENTED_EDGE ( 'NONE', *, *, #31014, .F. ) ;
#40478 = AXIS2_PLACEMENT_3D ( 'NONE', #10534, #10285, #18101 ) ;
#40479 = CARTESIAN_POINT ( 'NONE',  ( 11.99999999999999822, 0.000000000000000000, 0.000000000000000000 ) ) ;
#40480 = ORIENTED_EDGE ( 'NONE', *, *, #1233, .F. ) ;
#40481 = VECTOR ( 'NONE', #9129, 1000.000000000000227 ) ;
#40482 = DIRECTION ( 'NONE',  ( 0.000000000000000000, 0.000000000000000000, 1.000000000000000000 ) ) ;
#40483 = VERTEX_POINT ( 'NONE', #5211 ) ;
#40484 = CARTESIAN_POINT ( 'NONE',  ( 12.00000000000000000, 23.59884966291521735, -12.14883922797262805 ) ) ;
#40485 = DIRECTION ( 'NONE',  ( 0.9227826878668550226, 0.3853207896976523772, -0.000000000000000000 ) ) ;
#40486 = VERTEX_POINT ( 'NONE', #46803 ) ;
#40487 = VECTOR ( 'NONE', #8965, 1000.000000000000000 ) ;
#40488 = DIRECTION ( 'NONE',  ( -1.000000000000000000, -0.000000000000000000, 0.000000000000000000 ) ) ;
#40489 = AXIS2_PLACEMENT_3D ( 'NONE', #21926, #18008, #21694 ) ;
#40490 = ORIENTED_EDGE ( 'NONE', *, *, #25904, .T. ) ;
#40491 = CARTESIAN_POINT ( 'NONE',  ( 0.000000000000000000, 23.16143007188426850, 73.95703589263983702 ) ) ;
#40492 = DIRECTION ( 'NONE',  ( 0.000000000000000000, 0.000000000000000000, -1.000000000000000000 ) ) ;
#40493 = CARTESIAN_POINT ( 'NONE',  ( 15.00000000000000000, 22.07842321921480888, -8.187992925817425771 ) ) ;
#40494 = EDGE_LOOP ( 'NONE', ( #27137, #12705, #11792, #6058 ) ) ;
#40495 = CARTESIAN_POINT ( 'NONE',  ( -7.893099573151324044, -11.68370571044642503, 0.000000000000000000 ) ) ;
#40496 = ORIENTED_EDGE ( 'NONE', *, *, #23669, .T. ) ;
#40497 = ORIENTED_EDGE ( 'NONE', *, *, #17835, .T. ) ;
#40498 = CYLINDRICAL_SURFACE ( 'NONE', #1220, 82.00000000000000000 ) ;
#40499 = DIRECTION ( 'NONE',  ( -1.000000000000000000, -0.000000000000000000, -0.000000000000000000 ) ) ;
#40500 = DIRECTION ( 'NONE',  ( -0.6575728627325955200, 0.7533909544171996098, 1.230411769795008318E-16 ) ) ;
#40501 = DIRECTION ( 'NONE',  ( 0.000000000000000000, 0.000000000000000000, 1.000000000000000000 ) ) ;
#40502 = ORIENTED_EDGE ( 'NONE', *, *, #30109, .F. ) ;
#40503 = CARTESIAN_POINT ( 'NONE',  ( -3.000000000000000000, -11.95096189432312350, -23.69967320028773372 ) ) ;
#40504 = DIRECTION ( 'NONE',  ( -0.000000000000000000, -0.000000000000000000, -1.000000000000000000 ) ) ;
#40505 = FACE_OUTER_BOUND ( 'NONE', #1406, .T. ) ;
#40506 = VECTOR ( 'NONE', #26586, 1000.000000000000114 ) ;
#40507 = DIRECTION ( 'NONE',  ( -1.000000000000000000, 0.000000000000000000, -0.000000000000000000 ) ) ;
#40508 = LINE ( 'NONE', #21888, #22327 ) ;
#40509 = ORIENTED_EDGE ( 'NONE', *, *, #30399, .F. ) ;
#40510 = LINE ( 'NONE', #7207, #44316 ) ;
#40511 = EDGE_CURVE ( 'NONE', #28496, #14564, #12547, .T. ) ;
#40512 = PLANE ( 'NONE',  #173 ) ;
#40513 = CARTESIAN_POINT ( 'NONE',  ( -3.000000000000000000, 20.85821328998741109, 10.92862929874522315 ) ) ;
#40514 = EDGE_CURVE ( 'NONE', #10023, #15936, #1102, .T. ) ;
#40515 = CARTESIAN_POINT ( 'NONE',  ( 15.00000000000000000, -18.13022148937263012, -15.02647892043543898 ) ) ;
#40516 = DIRECTION ( 'NONE',  ( 0.000000000000000000, 0.9723699203976756689, 0.2334453638559094157 ) ) ;
#40517 = CARTESIAN_POINT ( 'NONE',  ( 10.00000000000000000, 70.52718814184294160, -26.02418014898236720 ) ) ;
#40518 = ORIENTED_EDGE ( 'NONE', *, *, #33918, .T. ) ;
#40519 = EDGE_CURVE ( 'NONE', #20542, #21097, #19819, .T. ) ;
#40520 = DIRECTION ( 'NONE',  ( 1.000000000000000000, 0.000000000000000000, -0.000000000000000000 ) ) ;
#40521 = AXIS2_PLACEMENT_3D ( 'NONE', #14362, #13402, #2857 ) ;
#40522 = ADVANCED_FACE ( 'NONE', ( #27235 ), #23548, .T. ) ;
#40523 = CIRCLE ( 'NONE', #17863, 37.49900000000001654 ) ;
#40524 = DIRECTION ( 'NONE',  ( -1.000000000000000000, -0.000000000000000000, 0.000000000000000000 ) ) ;
#40525 = ORIENTED_EDGE ( 'NONE', *, *, #11460, .F. ) ;
#40526 = ORIENTED_EDGE ( 'NONE', *, *, #43982, .T. ) ;
#40527 = CARTESIAN_POINT ( 'NONE',  ( 10.00000000000000000, 58.39081064771751528, 50.95692526931350841 ) ) ;
#40528 = AXIS2_PLACEMENT_3D ( 'NONE', #14525, #29448, #18660 ) ;
#40529 = ORIENTED_EDGE ( 'NONE', *, *, #23272, .F. ) ;
#40530 = VECTOR ( 'NONE', #14755, 1000.000000000000000 ) ;
#40531 = ORIENTED_EDGE ( 'NONE', *, *, #15283, .T. ) ;
#40532 = CARTESIAN_POINT ( 'NONE',  ( 10.00000000000000000, 35.38097989696512968, 12.42422080174651100 ) ) ;
#40533 = DIRECTION ( 'NONE',  ( 0.000000000000000000, 0.000000000000000000, 1.000000000000000000 ) ) ;
#40534 = DIRECTION ( 'NONE',  ( -0.1045284632676436315, -0.9945218953682742891, 0.000000000000000000 ) ) ;
#40535 = ORIENTED_EDGE ( 'NONE', *, *, #28354, .F. ) ;
#40536 = CARTESIAN_POINT ( 'NONE',  ( 23.49916127795269460, -121.5130826919798039, 5.500000000000000000 ) ) ;
#40537 = ORIENTED_EDGE ( 'NONE', *, *, #2472, .T. ) ;
#40538 = VERTEX_POINT ( 'NONE', #12789 ) ;
#40539 = ORIENTED_EDGE ( 'NONE', *, *, #38249, .F. ) ;
#40540 = CARTESIAN_POINT ( 'NONE',  ( 22.94323693612312809, -114.6983135802921083, -5.500000000000000000 ) ) ;
#40541 = LINE ( 'NONE', #7244, #25092 ) ;
#40542 = FACE_BOUND ( 'NONE', #18773, .T. ) ;
#40543 = EDGE_CURVE ( 'NONE', #35058, #29586, #8903, .T. ) ;
#40544 = VERTEX_POINT ( 'NONE', #35780 ) ;
#40545 = ORIENTED_EDGE ( 'NONE', *, *, #37862, .F. ) ;
#40546 = DIRECTION ( 'NONE',  ( 0.000000000000000000, -0.4067366430758009854, -0.9135454576426004225 ) ) ;
#40547 = EDGE_LOOP ( 'NONE', ( #40910, #28077, #27489, #28972 ) ) ;
#40548 = CARTESIAN_POINT ( 'NONE',  ( 14.59956846177685996, -138.4757300459248484, -5.500000000000000000 ) ) ;
#40549 = EDGE_CURVE ( 'NONE', #20931, #10647, #38981, .T. ) ;
#40550 = LINE ( 'NONE', #18017, #45183 ) ;
#40551 = DIRECTION ( 'NONE',  ( 0.000000000000000000, -0.5224985647159380298, -0.8526401643540988395 ) ) ;
#40552 = ORIENTED_EDGE ( 'NONE', *, *, #23974, .F. ) ;
#40553 = CARTESIAN_POINT ( 'NONE',  ( 0.000000000000000000, 0.000000000000000000, 0.000000000000000000 ) ) ;
#40554 = LINE ( 'NONE', #25128, #26848 ) ;
#40555 = VECTOR ( 'NONE', #2309, 1000.000000000000000 ) ;
#40556 = EDGE_CURVE ( 'NONE', #17607, #22223, #29241, .T. ) ;
#40557 = DIRECTION ( 'NONE',  ( 0.000000000000000000, 0.000000000000000000, 1.000000000000000000 ) ) ;
#40558 = DIRECTION ( 'NONE',  ( 0.000000000000000000, 0.2334453638559060851, -0.9723699203976764460 ) ) ;
#40559 = CARTESIAN_POINT ( 'NONE',  ( 5.822613034544236399, -142.8165987265839760, 5.500000000000000000 ) ) ;
#40560 = ORIENTED_EDGE ( 'NONE', *, *, #24733, .F. ) ;
#40561 = DIRECTION ( 'NONE',  ( 0.000000000000000000, 0.000000000000000000, 1.000000000000000000 ) ) ;
#40562 = CARTESIAN_POINT ( 'NONE',  ( 11.99999999999999822, -74.65491531819111515, -8.830959090343204920 ) ) ;
#40563 = DIRECTION ( 'NONE',  ( -5.778480238264233142E-17, 1.000000000000000000, -0.000000000000000000 ) ) ;
#40564 = CARTESIAN_POINT ( 'NONE',  ( 0.000000000000000000, -76.41127070299262414, -12.93880638057396304 ) ) ;
#40565 = EDGE_CURVE ( 'NONE', #47238, #15972, #8138, .T. ) ;
#40566 = ADVANCED_FACE ( 'NONE', ( #8612 ), #20354, .T. ) ;
#40567 = EDGE_CURVE ( 'NONE', #23195, #38922, #47283, .T. ) ;
#40568 = CYLINDRICAL_SURFACE ( 'NONE', #13813, 30.50000000000000000 ) ;
#40569 = COLOUR_RGB ( '', 0.72549020, 0.75294118, 0.79215686) ;
#40570 = DIRECTION ( 'NONE',  ( 0.000000000000000000, 0.4539904997395477482, -0.8910065241883674547 ) ) ;
#40571 = CARTESIAN_POINT ( 'NONE',  ( 10.00000000000000000, 4.992566952384984269, 37.16516213103279398 ) ) ;
#40572 = CARTESIAN_POINT ( 'NONE',  ( 11.99999999999999822, 65.58780272294129077, -36.73666225445822420 ) ) ;
#40573 = DIRECTION ( 'NONE',  ( -1.000000000000000000, 0.000000000000000000, 0.000000000000000000 ) ) ;
#40574 = ADVANCED_FACE ( 'NONE', ( #13980 ), #18119, .T. ) ;
#40575 = FILL_AREA_STYLE ('',( #10726 ) ) ;
#40576 = DIRECTION ( 'NONE',  ( 0.000000000000000000, 0.000000000000000000, 1.000000000000000000 ) ) ;
#40577 = ORIENTED_EDGE ( 'NONE', *, *, #28247, .F. ) ;
#40578 = AXIS2_PLACEMENT_3D ( 'NONE', #3369, #18306, #33245 ) ;
#40579 = ORIENTED_EDGE ( 'NONE', *, *, #9558, .F. ) ;
#40580 = CIRCLE ( 'NONE', #6974, 82.00000000000000000 ) ;
#40581 = EDGE_CURVE ( 'NONE', #45240, #34021, #15173, .T. ) ;
#40582 = CARTESIAN_POINT ( 'NONE',  ( 7.893099573151324044, -11.68370571044642503, -1.199999999999999956 ) ) ;
#40583 = DIRECTION ( 'NONE',  ( 1.000000000000000000, 0.000000000000000000, 0.000000000000000000 ) ) ;
#40584 = AXIS2_PLACEMENT_3D ( 'NONE', #21866, #40260, #6716 ) ;
#40585 = EDGE_LOOP ( 'NONE', ( #38613, #7019, #43080, #42902 ) ) ;
#40586 = CARTESIAN_POINT ( 'NONE',  ( 0.000000000000000000, 0.000000000000000000, 0.000000000000000000 ) ) ;
#40587 = ORIENTED_EDGE ( 'NONE', *, *, #35912, .T. ) ;
#40588 = VERTEX_POINT ( 'NONE', #21797 ) ;
#40589 = PRODUCT_DEFINITION_SHAPE ( 'NONE', 'NONE',  #48458 ) ;
#40590 = CARTESIAN_POINT ( 'NONE',  ( 0.000000000000000000, 75.11725578898467859, 2.956366410620910656 ) ) ;
#40591 = ADVANCED_FACE ( 'NONE', ( #17400 ), #13755, .T. ) ;
#40592 = ORIENTED_EDGE ( 'NONE', *, *, #24195, .T. ) ;
#40593 = CARTESIAN_POINT ( 'NONE',  ( 10.00000000000000000, 0.000000000000000000, 0.000000000000000000 ) ) ;
#40594 = VERTEX_POINT ( 'NONE', #25474 ) ;
#40595 = LINE ( 'NONE', #25652, #7982 ) ;
#40596 = EDGE_CURVE ( 'NONE', #10624, #21719, #10983, .T. ) ;
#40597 = DIRECTION ( 'NONE',  ( -1.000000000000000000, -0.000000000000000000, 0.000000000000000000 ) ) ;
#40598 = DIRECTION ( 'NONE',  ( -1.000000000000000000, 3.469446951953611033E-15, 0.000000000000000000 ) ) ;
#40599 = EDGE_CURVE ( 'NONE', #17612, #41379, #10800, .T. ) ;
#40600 = ORIENTED_EDGE ( 'NONE', *, *, #12240, .T. ) ;
#40601 = ORIENTED_EDGE ( 'NONE', *, *, #14464, .F. ) ;
#40602 = DIRECTION ( 'NONE',  ( -1.000000000000000000, 0.000000000000000000, 0.000000000000000000 ) ) ;
#40603 = AXIS2_PLACEMENT_3D ( 'NONE', #34775, #41411, #26241 ) ;
#40604 = DIRECTION ( 'NONE',  ( 0.000000000000000000, 0.000000000000000000, 1.000000000000000000 ) ) ;
#40605 = VERTEX_POINT ( 'NONE', #24991 ) ;
#40606 = ORIENTED_EDGE ( 'NONE', *, *, #34034, .F. ) ;
#40607 = FACE_OUTER_BOUND ( 'NONE', #9327, .T. ) ;
#40608 = LINE ( 'NONE', #47697, #18361 ) ;
#40609 = ADVANCED_FACE ( 'NONE', ( #6646 ), #36492, .F. ) ;
#40610 = VERTEX_POINT ( 'NONE', #43608 ) ;
#40611 = ORIENTED_EDGE ( 'NONE', *, *, #25668, .T. ) ;
#40612 = AXIS2_PLACEMENT_3D ( 'NONE', #13262, #28428, #35773 ) ;
#40613 = CYLINDRICAL_SURFACE ( 'NONE', #15220, 16.00000000000000000 ) ;
#40614 = PLANE ( 'NONE',  #15741 ) ;
#40615 = LINE ( 'NONE', #4148, #26130 ) ;
#40616 = CARTESIAN_POINT ( 'NONE',  ( 0.000000000000000000, 70.52718814184294160, -26.02418014898236720 ) ) ;
#40617 = CARTESIAN_POINT ( 'NONE',  ( 0.000000000000000000, 76.69515212746016175, 29.01471420065591289 ) ) ;
#40618 = EDGE_CURVE ( 'NONE', #35941, #27912, #8633, .T. ) ;
#40619 = ADVANCED_FACE ( 'NONE', ( #43839 ), #40425, .T. ) ;
#40620 = DIRECTION ( 'NONE',  ( 0.000000000000000000, 0.000000000000000000, 1.000000000000000000 ) ) ;
#40621 = FACE_OUTER_BOUND ( 'NONE', #30972, .T. ) ;
#40622 = CARTESIAN_POINT ( 'NONE',  ( 11.99999999999999822, -78.73519480814938731, -22.90783923731713045 ) ) ;
#40623 = ORIENTED_EDGE ( 'NONE', *, *, #5997, .T. ) ;
#40624 = DIRECTION ( 'NONE',  ( 0.000000000000000000, 0.000000000000000000, 1.000000000000000000 ) ) ;
#40625 = CARTESIAN_POINT ( 'NONE',  ( 0.000000000000000000, 39.04073710021366139, -15.48615015657542315 ) ) ;
#40626 = FILL_AREA_STYLE ('',( #10777 ) ) ;
#40627 = CARTESIAN_POINT ( 'NONE',  ( -32.50000000000000000, -120.0000000000000000, 2.500000000000000000 ) ) ;
#40628 = VERTEX_POINT ( 'NONE', #7116 ) ;
#40629 = EDGE_CURVE ( 'NONE', #5281, #23433, #39120, .T. ) ;
#40630 = ORIENTED_EDGE ( 'NONE', *, *, #20472, .F. ) ;
#40631 = FACE_OUTER_BOUND ( 'NONE', #28311, .T. ) ;
#40632 = CARTESIAN_POINT ( 'NONE',  ( 11.99999999999999822, 0.000000000000000000, 0.000000000000000000 ) ) ;
#40633 = ORIENTED_EDGE ( 'NONE', *, *, #28410, .T. ) ;
#40634 = EDGE_LOOP ( 'NONE', ( #6797, #18454, #16024, #31630 ) ) ;
#40635 = CIRCLE ( 'NONE', #8595, 16.00000000000000355 ) ;
#40636 = VECTOR ( 'NONE', #1351, 1000.000000000000000 ) ;
#40637 = CARTESIAN_POINT ( 'NONE',  ( 11.99999999999999822, -2.946379043146863719, 75.11764819372146462 ) ) ;
#40638 = ORIENTED_EDGE ( 'NONE', *, *, #11154, .T. ) ;
#40639 = DIRECTION ( 'NONE',  ( -1.000000000000000000, 0.000000000000000000, -0.000000000000000000 ) ) ;
#40640 = VERTEX_POINT ( 'NONE', #36967 ) ;
#40641 = VECTOR ( 'NONE', #4647, 1000.000000000000000 ) ;
#40642 = ORIENTED_EDGE ( 'NONE', *, *, #1779, .F. ) ;
#40643 = ORIENTED_EDGE ( 'NONE', *, *, #1035, .T. ) ;
#40644 = SURFACE_STYLE_USAGE ( .BOTH. , #2471 ) ;
#40645 = CIRCLE ( 'NONE', #22691, 82.00000000000000000 ) ;
#40646 = CIRCLE ( 'NONE', #25795, 82.00000000000000000 ) ;
#40647 = CARTESIAN_POINT ( 'NONE',  ( 5.000000000000000000, -67.80270845531855173, -46.11716303203261447 ) ) ;
#40648 = CIRCLE ( 'NONE', #10158, 77.49899999999999523 ) ;
#40649 = ORIENTED_EDGE ( 'NONE', *, *, #16026, .F. ) ;
#40650 = ORIENTED_EDGE ( 'NONE', *, *, #23415, .F. ) ;
#40651 = CARTESIAN_POINT ( 'NONE',  ( -235.0000123116479926, -123.0000000000000284, -2.500000000000000000 ) ) ;
#40652 = EDGE_LOOP ( 'NONE', ( #20922, #5075, #44582, #27294 ) ) ;
#40653 = EDGE_CURVE ( 'NONE', #33790, #26325, #3974, .T. ) ;
#40654 = DIRECTION ( 'NONE',  ( 1.000000000000000000, 0.000000000000000000, 0.000000000000000000 ) ) ;
#40655 = CARTESIAN_POINT ( 'NONE',  ( 10.00000000000000000, -59.46389618801928378, -49.70050353004953791 ) ) ;
#40656 = EDGE_CURVE ( 'NONE', #19341, #22651, #2955, .T. ) ;
#40657 = ORIENTED_EDGE ( 'NONE', *, *, #34922, .T. ) ;
#40658 = DIRECTION ( 'NONE',  ( 0.000000000000000000, -0.9969173337331287410, 0.07845909572783495156 ) ) ;
#40659 = PLANE ( 'NONE',  #7527 ) ;
#40660 = EDGE_LOOP ( 'NONE', ( #39385, #8974, #24715, #13549 ) ) ;
#40662 = ORIENTED_EDGE ( 'NONE', *, *, #27290, .F. ) ;
#40661 = DIRECTION ( 'NONE',  ( -1.000000000000000000, -0.000000000000000000, 0.000000000000000000 ) ) ;
#40663 = CARTESIAN_POINT ( 'NONE',  ( 10.00000000000000000, -38.55633173627023069, 16.65560815589396526 ) ) ;
#40664 = VERTEX_POINT ( 'NONE', #36008 ) ;
#40665 = DIRECTION ( 'NONE',  ( 1.000000000000000000, 0.000000000000000000, -0.000000000000000000 ) ) ;
#40666 = ORIENTED_EDGE ( 'NONE', *, *, #32619, .T. ) ;
#40667 = EDGE_LOOP ( 'NONE', ( #14840, #19344, #37179, #3082 ) ) ;
#40668 = CARTESIAN_POINT ( 'NONE',  ( 5.000000000000000000, -26.79245525562690844, -32.34446384430000876 ) ) ;
#40669 = DIRECTION ( 'NONE',  ( -1.000000000000000000, 0.000000000000000000, 0.000000000000000000 ) ) ;
#40670 = ORIENTED_EDGE ( 'NONE', *, *, #47263, .F. ) ;
#40671 = CARTESIAN_POINT ( 'NONE',  ( 10.00000000000000000, 37.22597642581158084, -5.202137450156524068 ) ) ;
#40672 = DIRECTION ( 'NONE',  ( -1.000000000000000000, -0.000000000000000000, 0.000000000000000000 ) ) ;
#40673 = DIRECTION ( 'NONE',  ( -0.7950889364178781449, 0.6064928550163533050, 0.000000000000000000 ) ) ;
#40674 = ORIENTED_EDGE ( 'NONE', *, *, #38413, .F. ) ;
#40675 = CARTESIAN_POINT ( 'NONE',  ( 15.00000000000000000, -11.95096189432312350, 23.69967320028773372 ) ) ;
#40676 = CARTESIAN_POINT ( 'NONE',  ( 11.99999999999999822, 0.000000000000000000, 0.000000000000000000 ) ) ;
#40677 = EDGE_CURVE ( 'NONE', #34210, #45280, #42261, .T. ) ;
#40679 = CIRCLE ( 'NONE', #45348, 42.00000000000000000 ) ;
#40678 = DIRECTION ( 'NONE',  ( -1.000000000000000000, 0.000000000000000000, 0.000000000000000000 ) ) ;
#40680 = AXIS2_PLACEMENT_3D ( 'NONE', #41813, #8272, #27126 ) ;
#40681 = CARTESIAN_POINT ( 'NONE',  ( 10.00000000000000000, -4.992566952385247170, 37.16516213103275845 ) ) ;
#40682 = EDGE_CURVE ( 'NONE', #31490, #24228, #39712, .T. ) ;
#40683 = LINE ( 'NONE', #7153, #30600 ) ;
#40684 = DIRECTION ( 'NONE',  ( -0.6516173805718079581, 0.7585478161175706058, 0.000000000000000000 ) ) ;
#40685 = CARTESIAN_POINT ( 'NONE',  ( 11.99999999999999822, 0.000000000000000000, 0.000000000000000000 ) ) ;
#40686 = AXIS2_PLACEMENT_3D ( 'NONE', #42735, #20687, #24125 ) ;
#40687 = VERTEX_POINT ( 'NONE', #28903 ) ;
#40688 = DIRECTION ( 'NONE',  ( 1.000000000000000000, -0.000000000000000000, -0.000000000000000000 ) ) ;
#40689 = DIRECTION ( 'NONE',  ( -1.000000000000000000, -0.000000000000000000, -0.000000000000000000 ) ) ;
#40690 = LINE ( 'NONE', #18652, #25622 ) ;
#40691 = CARTESIAN_POINT ( 'NONE',  ( 0.000000000000000000, -22.48208911017474065, -35.47612816024548721 ) ) ;
#40692 = AXIS2_PLACEMENT_3D ( 'NONE', #40448, #17908, #14501 ) ;
#40693 = ADVANCED_FACE ( 'NONE', ( #10300 ), #25218, .T. ) ;
#40694 = ORIENTED_EDGE ( 'NONE', *, *, #42773, .F. ) ;
#40695 = DIRECTION ( 'NONE',  ( -1.000000000000000000, -0.000000000000000000, -0.000000000000000000 ) ) ;
#40696 = AXIS2_PLACEMENT_3D ( 'NONE', #24232, #35969, #17126 ) ;
#40697 = VERTEX_POINT ( 'NONE', #14222 ) ;
#40698 = CYLINDRICAL_SURFACE ( 'NONE', #26797, 77.49899999999999523 ) ;
#40699 = DIRECTION ( 'NONE',  ( 0.000000000000000000, 0.000000000000000000, -1.000000000000000000 ) ) ;
#40700 = FACE_OUTER_BOUND ( 'NONE', #13964, .T. ) ;
#40701 = ORIENTED_EDGE ( 'NONE', *, *, #9116, .F. ) ;
#40702 = PLANE ( 'NONE',  #36210 ) ;
#40703 = ORIENTED_EDGE ( 'NONE', *, *, #23260, .T. ) ;
#40704 = AXIS2_PLACEMENT_3D ( 'NONE', #31189, #27509, #20152 ) ;
#40705 = CARTESIAN_POINT ( 'NONE',  ( 11.99999999999999822, 59.46389618801966037, 49.70050353004911159 ) ) ;
#40706 = CIRCLE ( 'NONE', #27451, 11.59999999999999787 ) ;
#40707 = EDGE_CURVE ( 'NONE', #9216, #43358, #14899, .T. ) ;
#40708 = LINE ( 'NONE', #26750, #37532 ) ;
#40709 = DIRECTION ( 'NONE',  ( 0.000000000000000000, 0.6494480483301793283, 0.7604059656000345946 ) ) ;
#40710 = AXIS2_PLACEMENT_3D ( 'NONE', #8636, #31915, #35567 ) ;
#40711 = VECTOR ( 'NONE', #19559, 1000.000000000000114 ) ;
#40712 = VERTEX_POINT ( 'NONE', #730 ) ;
#40713 = ADVANCED_FACE ( 'NONE', ( #45059 ), #29871, .T. ) ;
#40714 = LINE ( 'NONE', #2534, #34808 ) ;
#40715 = ORIENTED_EDGE ( 'NONE', *, *, #22295, .T. ) ;
#40716 = EDGE_CURVE ( 'NONE', #32005, #31590, #21138, .T. ) ;
#40717 = VECTOR ( 'NONE', #42305, 1000.000000000000000 ) ;
#40718 = CARTESIAN_POINT ( 'NONE',  ( 10.00000000000000000, -73.72996012237429397, -14.67089635893794508 ) ) ;
#40719 = CYLINDRICAL_SURFACE ( 'NONE', #28840, 31.99999999999998579 ) ;
#40720 = AXIS2_PLACEMENT_3D ( 'NONE', #24959, #2213, #17137 ) ;
#40721 = CARTESIAN_POINT ( 'NONE',  ( 10.00000000000000000, 0.000000000000000000, 0.000000000000000000 ) ) ;
#40722 = CYLINDRICAL_SURFACE ( 'NONE', #2291, 16.00000000000000000 ) ;
#40723 = VERTEX_POINT ( 'NONE', #23261 ) ;
#40724 = ADVANCED_FACE ( 'NONE', ( #48237 ), #15668, .F. ) ;
#40725 =( GEOMETRIC_REPRESENTATION_CONTEXT ( 3 ) GLOBAL_UNCERTAINTY_ASSIGNED_CONTEXT ( ( #30114 ) ) GLOBAL_UNIT_ASSIGNED_CONTEXT ( ( #4857, #34221, #27144 ) ) REPRESENTATION_CONTEXT ( 'NONE', 'WORKASPACE' ) );
#40726 = CARTESIAN_POINT ( 'NONE',  ( 0.000000000000000000, 0.000000000000000000, 0.000000000000000000 ) ) ;
#40727 = VERTEX_POINT ( 'NONE', #19335 ) ;
#40728 = ORIENTED_EDGE ( 'NONE', *, *, #17635, .F. ) ;
#40729 = EDGE_CURVE ( 'NONE', #8618, #39073, #11755, .T. ) ;
#40730 = DIRECTION ( 'NONE',  ( -1.000000000000000000, 0.000000000000000000, 0.000000000000000000 ) ) ;
#40731 = CARTESIAN_POINT ( 'NONE',  ( 5.000000000000000000, -74.74816331893454446, 33.71516098798714722 ) ) ;
#40732 = LINE ( 'NONE', #48076, #46148 ) ;
#40733 = CYLINDRICAL_SURFACE ( 'NONE', #23482, 82.00000000000000000 ) ;
#40734 = EDGE_LOOP ( 'NONE', ( #3365, #5588, #15623, #24330 ) ) ;
#40735 = CARTESIAN_POINT ( 'NONE',  ( 10.00000000000000000, -33.00180498840035170, -17.80606268964575278 ) ) ;
#40736 = DIRECTION ( 'NONE',  ( 0.000000000000000000, 0.000000000000000000, 1.000000000000000000 ) ) ;
#40737 = CARTESIAN_POINT ( 'NONE',  ( 6.000000000000000000, 71.21200624218852226, -40.65526001592539984 ) ) ;
#40738 = CARTESIAN_POINT ( 'NONE',  ( -1.474095553543409487, -120.2775649455957989, 2.500000000000000000 ) ) ;
#40739 = CARTESIAN_POINT ( 'NONE',  ( 10.00000000000000000, 71.91182617369230456, -28.89263327155667938 ) ) ;
#40740 = CARTESIAN_POINT ( 'NONE',  ( 10.00000000000000000, -35.53030884539077050, -12.26510123303296851 ) ) ;
#40741 = DIRECTION ( 'NONE',  ( 1.000000000000000000, 0.000000000000000000, 0.000000000000000000 ) ) ;
#40742 = DIRECTION ( 'NONE',  ( 0.000000000000000000, 0.9510565162951546414, -0.3090169943749442871 ) ) ;
#40743 = CARTESIAN_POINT ( 'NONE',  ( 0.000000000000000000, 35.53030884539102630, -12.26510123303222599 ) ) ;
#40744 = LINE ( 'NONE', #40513, #35451 ) ;
#40745 = CARTESIAN_POINT ( 'NONE',  ( 0.000000000000000000, 0.000000000000000000, 40.00000000000000000 ) ) ;
#40746 = VECTOR ( 'NONE', #33573, 1000.000000000000000 ) ;
#40747 = EDGE_CURVE ( 'NONE', #17337, #17528, #47684, .T. ) ;
#40748 = CARTESIAN_POINT ( 'NONE',  ( 10.00000000000000000, -62.50884508063395373, -41.76106447765554464 ) ) ;
#40749 = FACE_OUTER_BOUND ( 'NONE', #17175, .T. ) ;
#40750 = AXIS2_PLACEMENT_3D ( 'NONE', #2311, #28750, #10867 ) ;
#40751 = FACE_OUTER_BOUND ( 'NONE', #30428, .T. ) ;
#40752 = CARTESIAN_POINT ( 'NONE',  ( -3.000000000000000000, 20.85821328998756385, -10.92862929874494959 ) ) ;
#40753 = VECTOR ( 'NONE', #23271, 1000.000000000000000 ) ;
#40754 = VECTOR ( 'NONE', #21458, 1000.000000000000000 ) ;
#40755 = ADVANCED_FACE ( 'NONE', ( #37701 ), #41383, .T. ) ;
#40756 = CYLINDRICAL_SURFACE ( 'NONE', #17374, 31.99999999999998579 ) ;
#40757 = VECTOR ( 'NONE', #23634, 1000.000000000000000 ) ;
#40758 = ORIENTED_EDGE ( 'NONE', *, *, #30194, .F. ) ;
#40759 = ORIENTED_EDGE ( 'NONE', *, *, #42777, .F. ) ;
#40760 = ADVANCED_FACE ( 'NONE', ( #15441 ), #4182, .T. ) ;
#40761 = VERTEX_POINT ( 'NONE', #18617 ) ;
#40762 = VECTOR ( 'NONE', #40500, 1000.000000000000114 ) ;
#40763 = EDGE_LOOP ( 'NONE', ( #26503, #26260, #38261, #22782 ) ) ;
#40764 = VECTOR ( 'NONE', #16401, 1000.000000000000000 ) ;
#40765 = ORIENTED_EDGE ( 'NONE', *, *, #4161, .T. ) ;
#40766 = DIRECTION ( 'NONE',  ( 0.000000000000000000, 1.000000000000000000, 3.469446951953614189E-15 ) ) ;
#40767 = ORIENTED_EDGE ( 'NONE', *, *, #30294, .T. ) ;
#40768 = EDGE_CURVE ( 'NONE', #9305, #40415, #27415, .T. ) ;
#40769 = CARTESIAN_POINT ( 'NONE',  ( -3.000000000000000000, 0.000000000000000000, 0.000000000000000000 ) ) ;
#40770 = ADVANCED_FACE ( 'NONE', ( #509 ), #33309, .T. ) ;
#40771 = LINE ( 'NONE', #18497, #24983 ) ;
#40772 = CARTESIAN_POINT ( 'NONE',  ( 119.3426274441929280, -132.5434155921172419, 5.500000000000000000 ) ) ;
#40773 = ORIENTED_EDGE ( 'NONE', *, *, #33706, .T. ) ;
#40774 = FACE_OUTER_BOUND ( 'NONE', #20332, .T. ) ;
#40775 = ADVANCED_FACE ( 'NONE', ( #15204 ), #29744, .F. ) ;
#40776 = ORIENTED_EDGE ( 'NONE', *, *, #7215, .F. ) ;
#40777 = ORIENTED_EDGE ( 'NONE', *, *, #16095, .F. ) ;
#40778 = CARTESIAN_POINT ( 'NONE',  ( 0.000000000000000000, -35.92658777277517856, 10.74501242461269257 ) ) ;
#40779 = CYLINDRICAL_SURFACE ( 'NONE', #10237, 77.49899999999999523 ) ;
#40780 = CIRCLE ( 'NONE', #2473, 31.99999999999999289 ) ;
#40781 = CARTESIAN_POINT ( 'NONE',  ( 0.000000000000000000, -46.21855187248673502, 62.20884554314003623 ) ) ;
#40783 = ORIENTED_EDGE ( 'NONE', *, *, #42660, .F. ) ;
#40782 = AXIS2_PLACEMENT_3D ( 'NONE', #38258, #35063, #16466 ) ;
#40784 = ORIENTED_EDGE ( 'NONE', *, *, #45215, .F. ) ;
#40785 = CARTESIAN_POINT ( 'NONE',  ( 10.00000000000000000, 0.000000000000000000, 0.000000000000000000 ) ) ;
#40786 = ORIENTED_EDGE ( 'NONE', *, *, #11163, .T. ) ;
#40787 = EDGE_CURVE ( 'NONE', #8228, #13990, #6315, .T. ) ;
#40788 = AXIS2_PLACEMENT_3D ( 'NONE', #24059, #13046, #24998 ) ;
#40789 = DIRECTION ( 'NONE',  ( 0.000000000000000000, 0.9945218953682729568, 0.1045284632676578424 ) ) ;
#40790 = CARTESIAN_POINT ( 'NONE',  ( -26.29030328629083968, -123.6496510949466341, -5.500000000000000000 ) ) ;
#40791 = DIRECTION ( 'NONE',  ( -1.000000000000000000, 0.000000000000000000, 0.000000000000000000 ) ) ;
#40792 = CARTESIAN_POINT ( 'NONE',  ( 0.000000000000000000, -10.41901085202050581, -40.68715046381939970 ) ) ;
#40793 = DIRECTION ( 'NONE',  ( -1.000000000000000000, -0.000000000000000000, 0.000000000000000000 ) ) ;
#40794 = CIRCLE ( 'NONE', #20452, 31.99999999999998579 ) ;
#40795 = CIRCLE ( 'NONE', #12644, 31.99999999999998934 ) ;
#40796 = CARTESIAN_POINT ( 'NONE',  ( 0.000000000000000000, 77.32052557432841411, 5.256550761633121738 ) ) ;
#40797 = CARTESIAN_POINT ( 'NONE',  ( 10.00000000000000000, 16.23288003029497162, 33.80338159004289622 ) ) ;
#40798 = DIRECTION ( 'NONE',  ( -1.000000000000000000, 0.000000000000000000, -0.000000000000000000 ) ) ;
#40799 = CARTESIAN_POINT ( 'NONE',  ( -23.97194136764370498, -131.3950000906648938, 5.500000000000000000 ) ) ;
#40800 = ORIENTED_EDGE ( 'NONE', *, *, #47922, .T. ) ;
#40801 = DIRECTION ( 'NONE',  ( -1.000000000000000000, 0.000000000000000000, 0.000000000000000000 ) ) ;
#40802 = ORIENTED_EDGE ( 'NONE', *, *, #6866, .F. ) ;
#40803 = CIRCLE ( 'NONE', #9516, 31.99999999999999289 ) ;
#40804 = CARTESIAN_POINT ( 'NONE',  ( 0.000000000000000000, 15.33399622253600292, -80.55351364060572905 ) ) ;
#40805 = CYLINDRICAL_SURFACE ( 'NONE', #27517, 37.49900000000000233 ) ;
#40806 = DIRECTION ( 'NONE',  ( 0.000000000000000000, 0.000000000000000000, 1.000000000000000000 ) ) ;
#40807 = EDGE_CURVE ( 'NONE', #8701, #31375, #7365, .T. ) ;
#40808 = DIRECTION ( 'NONE',  ( 0.000000000000000000, -0.3090169943749349057, -0.9510565162951576390 ) ) ;
#40809 = CARTESIAN_POINT ( 'NONE',  ( -42.50000000000000000, 0.000000000000000000, 0.000000000000000000 ) ) ;
#40810 = ORIENTED_EDGE ( 'NONE', *, *, #46405, .F. ) ;
#40811 = CARTESIAN_POINT ( 'NONE',  ( 11.59999999999999787, 1.420590287010929336E-15, 52.00000000000002132 ) ) ;
#40812 = CARTESIAN_POINT ( 'NONE',  ( -7.469491406282094736, 4.756046723998911929, 32.98187577049606745 ) ) ;
#40813 = ORIENTED_EDGE ( 'NONE', *, *, #1069, .T. ) ;
#40814 = CARTESIAN_POINT ( 'NONE',  ( 0.000000000000000000, 0.000000000000000000, 0.000000000000000000 ) ) ;
#40815 =( NAMED_UNIT ( * ) SI_UNIT ( $, .STERADIAN. ) SOLID_ANGLE_UNIT ( ) );
#40816 = DIRECTION ( 'NONE',  ( -1.000000000000000000, 0.000000000000000000, -0.000000000000000000 ) ) ;
#40817 = ORIENTED_EDGE ( 'NONE', *, *, #31623, .T. ) ;
#40818 = ORIENTED_EDGE ( 'NONE', *, *, #24861, .T. ) ;
#40819 = AXIS2_PLACEMENT_3D ( 'NONE', #1386, #16311, #31253 ) ;
#40820 = AXIS2_PLACEMENT_3D ( 'NONE', #27189, #41626, #15677 ) ;
#40821 = EDGE_CURVE ( 'NONE', #16336, #29421, #4732, .T. ) ;
#40822 = ORIENTED_EDGE ( 'NONE', *, *, #12483, .T. ) ;
#40823 = DIRECTION ( 'NONE',  ( 1.000000000000000000, 0.000000000000000000, 0.000000000000000000 ) ) ;
#40824 = DIRECTION ( 'NONE',  ( -1.000000000000000000, 0.000000000000000000, 0.000000000000000000 ) ) ;
#40825 = VERTEX_POINT ( 'NONE', #44803 ) ;
#40826 = ORIENTED_EDGE ( 'NONE', *, *, #26364, .T. ) ;
#40827 = VECTOR ( 'NONE', #40507, 1000.000000000000000 ) ;
#40828 = VERTEX_POINT ( 'NONE', #23017 ) ;
#40829 = CARTESIAN_POINT ( 'NONE',  ( -0.9774260708577104939, -118.8621782758236378, -2.500000000000000000 ) ) ;
#40830 = CIRCLE ( 'NONE', #34556, 31.99999999999998579 ) ;
#40831 = VERTEX_POINT ( 'NONE', #11290 ) ;
#40832 = VERTEX_POINT ( 'NONE', #41152 ) ;
#40833 = EDGE_CURVE ( 'NONE', #14124, #34627, #9401, .T. ) ;
#40834 = EDGE_CURVE ( 'NONE', #4138, #14124, #43787, .T. ) ;
#40835 = EDGE_CURVE ( 'NONE', #34606, #19209, #7059, .T. ) ;
#40836 = CARTESIAN_POINT ( 'NONE',  ( 0.000000000000000000, -120.0000000000000000, 40.00000000000000711 ) ) ;
#40837 = EDGE_LOOP ( 'NONE', ( #39482, #47776, #13617, #32464 ) ) ;
#40838 = DIRECTION ( 'NONE',  ( -0.9227826878668540234, -0.3853207896976546531, 0.000000000000000000 ) ) ;
#40839 = ORIENTED_EDGE ( 'NONE', *, *, #13700, .F. ) ;
#40840 = EDGE_CURVE ( 'NONE', #23867, #39890, #28938, .T. ) ;
#40841 = DIRECTION ( 'NONE',  ( 0.000000000000000000, 0.5224985647159441360, 0.8526401643540952868 ) ) ;
#40842 = AXIS2_PLACEMENT_3D ( 'NONE', #19055, #38654, #20503 ) ;
#40843 = EDGE_CURVE ( 'NONE', #29618, #39337, #42597, .T. ) ;
#40844 = DIRECTION ( 'NONE',  ( 0.000000000000000000, 0.000000000000000000, 1.000000000000000000 ) ) ;
#40845 = DIRECTION ( 'NONE',  ( -1.000000000000000000, 0.000000000000000000, 0.000000000000000000 ) ) ;
#40846 = VERTEX_POINT ( 'NONE', #15918 ) ;
#40847 = ORIENTED_EDGE ( 'NONE', *, *, #826, .T. ) ;
#40848 = AXIS2_PLACEMENT_3D ( 'NONE', #32848, #43166, #17440 ) ;
#40849 = DIRECTION ( 'NONE',  ( 0.000000000000000000, -0.4539904997395350361, -0.8910065241883738940 ) ) ;
#40850 = DIRECTION ( 'NONE',  ( 0.000000000000000000, 0.000000000000000000, 1.000000000000000000 ) ) ;
#40851 = AXIS2_PLACEMENT_3D ( 'NONE', #12277, #19577, #41638 ) ;
#40852 = ORIENTED_EDGE ( 'NONE', *, *, #4912, .T. ) ;
#40853 = ORIENTED_EDGE ( 'NONE', *, *, #14087, .F. ) ;
#40854 = PLANE ( 'NONE',  #22879 ) ;
#40855 = CARTESIAN_POINT ( 'NONE',  ( 0.000000000000000000, 0.000000000000000000, 0.000000000000000000 ) ) ;
#40856 = VERTEX_POINT ( 'NONE', #43072 ) ;
#40857 = VECTOR ( 'NONE', #23947, 1000.000000000000000 ) ;
#40858 = CARTESIAN_POINT ( 'NONE',  ( -19.90058851926621841, -132.5883508287165853, -2.500000000000000000 ) ) ;
#40859 = CARTESIAN_POINT ( 'NONE',  ( 10.00000000000000000, -37.22597642581153821, 10.79786254984320415 ) ) ;
#40860 = CIRCLE ( 'NONE', #45527, 31.99999999999998579 ) ;
#40861 = CARTESIAN_POINT ( 'NONE',  ( 11.99999999999999822, 26.01480285779933510, -70.53064760720289428 ) ) ;
#40862 = CARTESIAN_POINT ( 'NONE',  ( 0.000000000000000000, -2.543863470248951320, 81.96053171279901051 ) ) ;
#40863 = DIRECTION ( 'NONE',  ( 0.000000000000000000, 1.000000000000000000, -9.787530781167598712E-16 ) ) ;
#40864 = CARTESIAN_POINT ( 'NONE',  ( 0.000000000000000000, -26.79245525562690844, -32.34446384430000876 ) ) ;
#40865 = AXIS2_PLACEMENT_3D ( 'NONE', #1061, #16010, #8643 ) ;
#40866 = DIRECTION ( 'NONE',  ( 0.9580045777625452175, 0.2867529058022035837, -0.000000000000000000 ) ) ;
#40867 = CARTESIAN_POINT ( 'NONE',  ( 10.00000000000000000, -2.663952781845854378, -41.91543099594820632 ) ) ;
#40868 = DIRECTION ( 'NONE',  ( 0.000000000000000000, -0.5877852522924802425, 0.8090169943749422332 ) ) ;
#40869 = VECTOR ( 'NONE', #14526, 1000.000000000000114 ) ;
#40870 = CARTESIAN_POINT ( 'NONE',  ( 0.000000000000000000, 0.000000000000000000, 0.000000000000000000 ) ) ;
#40871 = DIRECTION ( 'NONE',  ( 0.000000000000000000, 0.000000000000000000, 1.000000000000000000 ) ) ;
#40872 = FILL_AREA_STYLE ('',( #33034 ) ) ;
#40873 = CARTESIAN_POINT ( 'NONE',  ( 0.000000000000000000, 30.84782396557217865, 21.32104025579125306 ) ) ;
#40874 = ORIENTED_EDGE ( 'NONE', *, *, #13722, .F. ) ;
#40875 = ORIENTED_EDGE ( 'NONE', *, *, #5360, .F. ) ;
#40876 = EDGE_CURVE ( 'NONE', #41232, #9926, #15662, .T. ) ;
#40877 = PRODUCT_DEFINITION_CONTEXT ( 'detailed design', #6638, 'design' ) ;
#40878 = CARTESIAN_POINT ( 'NONE',  ( 10.00000000000000000, 36.72794159290334903, -65.59268652807170952 ) ) ;
#40879 = ADVANCED_FACE ( 'NONE', ( #16638 ), #38430, .T. ) ;
#40880 = VECTOR ( 'NONE', #30909, 1000.000000000000000 ) ;
#40881 = FACE_OUTER_BOUND ( 'NONE', #15769, .T. ) ;
#40882 = EDGE_CURVE ( 'NONE', #43246, #31653, #807, .T. ) ;
#40883 = VERTEX_POINT ( 'NONE', #16884 ) ;
#40884 = AXIS2_PLACEMENT_3D ( 'NONE', #31624, #15958, #38726 ) ;
#40885 = VERTEX_POINT ( 'NONE', #9288 ) ;
#40886 = DIRECTION ( 'NONE',  ( -1.000000000000000000, 0.000000000000000000, 0.000000000000000000 ) ) ;
#40887 = AXIS2_PLACEMENT_3D ( 'NONE', #28326, #33677, #33449 ) ;
#40888 = AXIS2_PLACEMENT_3D ( 'NONE', #20493, #35427, #16842 ) ;
#40889 = ORIENTED_EDGE ( 'NONE', *, *, #7050, .F. ) ;
#40890 = CARTESIAN_POINT ( 'NONE',  ( 23.11608002360578240, -124.4885236261218182, 5.500000000000000000 ) ) ;
#40891 = ORIENTED_EDGE ( 'NONE', *, *, #12173, .T. ) ;
#40892 = AXIS2_PLACEMENT_3D ( 'NONE', #12870, #31236, #8944 ) ;
#40893 = ORIENTED_EDGE ( 'NONE', *, *, #47022, .T. ) ;
#40894 = ORIENTED_EDGE ( 'NONE', *, *, #505, .F. ) ;
#40895 = ORIENTED_EDGE ( 'NONE', *, *, #12643, .T. ) ;
#40896 = DIRECTION ( 'NONE',  ( -1.000000000000000000, 0.000000000000000000, 0.000000000000000000 ) ) ;
#40897 = VECTOR ( 'NONE', #24191, 1000.000000000000000 ) ;
#40898 = EDGE_CURVE ( 'NONE', #24887, #17865, #5155, .T. ) ;
#40899 = EDGE_CURVE ( 'NONE', #27089, #44062, #1968, .T. ) ;
#40900 = DIRECTION ( 'NONE',  ( 0.000000000000000000, -0.000000000000000000, -1.000000000000000000 ) ) ;
#40901 = AXIS2_PLACEMENT_3D ( 'NONE', #33865, #340, #15291 ) ;
#40902 = ORIENTED_EDGE ( 'NONE', *, *, #13487, .T. ) ;
#40903 = EDGE_LOOP ( 'NONE', ( #30069, #26600, #41871, #47279 ) ) ;
#40904 = FACE_OUTER_BOUND ( 'NONE', #16085, .T. ) ;
#40905 = CIRCLE ( 'NONE', #8900, 31.99999999999998579 ) ;
#40906 = ORIENTED_EDGE ( 'NONE', *, *, #36315, .F. ) ;
#40907 = FACE_OUTER_BOUND ( 'NONE', #18103, .T. ) ;
#40908 = DIRECTION ( 'NONE',  ( -1.000000000000000000, -0.000000000000000000, 0.000000000000000000 ) ) ;
#40910 = ORIENTED_EDGE ( 'NONE', *, *, #19208, .T. ) ;
#40909 = AXIS2_PLACEMENT_3D ( 'NONE', #31215, #19934, #1350 ) ;
#40911 = CARTESIAN_POINT ( 'NONE',  ( 10.00000000000000000, 66.50666863322000211, 39.78640506895629869 ) ) ;
#40912 = DIRECTION ( 'NONE',  ( -1.000000000000000000, 0.000000000000000000, -0.000000000000000000 ) ) ;
#40913 = ORIENTED_EDGE ( 'NONE', *, *, #18880, .F. ) ;
#40914 = EDGE_CURVE ( 'NONE', #28215, #22790, #19552, .T. ) ;
#40915 = DIRECTION ( 'NONE',  ( 0.000000000000000000, 0.000000000000000000, -1.000000000000000000 ) ) ;
#40916 = DIRECTION ( 'NONE',  ( 0.000000000000000000, 0.000000000000000000, 1.000000000000000000 ) ) ;
#40917 = ORIENTED_EDGE ( 'NONE', *, *, #29390, .F. ) ;
#40918 = CARTESIAN_POINT ( 'NONE',  ( 0.000000000000000000, 0.000000000000000000, 40.00000000000000000 ) ) ;
#40919 = ORIENTED_EDGE ( 'NONE', *, *, #10924, .F. ) ;
#40920 = ORIENTED_EDGE ( 'NONE', *, *, #2466, .F. ) ;
#40921 = CARTESIAN_POINT ( 'NONE',  ( 0.000000000000000000, 0.000000000000000000, 0.000000000000000000 ) ) ;
#40922 = CARTESIAN_POINT ( 'NONE',  ( -3.000000000000000000, -4.261787119644969479, -26.19803753235780519 ) ) ;
#40923 = ORIENTED_EDGE ( 'NONE', *, *, #40256, .T. ) ;
#40924 = CARTESIAN_POINT ( 'NONE',  ( -6.880223345695647197, -142.5202692415819854, 5.500000000000000000 ) ) ;
#40925 = DIRECTION ( 'NONE',  ( 0.000000000000000000, 0.000000000000000000, 1.000000000000000000 ) ) ;
#40926 = CARTESIAN_POINT ( 'NONE',  ( 15.00000000000000000, -20.55727247249726020, 16.78983467731313084 ) ) ;
#40927 = DIRECTION ( 'NONE',  ( -0.000000000000000000, -0.000000000000000000, -1.000000000000000000 ) ) ;
#40928 = CARTESIAN_POINT ( 'NONE',  ( 12.00000000000000000, 23.49999999999999645, 1.499999999999995337 ) ) ;
#40929 = VECTOR ( 'NONE', #711, 1000.000000000000000 ) ;
#40930 = CARTESIAN_POINT ( 'NONE',  ( 0.000000000000000000, 0.000000000000000000, 12.50000000000000000 ) ) ;
#40931 = ORIENTED_EDGE ( 'NONE', *, *, #31936, .F. ) ;
#40932 = DIRECTION ( 'NONE',  ( -1.000000000000000000, -0.000000000000000000, 0.000000000000000000 ) ) ;
#40933 = CARTESIAN_POINT ( 'NONE',  ( 0.000000000000000000, 0.000000000000000000, 0.000000000000000000 ) ) ;
#40934 = DIRECTION ( 'NONE',  ( 0.000000000000000000, -0.8660254037844363761, 0.5000000000000038858 ) ) ;
#40935 = DIRECTION ( 'NONE',  ( 0.000000000000000000, 0.000000000000000000, 1.000000000000000000 ) ) ;
#40936 = AXIS2_PLACEMENT_3D ( 'NONE', #17964, #3041, #13585 ) ;
#40937 = VECTOR ( 'NONE', #44951, 1000.000000000000000 ) ;
#40938 = AXIS2_PLACEMENT_3D ( 'NONE', #42386, #46793, #17150 ) ;
#40939 = DIRECTION ( 'NONE',  ( 0.000000000000000000, 0.000000000000000000, -1.000000000000000000 ) ) ;
#40940 = DIRECTION ( 'NONE',  ( -1.000000000000000000, 0.000000000000000000, 0.000000000000000000 ) ) ;
#40941 = CARTESIAN_POINT ( 'NONE',  ( 10.00000000000000178, 0.000000000000000000, 12.50000000000000000 ) ) ;
#40942 = DIRECTION ( 'NONE',  ( 1.000000000000000000, -0.000000000000000000, -0.000000000000000000 ) ) ;
#40943 = ORIENTED_EDGE ( 'NONE', *, *, #18834, .T. ) ;
#40944 = EDGE_CURVE ( 'NONE', #33903, #1311, #22719, .T. ) ;
#40945 = DIRECTION ( 'NONE',  ( -1.000000000000000000, 0.000000000000000000, 0.000000000000000000 ) ) ;
#40946 = VECTOR ( 'NONE', #36352, 1000.000000000000114 ) ;
#40947 = ORIENTED_EDGE ( 'NONE', *, *, #11751, .F. ) ;
#40948 = AXIS2_PLACEMENT_3D ( 'NONE', #38716, #27686, #12516 ) ;
#40949 = LINE ( 'NONE', #29681, #43228 ) ;
#40950 = CIRCLE ( 'NONE', #24516, 31.99999999999999645 ) ;
#40951 = EDGE_CURVE ( 'NONE', #26872, #17933, #35478, .T. ) ;
#40952 = DIRECTION ( 'NONE',  ( 5.336177323473924868E-17, -3.796704924751176257E-16, -0.9999999999999998890 ) ) ;
#40953 = CARTESIAN_POINT ( 'NONE',  ( 12.00000000000000000, -18.13022148937242761, 15.02647892043569122 ) ) ;
#40954 = EDGE_CURVE ( 'NONE', #337, #22817, #69, .T. ) ;
#40955 = ORIENTED_EDGE ( 'NONE', *, *, #15355, .F. ) ;
#40956 = ORIENTED_EDGE ( 'NONE', *, *, #33453, .F. ) ;
#40957 = DIRECTION ( 'NONE',  ( 0.000000000000000000, 0.000000000000000000, -1.000000000000000000 ) ) ;
#40958 = VERTEX_POINT ( 'NONE', #13213 ) ;
#40959 = EDGE_CURVE ( 'NONE', #10988, #27800, #42344, .T. ) ;
#40960 = EDGE_CURVE ( 'NONE', #19441, #26557, #1473, .T. ) ;
#40961 = VECTOR ( 'NONE', #48039, 1000.000000000000000 ) ;
#40962 = VECTOR ( 'NONE', #8579, 1000.000000000000000 ) ;
#40963 = CARTESIAN_POINT ( 'NONE',  ( 10.00000000000000000, 37.48860685352291000, 0.8828120875901893649 ) ) ;
#40964 = EDGE_CURVE ( 'NONE', #46765, #24526, #38690, .T. ) ;
#40965 = DIRECTION ( 'NONE',  ( -0.000000000000000000, 0.7431448254773946882, -0.6691306063588577935 ) ) ;
#40966 = SHAPE_REPRESENTATION ( 'Shift Fork Lever Arm', ( #11636 ), #6986 ) ;
#40967 = AXIS2_PLACEMENT_3D ( 'NONE', #25917, #5964, #46830 ) ;
#40968 = VECTOR ( 'NONE', #46397, 1000.000000000000114 ) ;
#40969 = CARTESIAN_POINT ( 'NONE',  ( -21.33958957442910886, -129.9559990355020034, 5.500000000000000000 ) ) ;
#40970 = VECTOR ( 'NONE', #14324, 1000.000000000000000 ) ;
#40971 = ORIENTED_EDGE ( 'NONE', *, *, #28242, .F. ) ;
#40972 = CARTESIAN_POINT ( 'NONE',  ( 10.00000000000000000, -50.95692526931286181, -58.39081064771806240 ) ) ;
#40973 = ORIENTED_EDGE ( 'NONE', *, *, #17245, .T. ) ;
#40974 = DIRECTION ( 'NONE',  ( 0.000000000000000000, 0.9510565162951521989, 0.3090169943749515591 ) ) ;
#40975 = FACE_OUTER_BOUND ( 'NONE', #2308, .T. ) ;
#40976 = DIRECTION ( 'NONE',  ( 0.000000000000000000, 0.000000000000000000, 1.000000000000000000 ) ) ;
#40977 = EDGE_CURVE ( 'NONE', #23982, #35643, #24298, .T. ) ;
#40978 = DIRECTION ( 'NONE',  ( 0.000000000000000000, -0.7604059656000227152, -0.6494480483301933171 ) ) ;
#40979 = VECTOR ( 'NONE', #41307, 1000.000000000000114 ) ;
#40980 = VECTOR ( 'NONE', #6208, 1000.000000000000000 ) ;
#40981 = ORIENTED_EDGE ( 'NONE', *, *, #24021, .T. ) ;
#40982 = DIRECTION ( 'NONE',  ( -1.000000000000000000, 0.000000000000000000, 0.000000000000000000 ) ) ;
#40983 = ORIENTED_EDGE ( 'NONE', *, *, #7290, .T. ) ;
#40984 = ORIENTED_EDGE ( 'NONE', *, *, #19012, .F. ) ;
#40985 = FACE_OUTER_BOUND ( 'NONE', #12327, .T. ) ;
#40986 = AXIS2_PLACEMENT_3D ( 'NONE', #33711, #40824, #45228 ) ;
#40987 = CARTESIAN_POINT ( 'NONE',  ( 11.99999999999999822, 0.000000000000000000, 0.000000000000000000 ) ) ;
#40988 = CARTESIAN_POINT ( 'NONE',  ( 10.00000000000000000, -35.95386929396264009, 10.96151621346475658 ) ) ;
#40989 = CARTESIAN_POINT ( 'NONE',  ( 26.47460221209471598, -121.8961639463267090, 2.500000000000000000 ) ) ;
#40990 = ORIENTED_EDGE ( 'NONE', *, *, #12577, .F. ) ;
#40991 = DIRECTION ( 'NONE',  ( 1.000000000000000000, -0.000000000000000000, -0.000000000000000000 ) ) ;
#40992 = CARTESIAN_POINT ( 'NONE',  ( -3.702536634196119447, 8.043911037661890973, -45.00000000000000000 ) ) ;
#40993 = CARTESIAN_POINT ( 'NONE',  ( 6.000000000000000000, 76.69515212746016175, 29.01471420065590578 ) ) ;
#40994 = LINE ( 'NONE', #48084, #5651 ) ;
#40995 = CARTESIAN_POINT ( 'NONE',  ( -3.000000000000000000, -10.45096189432314837, -21.10159698893440350 ) ) ;
#40996 = CYLINDRICAL_SURFACE ( 'NONE', #26181, 16.00000000000000000 ) ;
#40997 = ORIENTED_EDGE ( 'NONE', *, *, #36734, .F. ) ;
#40998 = DIRECTION ( 'NONE',  ( 1.000000000000000000, 0.000000000000000000, 0.000000000000000000 ) ) ;
#40999 = DIRECTION ( 'NONE',  ( 0.8225049752423776450, 0.5687579148473764779, 0.000000000000000000 ) ) ;
#41001 = AXIS2_PLACEMENT_3D ( 'NONE', #11563, #3722, #8768 ) ;
#41000 = CARTESIAN_POINT ( 'NONE',  ( 10.00000000000000000, 37.16516213103285082, -4.992566952384588141 ) ) ;
#41002 = CARTESIAN_POINT ( 'NONE',  ( 10.00000000000000000, -55.20638768913797634, 51.02545421589302777 ) ) ;
#41003 = CARTESIAN_POINT ( 'NONE',  ( 6.000000000000000000, -8.966570791700160470, -81.50828551894237251 ) ) ;
#41004 = AXIS2_PLACEMENT_3D ( 'NONE', #44527, #32776, #25189 ) ;
#41005 = CARTESIAN_POINT ( 'NONE',  ( 10.00000000000000000, -4.992566952385247170, 37.16516213103275845 ) ) ;
#41006 = LINE ( 'NONE', #6980, #30033 ) ;
#41007 = CARTESIAN_POINT ( 'NONE',  ( 11.99999999999999822, 2.956366410620650420, 75.11725578898469280 ) ) ;
#41008 = CIRCLE ( 'NONE', #35547, 16.00000000000000000 ) ;
#41009 = CARTESIAN_POINT ( 'NONE',  ( 0.000000000000000000, 62.50329211542435104, 41.76937507738811917 ) ) ;
#41010 = VECTOR ( 'NONE', #27772, 1000.000000000000114 ) ;
#41011 = EDGE_CURVE ( 'NONE', #19725, #16756, #30858, .T. ) ;
#41012 = EDGE_CURVE ( 'NONE', #14039, #21975, #46209, .T. ) ;
#41013 = CARTESIAN_POINT ( 'NONE',  ( -10.94538922500103162, 0.000000000000000000, 13.90444123027096879 ) ) ;
#41014 = ORIENTED_EDGE ( 'NONE', *, *, #39230, .F. ) ;
#41015 = EDGE_CURVE ( 'NONE', #11748, #15250, #10012, .T. ) ;
#41016 = ORIENTED_EDGE ( 'NONE', *, *, #13925, .T. ) ;
#41017 = EDGE_LOOP ( 'NONE', ( #474, #32267, #21990, #25555 ) ) ;
#41018 = EDGE_CURVE ( 'NONE', #3149, #24941, #16508, .T. ) ;
#41019 = CIRCLE ( 'NONE', #47267, 82.00000000000000000 ) ;
#41020 = ADVANCED_FACE ( 'NONE', ( #32754 ), #32997, .T. ) ;
#41021 = AXIS2_PLACEMENT_3D ( 'NONE', #43278, #9738, #24677 ) ;
#41022 = CIRCLE ( 'NONE', #41709, 31.99999999999998934 ) ;
#41023 = FACE_OUTER_BOUND ( 'NONE', #12072, .T. ) ;
#41024 = VERTEX_POINT ( 'NONE', #36669 ) ;
#41025 = ORIENTED_EDGE ( 'NONE', *, *, #1669, .T. ) ;
#41026 = CIRCLE ( 'NONE', #19902, 77.49899999999999523 ) ;
#41027 = EDGE_CURVE ( 'NONE', #15680, #36155, #12596, .T. ) ;
#41028 = CARTESIAN_POINT ( 'NONE',  ( 10.00000000000000000, 0.000000000000000000, 0.000000000000000000 ) ) ;
#41029 = EDGE_CURVE ( 'NONE', #500, #19660, #43065, .T. ) ;
#41030 = APPLICATION_CONTEXT ( 'automotive_design' ) ;
#41031 = DIRECTION ( 'NONE',  ( -1.000000000000000000, -0.000000000000000000, -0.000000000000000000 ) ) ;
#41032 = DIRECTION ( 'NONE',  ( 0.7950889364178788110, -0.6064928550163524168, 0.000000000000000000 ) ) ;
#41033 = VERTEX_POINT ( 'NONE', #6828 ) ;
#41034 = DIRECTION ( 'NONE',  ( 0.000000000000000000, 0.000000000000000000, 1.000000000000000000 ) ) ;
#41035 = ORIENTED_EDGE ( 'NONE', *, *, #6251, .F. ) ;
#41036 = ORIENTED_EDGE ( 'NONE', *, *, #37626, .T. ) ;
#41037 = ORIENTED_EDGE ( 'NONE', *, *, #33483, .T. ) ;
#41038 = DIRECTION ( 'NONE',  ( -0.4796670183876317051, 0.8774505977381971134, 0.000000000000000000 ) ) ;
#41039 = DIRECTION ( 'NONE',  ( 0.000000000000000000, 0.000000000000000000, 1.000000000000000000 ) ) ;
#41040 = EDGE_CURVE ( 'NONE', #27843, #8199, #21950, .T. ) ;
#41042 = FACE_BOUND ( 'NONE', #23330, .T. ) ;
#41041 = VECTOR ( 'NONE', #31309, 1000.000000000000000 ) ;
#41043 = ORIENTED_EDGE ( 'NONE', *, *, #34907, .F. ) ;
#41044 = ORIENTED_EDGE ( 'NONE', *, *, #15154, .T. ) ;
#41045 = CYLINDRICAL_SURFACE ( 'NONE', #17724, 37.49900000000000233 ) ;
#41046 = ORIENTED_EDGE ( 'NONE', *, *, #39246, .T. ) ;
#41047 = CIRCLE ( 'NONE', #38712, 77.49899999999999523 ) ;
#41048 = CARTESIAN_POINT ( 'NONE',  ( 0.000000000000000000, -75.54627589209931671, -17.28742895386164591 ) ) ;
#41049 = DIRECTION ( 'NONE',  ( 0.000000000000000000, 0.7604059656000322631, -0.6494480483301821039 ) ) ;
#41050 = CARTESIAN_POINT ( 'NONE',  ( 0.000000000000000000, -51.02545421589285723, -55.20638768913812555 ) ) ;
#41051 = DIRECTION ( 'NONE',  ( 0.9435911131814398445, -0.3311129884571295534, 0.000000000000000000 ) ) ;
#41052 = DIRECTION ( 'NONE',  ( 0.000000000000000000, 0.000000000000000000, 1.000000000000000000 ) ) ;
#41053 = CARTESIAN_POINT ( 'NONE',  ( -0.2999999999999964362, 0.000000000000000000, -12.80000000000000071 ) ) ;
#41054 = DIRECTION ( 'NONE',  ( 0.000000000000000000, -6.982962677686266711E-15, 1.000000000000000000 ) ) ;
#41055 = SURFACE_SIDE_STYLE ('',( #48377 ) ) ;
#41056 = CARTESIAN_POINT ( 'NONE',  ( 0.000000000000000000, 46.53671651294032330, -59.03961581697353012 ) ) ;
#41057 = EDGE_LOOP ( 'NONE', ( #41315, #20349, #14845, #4505 ) ) ;
#41058 = EDGE_CURVE ( 'NONE', #42399, #28981, #39150, .T. ) ;
#41059 = CARTESIAN_POINT ( 'NONE',  ( 0.000000000000000000, 5.202137450156389953, 37.22597642581160216 ) ) ;
#41060 = AXIS2_PLACEMENT_3D ( 'NONE', #17219, #31461, #33128 ) ;
#41061 = CIRCLE ( 'NONE', #7430, 16.00000000000000000 ) ;
#41062 = ORIENTED_EDGE ( 'NONE', *, *, #8512, .F. ) ;
#41063 = CARTESIAN_POINT ( 'NONE',  ( 10.00000000000000000, 0.000000000000000000, 0.000000000000000000 ) ) ;
#41064 = VERTEX_POINT ( 'NONE', #40121 ) ;
#41065 = CIRCLE ( 'NONE', #21512, 37.49900000000000233 ) ;
#41066 = DIRECTION ( 'NONE',  ( 0.000000000000000000, 0.9238795325112877377, -0.3826834323650873948 ) ) ;
#41067 = ORIENTED_EDGE ( 'NONE', *, *, #40410, .F. ) ;
#41068 = DIRECTION ( 'NONE',  ( 0.000000000000000000, 0.9969173337331276308, 0.07845909572784864894 ) ) ;
#41069 = DIRECTION ( 'NONE',  ( 0.000000000000000000, 0.000000000000000000, 1.000000000000000000 ) ) ;
#41070 = CIRCLE ( 'NONE', #44969, 37.49900000000000944 ) ;
#41071 = FACE_OUTER_BOUND ( 'NONE', #37155, .T. ) ;
#41072 = CARTESIAN_POINT ( 'NONE',  ( 0.000000000000000000, 0.000000000000000000, 0.000000000000000000 ) ) ;
#41073 = DIRECTION ( 'NONE',  ( 0.000000000000000000, 0.000000000000000000, 1.000000000000000000 ) ) ;
#41074 = FACE_OUTER_BOUND ( 'NONE', #32333, .T. ) ;
#41075 = EDGE_LOOP ( 'NONE', ( #42794, #517, #24157, #9687 ) ) ;
#41076 = EDGE_CURVE ( 'NONE', #42450, #22226, #2408, .T. ) ;
#41077 = AXIS2_PLACEMENT_3D ( 'NONE', #21774, #39685, #10040 ) ;
#41078 = DIRECTION ( 'NONE',  ( 0.7273375899149802093, -0.6862798483830544471, 0.000000000000000000 ) ) ;
#41079 = DIRECTION ( 'NONE',  ( -1.000000000000000000, -0.000000000000000000, 0.000000000000000000 ) ) ;
#41080 = EDGE_CURVE ( 'NONE', #37160, #22256, #28371, .T. ) ;
#41081 = ORIENTED_EDGE ( 'NONE', *, *, #17097, .F. ) ;
#41082 = EDGE_CURVE ( 'NONE', #41996, #44807, #3130, .T. ) ;
#41083 = EDGE_LOOP ( 'NONE', ( #34330, #15161 ) ) ;
#41084 = VERTEX_POINT ( 'NONE', #24938 ) ;
#41085 = FACE_OUTER_BOUND ( 'NONE', #1897, .T. ) ;
#41086 = LINE ( 'NONE', #37394, #17520 ) ;
#41087 = ORIENTED_EDGE ( 'NONE', *, *, #42049, .F. ) ;
#41088 = AXIS2_PLACEMENT_3D ( 'NONE', #2723, #14720, #39942 ) ;
#41089 = AXIS2_PLACEMENT_3D ( 'NONE', #32598, #17900, #32825 ) ;
#41090 = DIRECTION ( 'NONE',  ( -1.000000000000000000, -0.000000000000000000, 0.000000000000000000 ) ) ;
#41091 = EDGE_LOOP ( 'NONE', ( #39521, #2124, #23934, #48238 ) ) ;
#41092 = AXIS2_PLACEMENT_3D ( 'NONE', #3536, #7691, #33400 ) ;
#41093 = VERTEX_POINT ( 'NONE', #36441 ) ;
#41094 = VECTOR ( 'NONE', #47109, 1000.000000000000000 ) ;
#41095 = AXIS2_PLACEMENT_3D ( 'NONE', #12736, #35239, #16889 ) ;
#41096 = DIRECTION ( 'NONE',  ( -0.000000000000000000, -0.6691306063588570163, 0.7431448254773953543 ) ) ;
#41097 = DIRECTION ( 'NONE',  ( -1.000000000000000000, -0.000000000000000000, 0.000000000000000000 ) ) ;
#41098 = VECTOR ( 'NONE', #47319, 1000.000000000000000 ) ;
#41099 = ORIENTED_EDGE ( 'NONE', *, *, #32063, .F. ) ;
#41100 = DIRECTION ( 'NONE',  ( -1.000000000000000000, -0.000000000000000000, -0.000000000000000000 ) ) ;
#41101 = VERTEX_POINT ( 'NONE', #47923 ) ;
#41102 = ORIENTED_EDGE ( 'NONE', *, *, #6221, .F. ) ;
#41103 = CARTESIAN_POINT ( 'NONE',  ( 0.000000000000000000, 35.91791733033570466, -68.67312586194960033 ) ) ;
#41104 = DIRECTION ( 'NONE',  ( -1.000000000000000000, 0.000000000000000000, 0.000000000000000000 ) ) ;
#41105 = CYLINDRICAL_SURFACE ( 'NONE', #40099, 31.99999999999998579 ) ;
#41106 = AXIS2_PLACEMENT_3D ( 'NONE', #23559, #30933, #35303 ) ;
#41107 = VERTEX_POINT ( 'NONE', #2654 ) ;
#41108 = ORIENTED_EDGE ( 'NONE', *, *, #17642, .T. ) ;
#41109 = CARTESIAN_POINT ( 'NONE',  ( 10.00000000000000000, 0.000000000000000000, 0.000000000000000000 ) ) ;
#41110 = CYLINDRICAL_SURFACE ( 'NONE', #38388, 77.49899999999999523 ) ;
#41111 = ORIENTED_EDGE ( 'NONE', *, *, #18687, .T. ) ;
#41112 = ORIENTED_EDGE ( 'NONE', *, *, #29464, .T. ) ;
#41113 = CYLINDRICAL_SURFACE ( 'NONE', #29127, 37.49900000000000233 ) ;
#41114 = EDGE_LOOP ( 'NONE', ( #16275, #19982, #23730, #33304 ) ) ;
#41115 = DIRECTION ( 'NONE',  ( 0.000000000000000000, 0.000000000000000000, 1.000000000000000000 ) ) ;
#41116 = CARTESIAN_POINT ( 'NONE',  ( 0.000000000000000000, 2.946379043146343246, 75.11764819372150725 ) ) ;
#41117 = LINE ( 'NONE', #11730, #24333 ) ;
#41118 = CARTESIAN_POINT ( 'NONE',  ( 0.000000000000000000, 35.38097989696528600, -12.42422080174602605 ) ) ;
#41119 = DIRECTION ( 'NONE',  ( 0.000000000000000000, -0.8526401643540970632, 0.5224985647159410274 ) ) ;
#41120 = DIRECTION ( 'NONE',  ( 1.000000000000000000, 0.000000000000000000, 0.000000000000000000 ) ) ;
#41121 = CARTESIAN_POINT ( 'NONE',  ( -25.00516449930816876, -111.2255058058861010, 2.500000000000000000 ) ) ;
#41122 = EDGE_CURVE ( 'NONE', #46691, #21034, #13694, .T. ) ;
#41123 = AXIS2_PLACEMENT_3D ( 'NONE', #42599, #8558, #9059 ) ;
#41124 = DIRECTION ( 'NONE',  ( -1.000000000000000000, 0.000000000000000000, -0.000000000000000000 ) ) ;
#41125 = CARTESIAN_POINT ( 'NONE',  ( -10.00000000000000000, 0.000000000000000000, 0.000000000000000000 ) ) ;
#41126 = EDGE_LOOP ( 'NONE', ( #13716, #27582, #38893, #32315 ) ) ;
#41127 = EDGE_CURVE ( 'NONE', #5676, #20033, #5542, .T. ) ;
#41128 = CARTESIAN_POINT ( 'NONE',  ( 12.69589495141918611, -96.69089767102708777, 5.500000000000000000 ) ) ;
#41129 = DIRECTION ( 'NONE',  ( -1.000000000000000000, 0.000000000000000000, 0.000000000000000000 ) ) ;
#41130 = EDGE_CURVE ( 'NONE', #17470, #25836, #21181, .T. ) ;
#41131 = CIRCLE ( 'NONE', #47343, 77.49900000000002365 ) ;
#41132 = CARTESIAN_POINT ( 'NONE',  ( 5.000000000000000000, -27.74655509720617275, -77.16300072079690153 ) ) ;
#41133 = EDGE_LOOP ( 'NONE', ( #22324, #22733, #16004, #42194 ) ) ;
#41134 = CIRCLE ( 'NONE', #20009, 77.49899999999999523 ) ;
#41135 = FACE_OUTER_BOUND ( 'NONE', #14361, .T. ) ;
#41136 = ADVANCED_FACE ( 'NONE', ( #10745 ), #25648, .T. ) ;
#41137 = VECTOR ( 'NONE', #21836, 999.9999999999998863 ) ;
#41138 = EDGE_CURVE ( 'NONE', #21018, #15597, #21743, .T. ) ;
#41139 = FACE_OUTER_BOUND ( 'NONE', #38692, .T. ) ;
#41140 = CIRCLE ( 'NONE', #47390, 82.00000000000000000 ) ;
#41141 = CARTESIAN_POINT ( 'NONE',  ( -3.000000000000000000, -23.29833615347109443, 3.418703333116492438 ) ) ;
#41142 = ORIENTED_EDGE ( 'NONE', *, *, #11218, .T. ) ;
#41143 = VECTOR ( 'NONE', #6858, 999.9999999999998863 ) ;
#41144 = DIRECTION ( 'NONE',  ( -1.000000000000000000, 0.000000000000000000, 0.000000000000000000 ) ) ;
#41145 = ORIENTED_EDGE ( 'NONE', *, *, #37012, .F. ) ;
#41146 = EDGE_CURVE ( 'NONE', #18512, #16815, #31381, .T. ) ;
#41147 = ORIENTED_EDGE ( 'NONE', *, *, #31764, .T. ) ;
#41148 = VERTEX_POINT ( 'NONE', #17341 ) ;
#41149 = ORIENTED_EDGE ( 'NONE', *, *, #45164, .F. ) ;
#41150 = LINE ( 'NONE', #7605, #20635 ) ;
#41151 = VECTOR ( 'NONE', #15861, 1000.000000000000000 ) ;
#41152 = CARTESIAN_POINT ( 'NONE',  ( 0.000000000000000000, 29.81001611431009479, 22.74946021919143391 ) ) ;
#41153 = EDGE_LOOP ( 'NONE', ( #6938, #2285, #3803, #30728 ) ) ;
#41154 = VERTEX_POINT ( 'NONE', #43554 ) ;
#41155 = ORIENTED_EDGE ( 'NONE', *, *, #38416, .T. ) ;
#41156 = CARTESIAN_POINT ( 'NONE',  ( 0.000000000000000000, 35.92658777277510040, 10.74501242461294659 ) ) ;
#41157 = EDGE_LOOP ( 'NONE', ( #47911, #7004, #9539, #45289 ) ) ;
#41158 = CIRCLE ( 'NONE', #5206, 31.99999999999998934 ) ;
#41159 = DIRECTION ( 'NONE',  ( -1.000000000000000000, 0.000000000000000000, 0.000000000000000000 ) ) ;
#41160 = DIRECTION ( 'NONE',  ( 0.000000000000000000, 0.5224985647159500202, -0.8526401643540915121 ) ) ;
#41161 = VERTEX_POINT ( 'NONE', #36192 ) ;
#41162 = ORIENTED_EDGE ( 'NONE', *, *, #10049, .T. ) ;
#41163 = DIRECTION ( 'NONE',  ( 0.000000000000000000, -0.5224985647159379187, -0.8526401643540989506 ) ) ;
#41164 = LINE ( 'NONE', #3700, #16918 ) ;
#41165 = ORIENTED_EDGE ( 'NONE', *, *, #7571, .T. ) ;
#41167 = ORIENTED_EDGE ( 'NONE', *, *, #33079, .T. ) ;
#41166 = LINE ( 'NONE', #26706, #9383 ) ;
#41168 = ADVANCED_FACE ( 'NONE', ( #13927 ), #28849, .T. ) ;
#41169 = DIRECTION ( 'NONE',  ( 1.000000000000000000, 0.000000000000000000, 0.000000000000000000 ) ) ;
#41170 = EDGE_LOOP ( 'NONE', ( #9389, #30782, #1417, #17678 ) ) ;
#41171 = AXIS2_PLACEMENT_3D ( 'NONE', #27386, #27625, #12227 ) ;
#41172 = CARTESIAN_POINT ( 'NONE',  ( -0.9515373497862389396, -96.47140937769621871, -5.500000000000000000 ) ) ;
#41173 = ORIENTED_EDGE ( 'NONE', *, *, #13214, .T. ) ;
#41174 = CARTESIAN_POINT ( 'NONE',  ( 11.99999999999999822, 66.50666863322000211, 39.78640506895628448 ) ) ;
#41175 = PLANE ( 'NONE',  #5178 ) ;
#41176 = ORIENTED_EDGE ( 'NONE', *, *, #7995, .F. ) ;
#41177 = EDGE_CURVE ( 'NONE', #44922, #47549, #7874, .T. ) ;
#41178 = DIRECTION ( 'NONE',  ( 0.000000000000000000, 0.000000000000000000, 1.000000000000000000 ) ) ;
#41179 = DIRECTION ( 'NONE',  ( -1.000000000000000000, 0.000000000000000000, 0.000000000000000000 ) ) ;
#41180 = DIRECTION ( 'NONE',  ( 0.000000000000000000, -0.4539904997395541875, 0.8910065241883642351 ) ) ;
#41181 = VECTOR ( 'NONE', #33463, 1000.000000000000000 ) ;
#41182 = ADVANCED_FACE ( 'NONE', ( #14893 ), #48412, .F. ) ;
#41183 = DIRECTION ( 'NONE',  ( -1.000000000000000000, 0.000000000000000000, 0.000000000000000000 ) ) ;
#41184 = CARTESIAN_POINT ( 'NONE',  ( 11.34017801569539685, -96.04900080221412395, 2.500000000000000000 ) ) ;
#41185 = CIRCLE ( 'NONE', #8359, 82.00000000000000000 ) ;
#41186 = CARTESIAN_POINT ( 'NONE',  ( 10.00000000000000000, 76.69515212746016175, 29.01471420065591289 ) ) ;
#41187 = DIRECTION ( 'NONE',  ( -1.000000000000000000, -0.000000000000000000, -0.000000000000000000 ) ) ;
#41188 = DIRECTION ( 'NONE',  ( 0.000000000000000000, 0.000000000000000000, 1.000000000000000000 ) ) ;
#41189 = CARTESIAN_POINT ( 'NONE',  ( 10.00000000000000000, -8.830959090341869100, -74.65491531819127147 ) ) ;
#41190 = PLANE ( 'NONE',  #5186 ) ;
#41191 = CARTESIAN_POINT ( 'NONE',  ( 5.000000000000000000, -33.71516098798792171, 74.74816331893418919 ) ) ;
#41192 = FACE_OUTER_BOUND ( 'NONE', #32770, .T. ) ;
#41193 = LINE ( 'NONE', #25993, #14699 ) ;
#41194 = ADVANCED_FACE ( 'NONE', ( #15143 ), #45467, .T. ) ;
#41195 = DIRECTION ( 'NONE',  ( -1.000000000000000000, 0.000000000000000000, 0.000000000000000000 ) ) ;
#41196 = ADVANCED_FACE ( 'NONE', ( #30070 ), #14660, .F. ) ;
#41197 = EDGE_LOOP ( 'NONE', ( #27769, #28438 ) ) ;
#41198 = EDGE_CURVE ( 'NONE', #35990, #39808, #34445, .T. ) ;
#41199 = CIRCLE ( 'NONE', #40416, 16.00000000000000000 ) ;
#41200 = LINE ( 'NONE', #33587, #7304 ) ;
#41201 = ORIENTED_EDGE ( 'NONE', *, *, #9850, .F. ) ;
#41202 = CARTESIAN_POINT ( 'NONE',  ( 12.00000000000000000, 22.07842321921480888, -8.187992925817425771 ) ) ;
#41203 = DIRECTION ( 'NONE',  ( 5.437773009819413426E-16, -6.230136962689586602E-16, 0.9999999999999997780 ) ) ;
#41204 = CIRCLE ( 'NONE', #16219, 42.00000000000000000 ) ;
#41205 = DIRECTION ( 'NONE',  ( -1.000000000000000000, 0.000000000000000000, -0.000000000000000000 ) ) ;
#41206 = ORIENTED_EDGE ( 'NONE', *, *, #7660, .T. ) ;
#41207 = LINE ( 'NONE', #10852, #36321 ) ;
#41208 = ORIENTED_EDGE ( 'NONE', *, *, #21048, .F. ) ;
#41209 = AXIS2_PLACEMENT_3D ( 'NONE', #6031, #35638, #17026 ) ;
#41210 = CARTESIAN_POINT ( 'NONE',  ( 0.000000000000000000, 0.000000000000000000, 0.000000000000000000 ) ) ;
#41211 = LINE ( 'NONE', #22834, #42212 ) ;
#41213 = ORIENTED_EDGE ( 'NONE', *, *, #20793, .F. ) ;
#41212 = DIRECTION ( 'NONE',  ( -1.000000000000000000, -0.000000000000000000, -0.000000000000000000 ) ) ;
#41214 = EDGE_LOOP ( 'NONE', ( #37124, #37956, #2682, #10754 ) ) ;
#41215 = FACE_OUTER_BOUND ( 'NONE', #28633, .T. ) ;
#41216 = CARTESIAN_POINT ( 'NONE',  ( 10.00000000000000000, 75.16055320797059380, -18.89407956138177269 ) ) ;
#41217 = CARTESIAN_POINT ( 'NONE',  ( 21.07894319797337701, -103.8699611390234878, 5.500000000000000000 ) ) ;
#41220 = ORIENTED_EDGE ( 'NONE', *, *, #35938, .F. ) ;
#41219 = CARTESIAN_POINT ( 'NONE',  ( 10.00000000000000000, 73.73191006444572793, -14.66109333815486515 ) ) ;
#41218 = AXIS2_PLACEMENT_3D ( 'NONE', #21395, #28979, #21646 ) ;
#41221 = EDGE_CURVE ( 'NONE', #8139, #13979, #26401, .T. ) ;
#41222 = ORIENTED_EDGE ( 'NONE', *, *, #10364, .T. ) ;
#41223 = LINE ( 'NONE', #4968, #19327 ) ;
#41224 = ORIENTED_EDGE ( 'NONE', *, *, #9196, .T. ) ;
#41225 = VERTEX_POINT ( 'NONE', #3874 ) ;
#41226 = DIRECTION ( 'NONE',  ( -1.000000000000000000, 0.000000000000000000, -0.000000000000000000 ) ) ;
#41227 = EDGE_CURVE ( 'NONE', #17771, #18736, #15613, .T. ) ;
#41228 = VECTOR ( 'NONE', #2169, 1000.000000000000000 ) ;
#41229 = FACE_OUTER_BOUND ( 'NONE', #5612, .T. ) ;
#41230 = DIRECTION ( 'NONE',  ( -1.000000000000000000, 0.000000000000000000, 0.000000000000000000 ) ) ;
#41231 = DIRECTION ( 'NONE',  ( -1.000000000000000000, 0.000000000000000000, -0.000000000000000000 ) ) ;
#41232 = VERTEX_POINT ( 'NONE', #44504 ) ;
#41233 = LINE ( 'NONE', #90, #9637 ) ;
#41234 = EDGE_CURVE ( 'NONE', #45891, #22916, #11021, .T. ) ;
#41235 = CARTESIAN_POINT ( 'NONE',  ( 10.00000000000000000, -37.01155633439053361, -6.555932627142825986 ) ) ;
#41236 = DIRECTION ( 'NONE',  ( -1.000000000000000000, 0.000000000000000000, 0.000000000000000000 ) ) ;
#41237 = DIRECTION ( 'NONE',  ( -0.000000000000000000, 0.8090169943749426773, -0.5877852522924796874 ) ) ;
#41238 = CARTESIAN_POINT ( 'NONE',  ( -19.90058851926621131, -132.5883508287165853, 5.500000000000000000 ) ) ;
#41239 = VECTOR ( 'NONE', #27695, 1000.000000000000227 ) ;
#41240 = CARTESIAN_POINT ( 'NONE',  ( 5.000000000000000000, -39.04073710021356192, 15.48615015657568073 ) ) ;
#41241 = CYLINDRICAL_SURFACE ( 'NONE', #23216, 82.00000000000000000 ) ;
#41242 = CARTESIAN_POINT ( 'NONE',  ( 1.250000000000000000, -12.36245420541525597, 0.000000000000000000 ) ) ;
#41243 = DIRECTION ( 'NONE',  ( -1.000000000000000000, 0.000000000000000000, -0.000000000000000000 ) ) ;
#41244 = LINE ( 'NONE', #7211, #3389 ) ;
#41245 = EDGE_CURVE ( 'NONE', #40727, #44946, #18031, .T. ) ;
#41246 = EDGE_CURVE ( 'NONE', #5318, #24524, #9443, .T. ) ;
#41247 = DIRECTION ( 'NONE',  ( -1.000000000000000000, 0.000000000000000000, 0.000000000000000000 ) ) ;
#41248 = DIRECTION ( 'NONE',  ( -1.000000000000000000, -0.000000000000000000, -0.000000000000000000 ) ) ;
#41249 = CARTESIAN_POINT ( 'NONE',  ( 10.00000000000000000, 36.88895765772633695, 6.736453364083687667 ) ) ;
#41250 = CYLINDRICAL_SURFACE ( 'NONE', #8277, 31.99999999999998579 ) ;
#41251 = CARTESIAN_POINT ( 'NONE',  ( 10.00000000000000000, 68.67312586195046720, -35.91791733033402068 ) ) ;
#41252 = DIRECTION ( 'NONE',  ( -1.000000000000000000, 0.000000000000000000, 0.000000000000000000 ) ) ;
#41253 = ORIENTED_EDGE ( 'NONE', *, *, #9905, .T. ) ;
#41254 = ORIENTED_EDGE ( 'NONE', *, *, #6264, .F. ) ;
#41255 = EDGE_CURVE ( 'NONE', #37523, #14949, #7296, .T. ) ;
#41256 = CIRCLE ( 'NONE', #20137, 16.00000000000000000 ) ;
#41257 = ORIENTED_EDGE ( 'NONE', *, *, #45642, .T. ) ;
#41258 = ORIENTED_EDGE ( 'NONE', *, *, #3128, .T. ) ;
#41259 = VERTEX_POINT ( 'NONE', #22955 ) ;
#41260 = CIRCLE ( 'NONE', #22522, 31.99999999999998224 ) ;
#41261 = DIRECTION ( 'NONE',  ( 0.000000000000000000, 0.000000000000000000, 1.000000000000000000 ) ) ;
#41262 = ORIENTED_EDGE ( 'NONE', *, *, #16403, .T. ) ;
#41263 = DIRECTION ( 'NONE',  ( 0.000000000000000000, 0.000000000000000000, 1.000000000000000000 ) ) ;
#41264 = VERTEX_POINT ( 'NONE', #10975 ) ;
#41265 = CARTESIAN_POINT ( 'NONE',  ( 15.00000000000000000, -22.67460108101782978, -6.353146135317906840 ) ) ;
#41266 = DIRECTION ( 'NONE',  ( 0.6064928550163524168, 0.7950889364178788110, 0.000000000000000000 ) ) ;
#41267 = VERTEX_POINT ( 'NONE', #33486 ) ;
#41268 = DIRECTION ( 'NONE',  ( 1.000000000000000000, 0.000000000000000000, 0.000000000000000000 ) ) ;
#41269 = ORIENTED_EDGE ( 'NONE', *, *, #30510, .F. ) ;
#41270 = ORIENTED_EDGE ( 'NONE', *, *, #40677, .T. ) ;
#41271 = VERTEX_POINT ( 'NONE', #33966 ) ;
#41272 = DIRECTION ( 'NONE',  ( 0.000000000000000000, 0.8526401643540936215, -0.5224985647159469115 ) ) ;
#41273 = LINE ( 'NONE', #22656, #25117 ) ;
#41274 = AXIS2_PLACEMENT_3D ( 'NONE', #30745, #8222, #23153 ) ;
#41275 = DIRECTION ( 'NONE',  ( -1.000000000000000000, -0.000000000000000000, -0.000000000000000000 ) ) ;
#41276 = ORIENTED_EDGE ( 'NONE', *, *, #24319, .F. ) ;
#41277 = ORIENTED_EDGE ( 'NONE', *, *, #25003, .T. ) ;
#41278 = VERTEX_POINT ( 'NONE', #48181 ) ;
#41279 = DIRECTION ( 'NONE',  ( -1.000000000000000000, -0.000000000000000000, -0.000000000000000000 ) ) ;
#41280 = ORIENTED_EDGE ( 'NONE', *, *, #30399, .T. ) ;
#41281 = FACE_OUTER_BOUND ( 'NONE', #39353, .T. ) ;
#41282 = EDGE_CURVE ( 'NONE', #26682, #36257, #36790, .T. ) ;
#41283 = LINE ( 'NONE', #10932, #47507 ) ;
#41284 = CARTESIAN_POINT ( 'NONE',  ( 0.000000000000000000, 0.000000000000000000, 0.000000000000000000 ) ) ;
#41285 = CARTESIAN_POINT ( 'NONE',  ( 0.000000000000000000, -34.44570377933549565, -69.42325613327476219 ) ) ;
#41286 = CARTESIAN_POINT ( 'NONE',  ( 10.00000000000000000, 0.000000000000000000, 0.000000000000000000 ) ) ;
#41287 = CARTESIAN_POINT ( 'NONE',  ( 0.000000000000000000, 0.000000000000000000, 0.000000000000000000 ) ) ;
#41288 = EDGE_CURVE ( 'NONE', #31890, #7607, #13369, .T. ) ;
#41289 = LINE ( 'NONE', #7744, #9235 ) ;
#41290 = VERTEX_POINT ( 'NONE', #41569 ) ;
#41291 = DIRECTION ( 'NONE',  ( 0.000000000000000000, -0.8090169943749530024, 0.5877852522924653655 ) ) ;
#41292 = CARTESIAN_POINT ( 'NONE',  ( 0.000000000000000000, 81.90746397400387480, 3.894527615418187150 ) ) ;
#41293 = ORIENTED_EDGE ( 'NONE', *, *, #21484, .T. ) ;
#41294 = DIRECTION ( 'NONE',  ( 0.1850432970638682395, -0.9827303690289279636, 0.000000000000000000 ) ) ;
#41295 = VECTOR ( 'NONE', #9534, 1000.000000000000000 ) ;
#41296 = VERTEX_POINT ( 'NONE', #21981 ) ;
#41297 = EDGE_CURVE ( 'NONE', #38237, #14425, #44628, .T. ) ;
#41298 = FACE_OUTER_BOUND ( 'NONE', #1250, .T. ) ;
#41299 = DIRECTION ( 'NONE',  ( 0.000000000000000000, 0.000000000000000000, 1.000000000000000000 ) ) ;
#41300 = CARTESIAN_POINT ( 'NONE',  ( -32.50000000000000000, -120.0000000000000000, 2.500000000000000000 ) ) ;
#41301 = DIRECTION ( 'NONE',  ( 0.1276937514489679681, 0.9918136447140103451, 0.000000000000000000 ) ) ;
#41302 = CIRCLE ( 'NONE', #25626, 82.00000000000000000 ) ;
#41303 = EDGE_CURVE ( 'NONE', #7858, #41627, #19033, .T. ) ;
#41304 = CARTESIAN_POINT ( 'NONE',  ( 0.000000000000000000, 0.000000000000000000, 0.000000000000000000 ) ) ;
#41305 = FACE_OUTER_BOUND ( 'NONE', #13612, .T. ) ;
#41306 = FACE_OUTER_BOUND ( 'NONE', #41214, .T. ) ;
#41307 = DIRECTION ( 'NONE',  ( 0.6516173805718079581, -0.7585478161175704948, 0.000000000000000000 ) ) ;
#41308 = EDGE_CURVE ( 'NONE', #6665, #13155, #5575, .T. ) ;
#41309 = FACE_OUTER_BOUND ( 'NONE', #40209, .T. ) ;
#41310 = CYLINDRICAL_SURFACE ( 'NONE', #39363, 42.00000000000000000 ) ;
#41311 = ORIENTED_EDGE ( 'NONE', *, *, #37032, .F. ) ;
#41312 = ORIENTED_EDGE ( 'NONE', *, *, #14530, .F. ) ;
#41313 = CIRCLE ( 'NONE', #15519, 31.99999999999998934 ) ;
#41314 = EDGE_CURVE ( 'NONE', #8938, #14976, #23933, .T. ) ;
#41315 = ORIENTED_EDGE ( 'NONE', *, *, #21935, .T. ) ;
#41316 = ORIENTED_EDGE ( 'NONE', *, *, #12779, .F. ) ;
#41317 = PLANE ( 'NONE',  #17888 ) ;
#41318 = LINE ( 'NONE', #33951, #39451 ) ;
#41319 = VERTEX_POINT ( 'NONE', #12434 ) ;
#41320 = ORIENTED_EDGE ( 'NONE', *, *, #2409, .F. ) ;
#41321 = EDGE_CURVE ( 'NONE', #34109, #39765, #43897, .T. ) ;
#41322 = FACE_OUTER_BOUND ( 'NONE', #47940, .T. ) ;
#41323 = AXIS2_PLACEMENT_3D ( 'NONE', #18300, #14401, #25399 ) ;
#41324 = ORIENTED_EDGE ( 'NONE', *, *, #4809, .F. ) ;
#41325 = ORIENTED_EDGE ( 'NONE', *, *, #39518, .F. ) ;
#41326 = AXIS2_PLACEMENT_3D ( 'NONE', #35193, #43519, #31306 ) ;
#41327 = AXIS2_PLACEMENT_3D ( 'NONE', #9903, #17473, #29223 ) ;
#41328 = DIRECTION ( 'NONE',  ( 0.000000000000000000, 0.000000000000000000, 1.000000000000000000 ) ) ;
#41330 = VERTEX_POINT ( 'NONE', #16830 ) ;
#41329 = CARTESIAN_POINT ( 'NONE',  ( 0.000000000000000000, -0.8299999999999999600, -1.199999999999999956 ) ) ;
#41331 = DIRECTION ( 'NONE',  ( 0.000000000000000000, 0.000000000000000000, 1.000000000000000000 ) ) ;
#41332 = ORIENTED_EDGE ( 'NONE', *, *, #28126, .T. ) ;
#41333 = CARTESIAN_POINT ( 'NONE',  ( 0.000000000000000000, -55.16347631942998220, -60.67117009219196433 ) ) ;
#41334 = ORIENTED_EDGE ( 'NONE', *, *, #31623, .F. ) ;
#41335 = ORIENTED_EDGE ( 'NONE', *, *, #36284, .F. ) ;
#41336 = ADVANCED_FACE ( 'NONE', ( #34939 ), #27601, .F. ) ;
#41337 = DIRECTION ( 'NONE',  ( 0.000000000000000000, -0.9969173337331271867, -0.07845909572785568498 ) ) ;
#41338 = ADVANCED_FACE ( 'NONE', ( #1652 ), #31783, .F. ) ;
#41339 = DIRECTION ( 'NONE',  ( 0.000000000000000000, 0.000000000000000000, 1.000000000000000000 ) ) ;
#41340 = DIRECTION ( 'NONE',  ( -0.000000000000000000, 0.8090169943749426773, 0.5877852522924797984 ) ) ;
#41341 = CARTESIAN_POINT ( 'NONE',  ( 10.00000000000000000, -6.736453364083292428, -36.88895765772640800 ) ) ;
#41342 = ORIENTED_EDGE ( 'NONE', *, *, #25275, .T. ) ;
#41343 = EDGE_CURVE ( 'NONE', #33371, #20366, #1419, .T. ) ;
#41344 = VERTEX_POINT ( 'NONE', #20006 ) ;
#41345 = STYLED_ITEM ( 'NONE', ( #17320 ), #47339 ) ;
#41346 = CARTESIAN_POINT ( 'NONE',  ( 10.00000000000000000, -25.88420570971381807, -27.13269053701123212 ) ) ;
#41347 = DIRECTION ( 'NONE',  ( -1.000000000000000000, -0.000000000000000000, 0.000000000000000000 ) ) ;
#41348 = EDGE_LOOP ( 'NONE', ( #25119, #42979, #35420, #7955 ) ) ;
#41349 = ORIENTED_EDGE ( 'NONE', *, *, #20665, .T. ) ;
#41350 = EDGE_CURVE ( 'NONE', #44417, #39726, #42053, .T. ) ;
#41351 = DIRECTION ( 'NONE',  ( 0.000000000000000000, 0.000000000000000000, 1.000000000000000000 ) ) ;
#41352 = VERTEX_POINT ( 'NONE', #16117 ) ;
#41353 = DIRECTION ( 'NONE',  ( 0.000000000000000000, 0.000000000000000000, 1.000000000000000000 ) ) ;
#41354 = DIRECTION ( 'NONE',  ( 0.8225049752423786442, 0.5687579148473752566, -0.000000000000000000 ) ) ;
#41355 = DIRECTION ( 'NONE',  ( -1.000000000000000000, 0.000000000000000000, 0.000000000000000000 ) ) ;
#41356 = CARTESIAN_POINT ( 'NONE',  ( 11.99999999999999822, 0.000000000000000000, 0.000000000000000000 ) ) ;
#41357 = LINE ( 'NONE', #8045, #42401 ) ;
#41358 = DIRECTION ( 'NONE',  ( -1.000000000000000000, -0.000000000000000000, 0.000000000000000000 ) ) ;
#41359 = DIRECTION ( 'NONE',  ( 0.000000000000000000, -0.1564344650402381132, 0.9876883405951365491 ) ) ;
#41360 = CARTESIAN_POINT ( 'NONE',  ( -20.30386590532152979, -102.9045904027214959, 5.500000000000000000 ) ) ;
#41361 = VECTOR ( 'NONE', #19272, 1000.000000000000000 ) ;
#41362 = CARTESIAN_POINT ( 'NONE',  ( -12.49999999999999645, 0.000000000000000000, -56.19999999999998863 ) ) ;
#41363 = ORIENTED_EDGE ( 'NONE', *, *, #47943, .F. ) ;
#41364 = DIRECTION ( 'NONE',  ( 0.000000000000000000, -0.3090169943749549453, 0.9510565162951511997 ) ) ;
#41365 = LINE ( 'NONE', #37679, #18359 ) ;
#41366 = CIRCLE ( 'NONE', #34314, 42.00000000000000000 ) ;
#41367 = CARTESIAN_POINT ( 'NONE',  ( 6.782329983125267248, 10.49999999999999645, -125.0000000000000000 ) ) ;
#41368 = EDGE_LOOP ( 'NONE', ( #44576, #28207, #43948, #35194, #28137 ) ) ;
#41369 = EDGE_CURVE ( 'NONE', #31484, #37160, #35269, .T. ) ;
#41370 = UNCERTAINTY_MEASURE_WITH_UNIT (LENGTH_MEASURE( 1.000000000000000082E-05 ), #26605, 'distance_accuracy_value', 'NONE');
#41371 = DIRECTION ( 'NONE',  ( 1.000000000000000000, 0.000000000000000000, 0.000000000000000000 ) ) ;
#41372 = AXIS2_PLACEMENT_3D ( 'NONE', #2618, #13418, #2388 ) ;
#41373 = LINE ( 'NONE', #11745, #29038 ) ;
#41374 = ADVANCED_FACE ( 'NONE', ( #34437 ), #46449, .T. ) ;
#41375 = DIRECTION ( 'NONE',  ( -1.000000000000000000, 0.000000000000000000, 0.000000000000000000 ) ) ;
#41376 = EDGE_LOOP ( 'NONE', ( #20005, #27529, #23636, #13725 ) ) ;
#41377 = DIRECTION ( 'NONE',  ( -1.000000000000000000, 0.000000000000000000, 0.000000000000000000 ) ) ;
#41378 = EDGE_LOOP ( 'NONE', ( #33202, #19735, #32414, #20343 ) ) ;
#41379 = VERTEX_POINT ( 'NONE', #38374 ) ;
#41380 = ORIENTED_EDGE ( 'NONE', *, *, #3062, .T. ) ;
#41381 = VERTEX_POINT ( 'NONE', #42536 ) ;
#41382 = VECTOR ( 'NONE', #3716, 1000.000000000000000 ) ;
#41383 = CYLINDRICAL_SURFACE ( 'NONE', #26614, 31.99999999999998579 ) ;
#41385 = ORIENTED_EDGE ( 'NONE', *, *, #11007, .F. ) ;
#41384 = VECTOR ( 'NONE', #29999, 1000.000000000000000 ) ;
#41386 = ORIENTED_EDGE ( 'NONE', *, *, #28749, .F. ) ;
#41387 = EDGE_CURVE ( 'NONE', #38308, #3149, #21209, .T. ) ;
#41388 = DIRECTION ( 'NONE',  ( 0.000000000000000000, -0.1564344650402170744, -0.9876883405951399908 ) ) ;
#41389 = ORIENTED_EDGE ( 'NONE', *, *, #39947, .T. ) ;
#41390 = CIRCLE ( 'NONE', #32742, 16.00000000000000000 ) ;
#41391 = DIRECTION ( 'NONE',  ( -1.000000000000000000, 0.000000000000000000, 0.000000000000000000 ) ) ;
#41392 = ADVANCED_FACE ( 'NONE', ( #4842 ), #20483, .T. ) ;
#41393 = DIRECTION ( 'NONE',  ( 0.000000000000000000, 0.000000000000000000, -1.000000000000000000 ) ) ;
#41394 = ORIENTED_EDGE ( 'NONE', *, *, #37181, .F. ) ;
#41395 = DIRECTION ( 'NONE',  ( -1.000000000000000000, 0.000000000000000000, 0.000000000000000000 ) ) ;
#41396 = CARTESIAN_POINT ( 'NONE',  ( 15.00000000000000000, -3.948201729842032215, 23.21447184625297666 ) ) ;
#41397 = ORIENTED_EDGE ( 'NONE', *, *, #1455, .T. ) ;
#41398 = DIRECTION ( 'NONE',  ( -1.000000000000000000, 0.000000000000000000, -0.000000000000000000 ) ) ;
#41399 = LINE ( 'NONE', #29417, #31345 ) ;
#41400 = ORIENTED_EDGE ( 'NONE', *, *, #12599, .T. ) ;
#41401 = CARTESIAN_POINT ( 'NONE',  ( 11.99999999999999822, -39.78640506895651896, 66.50666863321988842 ) ) ;
#41402 = ORIENTED_EDGE ( 'NONE', *, *, #19165, .F. ) ;
#41403 = ORIENTED_EDGE ( 'NONE', *, *, #48081, .F. ) ;
#41404 = ADVANCED_FACE ( 'NONE', ( #8743 ), #34685, .T. ) ;
#41405 = LINE ( 'NONE', #30879, #39319 ) ;
#41406 = DIRECTION ( 'NONE',  ( -1.000000000000000000, 0.000000000000000000, 0.000000000000000000 ) ) ;
#41407 = DIRECTION ( 'NONE',  ( -1.000000000000000000, -0.000000000000000000, 0.000000000000000000 ) ) ;
#41408 = EDGE_CURVE ( 'NONE', #48128, #17814, #26679, .T. ) ;
#41409 = DIRECTION ( 'NONE',  ( 0.000000000000000000, 0.4539904997395414754, 0.8910065241883706744 ) ) ;
#41410 = CARTESIAN_POINT ( 'NONE',  ( 11.99999999999999822, 68.55367621811204515, -44.99326035065983120 ) ) ;
#41411 = DIRECTION ( 'NONE',  ( 0.000000000000000000, 0.000000000000000000, 1.000000000000000000 ) ) ;
#41412 = CARTESIAN_POINT ( 'NONE',  ( 4.250000000000000000, -13.95926121303099343, -1.199999999999999956 ) ) ;
#41413 = LINE ( 'NONE', #10595, #22357 ) ;
#41414 = CARTESIAN_POINT ( 'NONE',  ( 0.000000000000000000, 17.80606268964585226, -33.00180498840028775 ) ) ;
#41415 = CARTESIAN_POINT ( 'NONE',  ( 0.000000000000000000, -30.00120703465222149, 22.64427369931158296 ) ) ;
#41416 = LINE ( 'NONE', #7640, #17003 ) ;
#41417 = FACE_BOUND ( 'NONE', #24280, .T. ) ;
#41418 = CYLINDRICAL_SURFACE ( 'NONE', #38549, 31.99999999999998579 ) ;
#41419 = CARTESIAN_POINT ( 'NONE',  ( 12.00000000000000000, 20.85821328998756385, 10.92862929874494249 ) ) ;
#41420 = DIRECTION ( 'NONE',  ( -1.000000000000000000, 0.000000000000000000, 0.000000000000000000 ) ) ;
#41421 = CARTESIAN_POINT ( 'NONE',  ( -3.000000000000000000, 5.835314593368772229, -22.81335362449846826 ) ) ;
#41422 = VERTEX_POINT ( 'NONE', #45967 ) ;
#41423 = ORIENTED_EDGE ( 'NONE', *, *, #28463, .F. ) ;
#41424 = VECTOR ( 'NONE', #44211, 1000.000000000000000 ) ;
#41425 = CARTESIAN_POINT ( 'NONE',  ( 5.000000000000002665, 21.60688246758586217, 79.10210256391376049 ) ) ;
#41426 = CIRCLE ( 'NONE', #23450, 82.00000000000000000 ) ;
#41427 = ORIENTED_EDGE ( 'NONE', *, *, #7177, .F. ) ;
#41428 = DIRECTION ( 'NONE',  ( 0.000000000000000000, 0.6494480483301849905, -0.7604059656000299317 ) ) ;
#41429 = VECTOR ( 'NONE', #40300, 1000.000000000000000 ) ;
#41430 = DIRECTION ( 'NONE',  ( 0.000000000000000000, -2.775557561562891351E-17, 1.000000000000000000 ) ) ;
#41431 = CARTESIAN_POINT ( 'NONE',  ( 10.00000000000000000, 16.95692799528845640, -2.500000000000000000 ) ) ;
#41432 = ORIENTED_EDGE ( 'NONE', *, *, #33102, .T. ) ;
#41433 = AXIS2_PLACEMENT_3D ( 'NONE', #6305, #21217, #2607 ) ;
#41434 = AXIS2_PLACEMENT_3D ( 'NONE', #45534, #11774, #4904 ) ;
#41435 = EDGE_CURVE ( 'NONE', #41545, #15919, #14977, .T. ) ;
#41436 = ORIENTED_EDGE ( 'NONE', *, *, #36737, .F. ) ;
#41437 = DIRECTION ( 'NONE',  ( -1.000000000000000000, 0.000000000000000000, 0.000000000000000000 ) ) ;
#41438 = ORIENTED_EDGE ( 'NONE', *, *, #17789, .T. ) ;
#41439 = PLANE ( 'NONE',  #19065 ) ;
#41440 = DIRECTION ( 'NONE',  ( 1.000000000000000000, -0.000000000000000000, -0.000000000000000000 ) ) ;
#41442 = ORIENTED_EDGE ( 'NONE', *, *, #8538, .T. ) ;
#41441 = DIRECTION ( 'NONE',  ( -1.000000000000000000, -0.000000000000000000, -0.000000000000000000 ) ) ;
#41443 = VERTEX_POINT ( 'NONE', #23202 ) ;
#41444 = EDGE_CURVE ( 'NONE', #8400, #390, #47757, .T. ) ;
#41445 = EDGE_CURVE ( 'NONE', #23147, #16520, #14164, .T. ) ;
#41446 = EDGE_CURVE ( 'NONE', #27599, #14155, #34483, .T. ) ;
#41447 = CARTESIAN_POINT ( 'NONE',  ( -10.00000000000000000, 0.000000000000000000, 0.000000000000000000 ) ) ;
#41448 = CARTESIAN_POINT ( 'NONE',  ( 15.00000000000000000, 16.61724383029390140, 20.69703378468902955 ) ) ;
#41449 = FACE_OUTER_BOUND ( 'NONE', #17658, .T. ) ;
#41450 = CIRCLE ( 'NONE', #21105, 82.00000000000000000 ) ;
#41451 = DIRECTION ( 'NONE',  ( 0.000000000000000000, -0.3090169943749549453, 0.9510565162951511997 ) ) ;
#41452 = ORIENTED_EDGE ( 'NONE', *, *, #34295, .T. ) ;
#41453 = CARTESIAN_POINT ( 'NONE',  ( 10.00000000000000000, -17.80606268964516659, -33.00180498840066434 ) ) ;
#41454 = ORIENTED_EDGE ( 'NONE', *, *, #16091, .F. ) ;
#41455 = ORIENTED_EDGE ( 'NONE', *, *, #2709, .T. ) ;
#41456 = ADVANCED_FACE ( 'NONE', ( #17537 ), #13154, .F. ) ;
#41457 = CARTESIAN_POINT ( 'NONE',  ( 10.00000000000000000, 76.41127070299292257, -12.93880638057232346 ) ) ;
#41458 = AXIS2_PLACEMENT_3D ( 'NONE', #10646, #28759, #47369 ) ;
#41459 = AXIS2_PLACEMENT_3D ( 'NONE', #11529, #26454, #30374 ) ;
#41460 = CARTESIAN_POINT ( 'NONE',  ( 10.00000000000000000, -0.6853352020787742971, -37.58145647212455032 ) ) ;
#41461 = EDGE_CURVE ( 'NONE', #5896, #12471, #36831, .T. ) ;
#41462 = CARTESIAN_POINT ( 'NONE',  ( 10.00000000000000000, -46.54456581323847786, 59.03342792756247093 ) ) ;
#41463 = LINE ( 'NONE', #22382, #13368 ) ;
#41464 = ORIENTED_EDGE ( 'NONE', *, *, #40369, .F. ) ;
#41465 = CARTESIAN_POINT ( 'NONE',  ( 0.000000000000000000, -33.79645857604525361, 16.45098606841114730 ) ) ;
#41466 = CARTESIAN_POINT ( 'NONE',  ( 0.000000000000000000, -31.46837873495025306, 68.27212725128265447 ) ) ;
#41467 = AXIS2_PLACEMENT_3D ( 'NONE', #31156, #5679, #5935 ) ;
#41468 = DIRECTION ( 'NONE',  ( 0.2867529058022035837, -0.9580045777625452175, 0.000000000000000000 ) ) ;
#41469 = AXIS2_PLACEMENT_3D ( 'NONE', #3960, #15230, #22797 ) ;
#41470 = DIRECTION ( 'NONE',  ( 0.000000000000000000, 0.000000000000000000, 1.000000000000000000 ) ) ;
#41471 = CARTESIAN_POINT ( 'NONE',  ( 0.000000000000000000, 0.000000000000000000, 0.000000000000000000 ) ) ;
#41472 = VECTOR ( 'NONE', #24475, 1000.000000000000000 ) ;
#41473 = CARTESIAN_POINT ( 'NONE',  ( 10.00000000000000000, 26.01480285779933510, -70.53064760720289428 ) ) ;
#41474 = DIRECTION ( 'NONE',  ( 0.000000000000000000, -0.5877852522924708056, 0.8090169943749490056 ) ) ;
#41475 = LINE ( 'NONE', #11131, #45110 ) ;
#41476 = EDGE_CURVE ( 'NONE', #3678, #38915, #46928, .T. ) ;
#41477 = CYLINDRICAL_SURFACE ( 'NONE', #22827, 31.99999999999998579 ) ;
#41478 = DIRECTION ( 'NONE',  ( 0.000000000000000000, 0.000000000000000000, 1.000000000000000000 ) ) ;
#41479 = LINE ( 'NONE', #15052, #29387 ) ;
#41480 = CARTESIAN_POINT ( 'NONE',  ( 0.000000000000000000, 68.27212725128275395, 31.46837873495001503 ) ) ;
#41481 = DIRECTION ( 'NONE',  ( 1.000000000000000000, 0.000000000000000000, 0.000000000000000000 ) ) ;
#41482 = LINE ( 'NONE', #34128, #9846 ) ;
#41483 = ORIENTED_EDGE ( 'NONE', *, *, #23228, .T. ) ;
#41484 = DIRECTION ( 'NONE',  ( -1.000000000000000000, 0.000000000000000000, 0.000000000000000000 ) ) ;
#41485 = EDGE_LOOP ( 'NONE', ( #44278, #36791, #15075, #5697 ) ) ;
#41486 = ADVANCED_FACE ( 'NONE', ( #9961 ), #10441, .F. ) ;
#41487 = AXIS2_PLACEMENT_3D ( 'NONE', #26538, #15040, #6967 ) ;
#41488 = EDGE_CURVE ( 'NONE', #16291, #38706, #11058, .T. ) ;
#41489 = CIRCLE ( 'NONE', #47718, 31.99999999999998934 ) ;
#41490 = AXIS2_PLACEMENT_3D ( 'NONE', #8019, #30540, #7052 ) ;
#41491 = EDGE_CURVE ( 'NONE', #2023, #2304, #25360, .T. ) ;
#41492 = DIRECTION ( 'NONE',  ( 0.000000000000000000, -0.9781476007338067991, -0.2079116908177533196 ) ) ;
#41493 = VERTEX_POINT ( 'NONE', #36617 ) ;
#41494 = EDGE_CURVE ( 'NONE', #46638, #28147, #2850, .T. ) ;
#41495 = CIRCLE ( 'NONE', #845, 42.00000000000000000 ) ;
#41496 = VECTOR ( 'NONE', #27992, 1000.000000000000000 ) ;
#41497 = DIRECTION ( 'NONE',  ( 0.000000000000000000, 0.9135454576426005335, 0.4067366430758010409 ) ) ;
#41498 = AXIS2_PLACEMENT_3D ( 'NONE', #29588, #13940, #37175 ) ;
#41499 = DIRECTION ( 'NONE',  ( -0.000000000000000000, -0.000000000000000000, -1.000000000000000000 ) ) ;
#41500 = DIRECTION ( 'NONE',  ( -1.000000000000000000, 0.000000000000000000, 0.000000000000000000 ) ) ;
#41501 = ORIENTED_EDGE ( 'NONE', *, *, #4695, .F. ) ;
#41502 = DIRECTION ( 'NONE',  ( 1.000000000000000000, 0.000000000000000000, 0.000000000000000000 ) ) ;
#41503 = EDGE_CURVE ( 'NONE', #22671, #30256, #38415, .T. ) ;
#41504 = ORIENTED_EDGE ( 'NONE', *, *, #35590, .T. ) ;
#41505 = ORIENTED_EDGE ( 'NONE', *, *, #46739, .F. ) ;
#41506 = EDGE_CURVE ( 'NONE', #3764, #44761, #17295, .T. ) ;
#41507 = EDGE_CURVE ( 'NONE', #1214, #6623, #7142, .T. ) ;
#41508 = DIRECTION ( 'NONE',  ( 0.000000000000000000, 0.000000000000000000, 1.000000000000000000 ) ) ;
#41509 = DIRECTION ( 'NONE',  ( 0.000000000000000000, 0.000000000000000000, 1.000000000000000000 ) ) ;
#41510 = PLANE ( 'NONE',  #22829 ) ;
#41511 = VERTEX_POINT ( 'NONE', #43253 ) ;
#41512 = VERTEX_POINT ( 'NONE', #17777 ) ;
#41513 = ORIENTED_EDGE ( 'NONE', *, *, #20381, .T. ) ;
#41514 = EDGE_LOOP ( 'NONE', ( #4131, #17323, #43180, #35309 ) ) ;
#41515 = DIRECTION ( 'NONE',  ( 0.000000000000000000, 0.000000000000000000, 1.000000000000000000 ) ) ;
#41516 = ORIENTED_EDGE ( 'NONE', *, *, #23951, .F. ) ;
#41517 = PLANE ( 'NONE',  #7438 ) ;
#41518 = DIRECTION ( 'NONE',  ( 0.000000000000000000, 0.000000000000000000, 1.000000000000000000 ) ) ;
#41519 = PLANE ( 'NONE',  #25258 ) ;
#41520 = CARTESIAN_POINT ( 'NONE',  ( 11.99999999999999822, 0.000000000000000000, 0.000000000000000000 ) ) ;
#41521 = CARTESIAN_POINT ( 'NONE',  ( 4.999999999999999112, -40.68715046381921496, -10.41901085202121280 ) ) ;
#41522 = LINE ( 'NONE', #4076, #27621 ) ;
#41523 = DIRECTION ( 'NONE',  ( -1.000000000000000000, 0.000000000000000000, -0.000000000000000000 ) ) ;
#41524 = CARTESIAN_POINT ( 'NONE',  ( -15.44521549751111422, -137.7748507232956001, -5.500000000000000000 ) ) ;
#41526 = EDGE_CURVE ( 'NONE', #46150, #23361, #15734, .T. ) ;
#41525 = DIRECTION ( 'NONE',  ( 0.000000000000000000, 0.000000000000000000, 1.000000000000000000 ) ) ;
#41527 = ORIENTED_EDGE ( 'NONE', *, *, #19379, .F. ) ;
#41528 = DIRECTION ( 'NONE',  ( 0.000000000000000000, -0.3090169943749350168, -0.9510565162951576390 ) ) ;
#41529 = ORIENTED_EDGE ( 'NONE', *, *, #243, .T. ) ;
#41530 = EDGE_LOOP ( 'NONE', ( #8863, #34815, #21802, #11773 ) ) ;
#41531 = AXIS2_PLACEMENT_3D ( 'NONE', #36563, #25061, #13829 ) ;
#41532 = DIRECTION ( 'NONE',  ( 0.000000000000000000, 0.8910065241883657894, 0.4539904997395510788 ) ) ;
#41533 = VECTOR ( 'NONE', #40133, 1000.000000000000227 ) ;
#41534 = VECTOR ( 'NONE', #2597, 1000.000000000000114 ) ;
#41535 = DIRECTION ( 'NONE',  ( -1.000000000000000000, -0.000000000000000000, -0.000000000000000000 ) ) ;
#41536 = CARTESIAN_POINT ( 'NONE',  ( 2.500000000000000000, 16.00000000000000000, 0.000000000000000000 ) ) ;
#41537 = CARTESIAN_POINT ( 'NONE',  ( 26.09152095774781799, -124.8716048804687375, -5.500000000000000000 ) ) ;
#41538 = AXIS2_PLACEMENT_3D ( 'NONE', #43084, #14181, #9533 ) ;
#41539 = DIRECTION ( 'NONE',  ( -1.000000000000000000, -0.000000000000000000, 0.000000000000000000 ) ) ;
#41540 = DIRECTION ( 'NONE',  ( 0.000000000000000000, 0.000000000000000000, 1.000000000000000000 ) ) ;
#41541 = ORIENTED_EDGE ( 'NONE', *, *, #21784, .T. ) ;
#41542 = CYLINDRICAL_SURFACE ( 'NONE', #28666, 31.99999999999998579 ) ;
#41543 = LINE ( 'NONE', #19006, #18577 ) ;
#41544 = DIRECTION ( 'NONE',  ( -0.9730327541852497042, 0.2306669878475623159, 0.000000000000000000 ) ) ;
#41545 = VERTEX_POINT ( 'NONE', #36139 ) ;
#41546 = PRESENTATION_LAYER_ASSIGNMENT (  '', '', ( #14180 ) ) ;
#41547 = ORIENTED_EDGE ( 'NONE', *, *, #21675, .T. ) ;
#41548 = EDGE_CURVE ( 'NONE', #10384, #15864, #30585, .T. ) ;
#41549 = EDGE_CURVE ( 'NONE', #32278, #33790, #39338, .T. ) ;
#41550 = ORIENTED_EDGE ( 'NONE', *, *, #12719, .F. ) ;
#41551 = FACE_OUTER_BOUND ( 'NONE', #10461, .T. ) ;
#41552 = DIRECTION ( 'NONE',  ( 0.000000000000000000, 0.000000000000000000, 1.000000000000000000 ) ) ;
#41553 = ORIENTED_EDGE ( 'NONE', *, *, #11780, .T. ) ;
#41554 = ADVANCED_FACE ( 'NONE', ( #5820 ), #39600, .T. ) ;
#41555 = AXIS2_PLACEMENT_3D ( 'NONE', #32504, #10217, #13010 ) ;
#41556 = AXIS2_PLACEMENT_3D ( 'NONE', #40721, #17232, #6717 ) ;
#41557 = FACE_OUTER_BOUND ( 'NONE', #2898, .T. ) ;
#41558 = CIRCLE ( 'NONE', #40031, 31.99999999999998579 ) ;
#41559 = VERTEX_POINT ( 'NONE', #13881 ) ;
#41560 = VERTEX_POINT ( 'NONE', #6064 ) ;
#41561 = VECTOR ( 'NONE', #12872, 999.9999999999998863 ) ;
#41562 = VECTOR ( 'NONE', #41712, 1000.000000000000000 ) ;
#41563 = VECTOR ( 'NONE', #24417, 1000.000000000000000 ) ;
#41564 = EDGE_CURVE ( 'NONE', #6127, #23361, #31409, .T. ) ;
#41565 = EDGE_CURVE ( 'NONE', #43990, #8879, #47163, .T. ) ;
#41566 = CARTESIAN_POINT ( 'NONE',  ( 10.00000000000000000, 0.000000000000000000, 0.000000000000000000 ) ) ;
#41568 = ORIENTED_EDGE ( 'NONE', *, *, #6156, .F. ) ;
#41567 = DIRECTION ( 'NONE',  ( 0.000000000000000000, 0.1564344650402244852, 0.9876883405951387696 ) ) ;
#41569 = CARTESIAN_POINT ( 'NONE',  ( 11.99999999999999822, 15.33399622253482342, 80.55351364060595643 ) ) ;
#41570 = ORIENTED_EDGE ( 'NONE', *, *, #32854, .F. ) ;
#41571 = PLANE ( 'NONE',  #33308 ) ;
#41572 = ADVANCED_FACE ( 'NONE', ( #33439, #15081 ), #132, .F. ) ;
#41573 = ORIENTED_EDGE ( 'NONE', *, *, #30182, .F. ) ;
#41574 = VERTEX_POINT ( 'NONE', #10695 ) ;
#41575 = DIRECTION ( 'NONE',  ( 1.000000000000000000, 0.000000000000000000, 0.000000000000000000 ) ) ;
#41576 = VECTOR ( 'NONE', #34264, 1000.000000000000000 ) ;
#41577 = DIRECTION ( 'NONE',  ( -0.000000000000000000, 0.5000000000000031086, -0.8660254037844369313 ) ) ;
#41578 = CARTESIAN_POINT ( 'NONE',  ( 10.00000000000000000, 54.21277698773675979, 55.38113227695801299 ) ) ;
#41579 = VERTEX_POINT ( 'NONE', #40781 ) ;
#41580 = ORIENTED_EDGE ( 'NONE', *, *, #31711, .F. ) ;
#41581 = ADVANCED_FACE ( 'NONE', ( #7002 ), #44942, .T. ) ;
#41582 = LINE ( 'NONE', #42070, #39971 ) ;
#41583 = ORIENTED_EDGE ( 'NONE', *, *, #11746, .F. ) ;
#41584 = VERTEX_POINT ( 'NONE', #11647 ) ;
#41585 = CYLINDRICAL_SURFACE ( 'NONE', #24421, 31.99999999999999289 ) ;
#41586 = ORIENTED_EDGE ( 'NONE', *, *, #44100, .T. ) ;
#41587 = DIRECTION ( 'NONE',  ( -1.000000000000000000, -0.000000000000000000, -0.000000000000000000 ) ) ;
#41588 = DIRECTION ( 'NONE',  ( 0.000000000000000000, 0.3826834323650905589, -0.9238795325112864054 ) ) ;
#41589 = CARTESIAN_POINT ( 'NONE',  ( 11.99999999999999822, -8.840884882375609877, 74.65374052328647281 ) ) ;
#41590 = DIRECTION ( 'NONE',  ( 1.000000000000000000, 0.000000000000000000, -0.000000000000000000 ) ) ;
#41591 = DIRECTION ( 'NONE',  ( 0.000000000000000000, 0.000000000000000000, -1.000000000000000000 ) ) ;
#41592 = DIRECTION ( 'NONE',  ( -1.000000000000000000, 0.000000000000000000, 0.000000000000000000 ) ) ;
#41594 = CIRCLE ( 'NONE', #32985, 77.49900000000000944 ) ;
#41593 = CARTESIAN_POINT ( 'NONE',  ( 10.00000000000000000, -46.53671651293907274, -59.03961581697448935 ) ) ;
#41595 = CARTESIAN_POINT ( 'NONE',  ( 10.00000000000000000, 0.000000000000000000, 0.000000000000000000 ) ) ;
#41596 = DIRECTION ( 'NONE',  ( -1.000000000000000000, 0.000000000000000000, 0.000000000000000000 ) ) ;
#41597 = AXIS2_PLACEMENT_3D ( 'NONE', #3142, #10507, #29094 ) ;
#41598 = DIRECTION ( 'NONE',  ( 0.000000000000000000, 0.000000000000000000, -1.000000000000000000 ) ) ;
#41599 = CARTESIAN_POINT ( 'NONE',  ( -12.50000000000000000, -132.5000000000000000, -40.00000000000000000 ) ) ;
#41600 = CARTESIAN_POINT ( 'NONE',  ( -26.53422223201112828, -120.6595836127786043, 5.500000000000000000 ) ) ;
#41601 = AXIS2_PLACEMENT_3D ( 'NONE', #32901, #43928, #3044 ) ;
#41602 = ORIENTED_EDGE ( 'NONE', *, *, #28932, .F. ) ;
#41603 = CARTESIAN_POINT ( 'NONE',  ( 11.99999999999999822, 46.54456581323805153, 59.03342792756280488 ) ) ;
#41604 = ADVANCED_FACE ( 'NONE', ( #33198 ), #48125, .T. ) ;
#41605 = DIRECTION ( 'NONE',  ( 0.000000000000000000, -0.5877852522924803536, 0.8090169943749422332 ) ) ;
#41606 = DIRECTION ( 'NONE',  ( 0.000000000000000000, 0.7071067811865437980, 0.7071067811865512365 ) ) ;
#41607 = EDGE_CURVE ( 'NONE', #30536, #923, #33666, .T. ) ;
#41608 = ORIENTED_EDGE ( 'NONE', *, *, #36679, .T. ) ;
#41609 = EDGE_CURVE ( 'NONE', #18326, #38804, #29807, .T. ) ;
#41610 = EDGE_CURVE ( 'NONE', #25536, #38965, #2481, .T. ) ;
#41611 = EDGE_CURVE ( 'NONE', #37953, #2290, #45184, .T. ) ;
#41612 = ADVANCED_FACE ( 'NONE', ( #10923 ), #41510, .F. ) ;
#41613 = DIRECTION ( 'NONE',  ( -1.000000000000000000, -0.000000000000000000, -0.000000000000000000 ) ) ;
#41614 = VERTEX_POINT ( 'NONE', #37833 ) ;
#41615 = ORIENTED_EDGE ( 'NONE', *, *, #23902, .F. ) ;
#41616 = VERTEX_POINT ( 'NONE', #29289 ) ;
#41617 = AXIS2_PLACEMENT_3D ( 'NONE', #18881, #3230, #26253 ) ;
#41618 = AXIS2_PLACEMENT_3D ( 'NONE', #29161, #14973, #44346 ) ;
#41619 = DIRECTION ( 'NONE',  ( -1.000000000000000000, -0.000000000000000000, -0.000000000000000000 ) ) ;
#41620 = EDGE_CURVE ( 'NONE', #33189, #43507, #18971, .T. ) ;
#41621 = ORIENTED_EDGE ( 'NONE', *, *, #45687, .F. ) ;
#41622 = FACE_BOUND ( 'NONE', #24519, .T. ) ;
#41623 = AXIS2_PLACEMENT_3D ( 'NONE', #45736, #5345, #20495 ) ;
#41624 = ORIENTED_EDGE ( 'NONE', *, *, #40653, .F. ) ;
#41625 = DIRECTION ( 'NONE',  ( 1.000000000000000000, -0.000000000000000000, -0.000000000000000000 ) ) ;
#41626 = DIRECTION ( 'NONE',  ( -1.000000000000000000, 0.000000000000000000, 0.000000000000000000 ) ) ;
#41627 = VERTEX_POINT ( 'NONE', #29528 ) ;
#41628 = CARTESIAN_POINT ( 'NONE',  ( 10.00000000000000000, 12.26510123303308752, -35.53030884539072787 ) ) ;
#41629 = VERTEX_POINT ( 'NONE', #7245 ) ;
#41630 = PLANE ( 'NONE',  #22696 ) ;
#41631 = ADVANCED_FACE ( 'NONE', ( #22897 ), #14843, .T. ) ;
#41632 = CARTESIAN_POINT ( 'NONE',  ( 10.00000000000000000, 37.22597642581150268, 5.202137450157037435 ) ) ;
#41633 = ORIENTED_EDGE ( 'NONE', *, *, #16357, .F. ) ;
#41634 = VECTOR ( 'NONE', #42974, 1000.000000000000000 ) ;
#41635 = CARTESIAN_POINT ( 'NONE',  ( 0.000000000000000000, -70.53064760720336324, 26.01480285779810231 ) ) ;
#41636 = VERTEX_POINT ( 'NONE', #47870 ) ;
#41637 = ORIENTED_EDGE ( 'NONE', *, *, #24195, .F. ) ;
#41638 = DIRECTION ( 'NONE',  ( 0.000000000000000000, 0.3090169943749411230, 0.9510565162951555296 ) ) ;
#41639 = DIRECTION ( 'NONE',  ( 0.000000000000000000, 0.000000000000000000, 1.000000000000000000 ) ) ;
#41640 = ORIENTED_EDGE ( 'NONE', *, *, #5478, .T. ) ;
#41641 = CIRCLE ( 'NONE', #25977, 42.00000000000000000 ) ;
#41642 = DIRECTION ( 'NONE',  ( -1.000000000000000000, 0.000000000000000000, 0.000000000000000000 ) ) ;
#41643 = PLANE ( 'NONE',  #46184 ) ;
#41644 = CARTESIAN_POINT ( 'NONE',  ( 15.00000000000000000, 23.59884966291521380, -12.14883922797262805 ) ) ;
#41645 = DIRECTION ( 'NONE',  ( -1.000000000000000000, 0.000000000000000000, 0.000000000000000000 ) ) ;
#41646 = FACE_OUTER_BOUND ( 'NONE', #26554, .T. ) ;
#41647 = CARTESIAN_POINT ( 'NONE',  ( 10.00000000000000000, 62.50884508063427347, 41.76106447765511831 ) ) ;
#41648 = EDGE_CURVE ( 'NONE', #9073, #44497, #26715, .T. ) ;
#41649 = DIRECTION ( 'NONE',  ( 1.000000000000000000, 0.000000000000000000, -0.000000000000000000 ) ) ;
#41650 = DIRECTION ( 'NONE',  ( -1.000000000000000000, -0.000000000000000000, 0.000000000000000000 ) ) ;
#41651 = CARTESIAN_POINT ( 'NONE',  ( 0.000000000000000000, 40.68715046381943523, -10.41901085202036370 ) ) ;
#41652 = VECTOR ( 'NONE', #9306, 1000.000000000000114 ) ;
#41653 = ORIENTED_EDGE ( 'NONE', *, *, #41127, .T. ) ;
#41654 = CARTESIAN_POINT ( 'NONE',  ( 0.000000000000000000, -8.830959090341869100, -74.65491531819127147 ) ) ;
#41655 = DIRECTION ( 'NONE',  ( 0.000000000000000000, 1.000000000000000000, 0.000000000000000000 ) ) ;
#41656 = DIRECTION ( 'NONE',  ( 0.000000000000000000, 0.000000000000000000, 1.000000000000000000 ) ) ;
#41657 = LINE ( 'NONE', #1275, #9262 ) ;
#41658 = EDGE_CURVE ( 'NONE', #15777, #2920, #138, .T. ) ;
#41659 = ORIENTED_EDGE ( 'NONE', *, *, #35882, .T. ) ;
#41660 = ADVANCED_FACE ( 'NONE', ( #40542, #36856, #44688, #3324, #11168, #18256, #26093, #41042, #37351, #13278, #24776, #9121, #35060, #5221, #31412, #32127, #16235 ), #42411, .T. ) ;
#41661 = CIRCLE ( 'NONE', #47899, 15.99999999999999822 ) ;
#41662 = DIRECTION ( 'NONE',  ( -1.000000000000000000, 0.000000000000000000, 0.000000000000000000 ) ) ;
#41663 = VERTEX_POINT ( 'NONE', #17170 ) ;
#41664 = EDGE_CURVE ( 'NONE', #16116, #2031, #7936, .T. ) ;
#41665 = CARTESIAN_POINT ( 'NONE',  ( 10.00000000000000000, 0.000000000000000000, 0.000000000000000000 ) ) ;
#41666 = VECTOR ( 'NONE', #19759, 999.9999999999998863 ) ;
#41667 = APPLICATION_PROTOCOL_DEFINITION ( 'draft international standard', 'automotive_design', 1998, #30723 ) ;
#41668 = AXIS2_PLACEMENT_3D ( 'NONE', #45735, #41577, #30081 ) ;
#41669 = ADVANCED_FACE ( 'NONE', ( #28198 ), #39717, .F. ) ;
#41670 = DIRECTION ( 'NONE',  ( 0.000000000000000000, 0.8526401643540897357, 0.5224985647159531288 ) ) ;
#41671 = CIRCLE ( 'NONE', #15077, 37.49900000000000944 ) ;
#41672 = ORIENTED_EDGE ( 'NONE', *, *, #1505, .T. ) ;
#41673 = EDGE_CURVE ( 'NONE', #34735, #19426, #27977, .T. ) ;
#41674 = AXIS2_PLACEMENT_3D ( 'NONE', #32663, #7200, #47587 ) ;
#41675 = ADVANCED_FACE ( 'NONE', ( #24284 ), #38988, .T. ) ;
#41676 = VECTOR ( 'NONE', #1079, 1000.000000000000000 ) ;
#41677 = DIRECTION ( 'NONE',  ( -1.000000000000000000, 0.000000000000000000, 0.000000000000000000 ) ) ;
#41678 = ORIENTED_EDGE ( 'NONE', *, *, #8373, .F. ) ;
#41679 = LINE ( 'NONE', #38012, #2632 ) ;
#41680 = CARTESIAN_POINT ( 'NONE',  ( 10.00000000000000000, 27.75498641678786527, -31.52238457039571173 ) ) ;
#41682 = ORIENTED_EDGE ( 'NONE', *, *, #47891, .T. ) ;
#41681 = CARTESIAN_POINT ( 'NONE',  ( 0.000000000000000000, -22.32062822937489344, 14.36278369418800160 ) ) ;
#41683 = VERTEX_POINT ( 'NONE', #5946 ) ;
#41684 = VECTOR ( 'NONE', #5923, 1000.000000000000000 ) ;
#41685 = DIRECTION ( 'NONE',  ( 1.000000000000000000, 0.000000000000000000, 0.000000000000000000 ) ) ;
#41686 = CARTESIAN_POINT ( 'NONE',  ( 0.000000000000000000, 25.88420570971400991, 27.13269053701105449 ) ) ;
#41687 = DIRECTION ( 'NONE',  ( 0.000000000000000000, -0.9945218953682742891, -0.1045284632676449360 ) ) ;
#41688 = CIRCLE ( 'NONE', #26067, 37.49900000000000233 ) ;
#41689 = DIRECTION ( 'NONE',  ( -1.000000000000000000, 0.000000000000000000, 0.000000000000000000 ) ) ;
#41690 = ORIENTED_EDGE ( 'NONE', *, *, #24211, .T. ) ;
#41691 = CARTESIAN_POINT ( 'NONE',  ( 11.41210121379328335, -99.40233154247455616, 5.500000000000000000 ) ) ;
#41692 = ORIENTED_EDGE ( 'NONE', *, *, #42095, .F. ) ;
#41693 = ORIENTED_EDGE ( 'NONE', *, *, #17706, .F. ) ;
#41694 = AXIS2_PLACEMENT_3D ( 'NONE', #2154, #39613, #32021 ) ;
#41695 = DIRECTION ( 'NONE',  ( 0.000000000000000000, 0.000000000000000000, 1.000000000000000000 ) ) ;
#41696 = AXIS2_PLACEMENT_3D ( 'NONE', #22311, #16128, #42298 ) ;
#41697 = AXIS2_PLACEMENT_3D ( 'NONE', #4937, #31391, #34792 ) ;
#41698 = CARTESIAN_POINT ( 'NONE',  ( -11.99999999999999645, 0.000000000000000000, 12.85999999999999943 ) ) ;
#41699 = CIRCLE ( 'NONE', #1020, 31.99999999999998579 ) ;
#41700 = DIRECTION ( 'NONE',  ( 0.7273375899149802093, -0.6862798483830544471, 0.000000000000000000 ) ) ;
#41701 = DIRECTION ( 'NONE',  ( -1.000000000000000000, 0.000000000000000000, 0.000000000000000000 ) ) ;
#41702 = ORIENTED_EDGE ( 'NONE', *, *, #23260, .F. ) ;
#41703 = DIRECTION ( 'NONE',  ( 0.000000000000000000, 0.1564344650402244852, 0.9876883405951387696 ) ) ;
#41704 = CARTESIAN_POINT ( 'NONE',  ( 0.000000000000000000, 2.663952781846149254, 41.91543099594818500 ) ) ;
#41705 = CARTESIAN_POINT ( 'NONE',  ( 0.000000000000000000, -46.53671651293991118, 59.03961581697383565 ) ) ;
#41706 = DIRECTION ( 'NONE',  ( -1.000000000000000000, -0.000000000000000000, 0.000000000000000000 ) ) ;
#41707 = DIRECTION ( 'NONE',  ( 0.000000000000000000, 0.000000000000000000, -1.000000000000000000 ) ) ;
#41708 = EDGE_CURVE ( 'NONE', #25783, #31111, #35552, .T. ) ;
#41709 = AXIS2_PLACEMENT_3D ( 'NONE', #27233, #30421, #46074 ) ;
#41710 = VECTOR ( 'NONE', #15768, 999.9999999999998863 ) ;
#41711 = LINE ( 'NONE', #42433, #30134 ) ;
#41712 = DIRECTION ( 'NONE',  ( -1.000000000000000000, 0.000000000000000000, -0.000000000000000000 ) ) ;
#41713 = CARTESIAN_POINT ( 'NONE',  ( 10.00000000000000000, 0.000000000000000000, 0.000000000000000000 ) ) ;
#41714 = VECTOR ( 'NONE', #46534, 1000.000000000000000 ) ;
#41715 = CIRCLE ( 'NONE', #33875, 16.00000000000000000 ) ;
#41716 = DIRECTION ( 'NONE',  ( -1.000000000000000000, -0.000000000000000000, -0.000000000000000000 ) ) ;
#41717 = CARTESIAN_POINT ( 'NONE',  ( 10.00000000000000000, 12.26510123303308752, -35.53030884539072787 ) ) ;
#41718 = AXIS2_PLACEMENT_3D ( 'NONE', #16280, #46133, #12850 ) ;
#41719 = CARTESIAN_POINT ( 'NONE',  ( 21.85433023846371370, -135.0628101570779620, -5.500000000000000000 ) ) ;
#41720 = CYLINDRICAL_SURFACE ( 'NONE', #42781, 31.99999999999998579 ) ;
#41721 = LINE ( 'NONE', #41249, #14381 ) ;
#41722 = DIRECTION ( 'NONE',  ( -1.000000000000000000, -0.000000000000000000, -0.000000000000000000 ) ) ;
#41723 = EDGE_LOOP ( 'NONE', ( #11165, #30927, #39701, #40302 ) ) ;
#41724 = ADVANCED_FACE ( 'NONE', ( #31902 ), #43137, .T. ) ;
#41725 = EDGE_CURVE ( 'NONE', #28319, #41768, #27521, .T. ) ;
#41726 = LINE ( 'NONE', #38060, #16660 ) ;
#41727 = VERTEX_POINT ( 'NONE', #1303 ) ;
#41728 = AXIS2_PLACEMENT_3D ( 'NONE', #39019, #27285, #39254 ) ;
#41729 = EDGE_CURVE ( 'NONE', #3853, #38187, #15011, .T. ) ;
#41730 = CIRCLE ( 'NONE', #28445, 16.00000000000000000 ) ;
#41731 = ORIENTED_EDGE ( 'NONE', *, *, #8069, .T. ) ;
#41732 = ADVANCED_FACE ( 'NONE', ( #46086 ), #20360, .F. ) ;
#41733 = VERTEX_POINT ( 'NONE', #46576 ) ;
#41734 = AXIS2_PLACEMENT_3D ( 'NONE', #29957, #14795, #7199 ) ;
#41735 = AXIS2_PLACEMENT_3D ( 'NONE', #32457, #9438, #39308 ) ;
#41737 = EDGE_CURVE ( 'NONE', #44507, #14647, #7965, .T. ) ;
#41736 = ORIENTED_EDGE ( 'NONE', *, *, #29018, .T. ) ;
#41738 = DIRECTION ( 'NONE',  ( -1.000000000000000000, 0.000000000000000000, 0.000000000000000000 ) ) ;
#41739 = ORIENTED_EDGE ( 'NONE', *, *, #47671, .F. ) ;
#41740 = VECTOR ( 'NONE', #40896, 1000.000000000000000 ) ;
#41741 = AXIS2_PLACEMENT_3D ( 'NONE', #35580, #39747, #6442 ) ;
#41742 = CARTESIAN_POINT ( 'NONE',  ( -8.826826895187510402, -94.96827758698185562, 5.500000000000000000 ) ) ;
#41743 = AXIS2_PLACEMENT_3D ( 'NONE', #48434, #30096, #45023 ) ;
#41744 = DIRECTION ( 'NONE',  ( -1.000000000000000000, 0.000000000000000000, -0.000000000000000000 ) ) ;
#41745 = AXIS2_PLACEMENT_3D ( 'NONE', #46070, #12538, #27473 ) ;
#41747 = DIRECTION ( 'NONE',  ( 0.000000000000000000, 0.000000000000000000, 1.000000000000000000 ) ) ;
#41746 = CIRCLE ( 'NONE', #20641, 16.00000000000000000 ) ;
#41748 = ORIENTED_EDGE ( 'NONE', *, *, #3075, .T. ) ;
#41749 = DIRECTION ( 'NONE',  ( -1.000000000000000000, 0.000000000000000000, 0.000000000000000000 ) ) ;
#41750 = VERTEX_POINT ( 'NONE', #16708 ) ;
#41751 = ORIENTED_EDGE ( 'NONE', *, *, #22758, .F. ) ;
#41752 = CARTESIAN_POINT ( 'NONE',  ( 10.00000000000000000, -58.39081064771787766, 50.95692526931307498 ) ) ;
#41753 = DIRECTION ( 'NONE',  ( 0.000000000000000000, 0.000000000000000000, 1.000000000000000000 ) ) ;
#41754 = ORIENTED_EDGE ( 'NONE', *, *, #43988, .F. ) ;
#41755 = EDGE_LOOP ( 'NONE', ( #11921, #12932, #41253, #12790 ) ) ;
#41756 = ORIENTED_EDGE ( 'NONE', *, *, #17521, .T. ) ;
#41757 = LINE ( 'NONE', #858, #24760 ) ;
#41758 = ORIENTED_EDGE ( 'NONE', *, *, #10111, .F. ) ;
#41759 = DIRECTION ( 'NONE',  ( -0.000000000000000000, 0.1045284632676570929, -0.9945218953682730678 ) ) ;
#41760 = DIRECTION ( 'NONE',  ( -1.000000000000000000, 0.000000000000000000, 0.000000000000000000 ) ) ;
#41761 = LINE ( 'NONE', #27080, #33097 ) ;
#41762 = DIRECTION ( 'NONE',  ( 0.000000000000000000, 0.000000000000000000, -1.000000000000000000 ) ) ;
#41763 = DIRECTION ( 'NONE',  ( 0.000000000000000000, -0.5877852522924624790, -0.8090169943749550008 ) ) ;
#41764 = LINE ( 'NONE', #44703, #35438 ) ;
#41765 = CARTESIAN_POINT ( 'NONE',  ( 10.00000000000000000, 46.21855187248629449, 62.20884554314036308 ) ) ;
#41766 = FACE_OUTER_BOUND ( 'NONE', #15208, .T. ) ;
#41767 = CARTESIAN_POINT ( 'NONE',  ( 15.00000000000000000, 16.61724383029390140, 20.69703378468902955 ) ) ;
#41768 = VERTEX_POINT ( 'NONE', #38754 ) ;
#41769 = CARTESIAN_POINT ( 'NONE',  ( 19.12409105625795291, -101.5943176906707919, 5.500000000000000000 ) ) ;
#41770 = AXIS2_PLACEMENT_3D ( 'NONE', #13948, #2676, #6850 ) ;
#41771 = CARTESIAN_POINT ( 'NONE',  ( 11.99999999999999822, 0.000000000000000000, 0.000000000000000000 ) ) ;
#41772 = ADVANCED_FACE ( 'NONE', ( #31658 ), #20132, .T. ) ;
#41773 = VERTEX_POINT ( 'NONE', #42663 ) ;
#41774 = ORIENTED_EDGE ( 'NONE', *, *, #38605, .T. ) ;
#41775 = FACE_OUTER_BOUND ( 'NONE', #17531, .T. ) ;
#41776 = CIRCLE ( 'NONE', #44139, 82.00000000000000000 ) ;
#41777 = EDGE_CURVE ( 'NONE', #44508, #11246, #46281, .T. ) ;
#41778 = CARTESIAN_POINT ( 'NONE',  ( 11.99999999999999822, 0.000000000000000000, 0.000000000000000000 ) ) ;
#41779 = VECTOR ( 'NONE', #12797, 1000.000000000000000 ) ;
#41780 = CARTESIAN_POINT ( 'NONE',  ( 5.000000000000002665, -21.60688246758530440, -79.10210256391390260 ) ) ;
#41781 = CARTESIAN_POINT ( 'NONE',  ( 32.50000000000000000, -120.0000000000000000, -2.500000000000000000 ) ) ;
#41782 = EDGE_CURVE ( 'NONE', #4110, #15076, #44569, .T. ) ;
#41783 = CYLINDRICAL_SURFACE ( 'NONE', #47418, 37.49900000000000233 ) ;
#41784 = DIRECTION ( 'NONE',  ( -1.000000000000000000, 0.000000000000000000, -0.000000000000000000 ) ) ;
#41785 = ORIENTED_EDGE ( 'NONE', *, *, #39174, .F. ) ;
#41786 = AXIS2_PLACEMENT_3D ( 'NONE', #20475, #13146, #9702 ) ;
#41787 = CIRCLE ( 'NONE', #12849, 31.99999999999999289 ) ;
#41788 = CARTESIAN_POINT ( 'NONE',  ( 10.00000000000000000, -58.39081064771713869, -50.95692526931392052 ) ) ;
#41789 = CARTESIAN_POINT ( 'NONE',  ( 10.00000000000000000, 71.27951684758026829, 30.41916302227139113 ) ) ;
#41790 = AXIS2_PLACEMENT_3D ( 'NONE', #24907, #39623, #20996 ) ;
#41791 = VERTEX_POINT ( 'NONE', #47741 ) ;
#41792 = EDGE_CURVE ( 'NONE', #14101, #16743, #44333, .T. ) ;
#41793 = FILL_AREA_STYLE_COLOUR ( '', #37453 ) ;
#41794 = LINE ( 'NONE', #12415, #4880 ) ;
#41795 = AXIS2_PLACEMENT_3D ( 'NONE', #42742, #38331, #24356 ) ;
#41796 = VERTEX_POINT ( 'NONE', #21328 ) ;
#41797 = EDGE_CURVE ( 'NONE', #29191, #44743, #22013, .T. ) ;
#41798 = ADVANCED_FACE ( 'NONE', ( #36260 ), #48246, .F. ) ;
#41799 = ORIENTED_EDGE ( 'NONE', *, *, #36664, .T. ) ;
#41800 = EDGE_LOOP ( 'NONE', ( #46742, #7434, #43563, #30367 ) ) ;
#41801 = ORIENTED_EDGE ( 'NONE', *, *, #24692, .T. ) ;
#41802 = VERTEX_POINT ( 'NONE', #32818 ) ;
#41803 = FACE_OUTER_BOUND ( 'NONE', #17666, .T. ) ;
#41804 = CYLINDRICAL_SURFACE ( 'NONE', #40986, 31.99999999999998579 ) ;
#41805 = ORIENTED_EDGE ( 'NONE', *, *, #12341, .F. ) ;
#41806 = AXIS2_PLACEMENT_3D ( 'NONE', #11001, #26421, #8041 ) ;
#41807 = DIRECTION ( 'NONE',  ( 0.000000000000000000, 0.000000000000000000, 1.000000000000000000 ) ) ;
#41808 = AXIS2_PLACEMENT_3D ( 'NONE', #39285, #31964, #28041 ) ;
#41809 = CIRCLE ( 'NONE', #14448, 16.00000000000000000 ) ;
#41810 = VERTEX_POINT ( 'NONE', #14481 ) ;
#41811 = ORIENTED_EDGE ( 'NONE', *, *, #13970, .F. ) ;
#41812 = CARTESIAN_POINT ( 'NONE',  ( 11.99999999999999822, 62.50884508063487033, -41.76106447765422303 ) ) ;
#41813 = CARTESIAN_POINT ( 'NONE',  ( 10.00000000000000000, 0.000000000000000000, 0.000000000000000000 ) ) ;
#41814 = CARTESIAN_POINT ( 'NONE',  ( 0.000000000000000000, -120.0000000000000000, 125.0000000000000000 ) ) ;
#41815 = VECTOR ( 'NONE', #66, 1000.000000000000000 ) ;
#41816 = ORIENTED_EDGE ( 'NONE', *, *, #42506, .T. ) ;
#41817 = DIRECTION ( 'NONE',  ( -1.000000000000000000, -0.000000000000000000, -0.000000000000000000 ) ) ;
#41818 = ORIENTED_EDGE ( 'NONE', *, *, #22104, .T. ) ;
#41819 = ORIENTED_EDGE ( 'NONE', *, *, #22803, .F. ) ;
#41820 = CIRCLE ( 'NONE', #8197, 16.00000000000000000 ) ;
#41821 = DIRECTION ( 'NONE',  ( 0.000000000000000000, 0.000000000000000000, 1.000000000000000000 ) ) ;
#41822 = CIRCLE ( 'NONE', #45036, 42.00000000000000000 ) ;
#41823 = DIRECTION ( 'NONE',  ( 1.000000000000000000, 0.000000000000000000, 0.000000000000000000 ) ) ;
#41824 = DIRECTION ( 'NONE',  ( -1.000000000000000000, -0.000000000000000000, 0.000000000000000000 ) ) ;
#41826 = EDGE_LOOP ( 'NONE', ( #2656, #12092, #20516, #25045 ) ) ;
#41825 = AXIS2_PLACEMENT_3D ( 'NONE', #35628, #25078, #28763 ) ;
#41827 = ORIENTED_EDGE ( 'NONE', *, *, #28651, .F. ) ;
#41828 = CARTESIAN_POINT ( 'NONE',  ( -4.250000000000000000, -13.95926121303099343, -1.199999999999999956 ) ) ;
#41829 = CARTESIAN_POINT ( 'NONE',  ( 11.99999999999999822, 77.32052557432849937, -5.256550761632002633 ) ) ;
#41830 = EDGE_CURVE ( 'NONE', #12875, #36756, #21083, .T. ) ;
#41831 = ORIENTED_EDGE ( 'NONE', *, *, #21139, .F. ) ;
#41832 = DIRECTION ( 'NONE',  ( 0.000000000000000000, 0.000000000000000000, 1.000000000000000000 ) ) ;
#41833 = VERTEX_POINT ( 'NONE', #28692 ) ;
#41834 = DIRECTION ( 'NONE',  ( -1.000000000000000000, -0.000000000000000000, -0.000000000000000000 ) ) ;
#41835 = EDGE_CURVE ( 'NONE', #7063, #40162, #21807, .T. ) ;
#41836 = CARTESIAN_POINT ( 'NONE',  ( 0.000000000000000000, -62.50329211542465657, 41.76937507738766442 ) ) ;
#41837 = DIRECTION ( 'NONE',  ( 0.000000000000000000, 0.000000000000000000, 1.000000000000000000 ) ) ;
#41838 = CARTESIAN_POINT ( 'NONE',  ( 10.00000000000000000, -23.16143007188481207, 73.95703589263968070 ) ) ;
#41839 = AXIS2_PLACEMENT_3D ( 'NONE', #34470, #42817, #8306 ) ;
#41840 = DIRECTION ( 'NONE',  ( 1.000000000000000000, 0.000000000000000000, 0.000000000000000000 ) ) ;
#41841 = DIRECTION ( 'NONE',  ( -1.000000000000000000, -0.000000000000000000, 0.000000000000000000 ) ) ;
#41842 = EDGE_CURVE ( 'NONE', #37702, #37765, #22045, .T. ) ;
#41843 = DIRECTION ( 'NONE',  ( -1.000000000000000000, -0.000000000000000000, -0.000000000000000000 ) ) ;
#41844 = CIRCLE ( 'NONE', #26213, 32.00000000000000000 ) ;
#41845 = CARTESIAN_POINT ( 'NONE',  ( 11.99999999999999822, 55.16347631943042984, 60.67117009219156643 ) ) ;
#41846 = DIRECTION ( 'NONE',  ( -1.000000000000000000, 0.000000000000000000, -0.000000000000000000 ) ) ;
#41847 = EDGE_LOOP ( 'NONE', ( #2468, #26526, #1662, #7418 ) ) ;
#41848 = CIRCLE ( 'NONE', #24618, 31.99999999999998934 ) ;
#41849 = DIRECTION ( 'NONE',  ( -1.000000000000000000, 0.000000000000000000, 0.000000000000000000 ) ) ;
#41850 = CARTESIAN_POINT ( 'NONE',  ( 10.00000000000000000, -14.67089635893764665, 73.72996012237435082 ) ) ;
#41851 =( LENGTH_UNIT ( ) NAMED_UNIT ( * ) SI_UNIT ( .MILLI., .METRE. ) );
#41852 = DIRECTION ( 'NONE',  ( -1.000000000000000000, -0.000000000000000000, -0.000000000000000000 ) ) ;
#41853 = EDGE_CURVE ( 'NONE', #45623, #11599, #11041, .T. ) ;
#41854 = ADVANCED_FACE ( 'NONE', ( #36732 ), #14230, .T. ) ;
#41855 = ORIENTED_EDGE ( 'NONE', *, *, #1863, .F. ) ;
#41856 = ORIENTED_EDGE ( 'NONE', *, *, #46752, .F. ) ;
#41857 = CIRCLE ( 'NONE', #33244, 82.00000000000000000 ) ;
#41858 = AXIS2_PLACEMENT_3D ( 'NONE', #32880, #13823, #47805 ) ;
#41859 = UNCERTAINTY_MEASURE_WITH_UNIT (LENGTH_MEASURE( 1.000000000000000082E-05 ), #22933, 'distance_accuracy_value', 'NONE');
#41860 = CARTESIAN_POINT ( 'NONE',  ( -3.000000000000000000, 9.615535125378775305, 24.73947219025917121 ) ) ;
#41861 = VECTOR ( 'NONE', #30507, 1000.000000000000000 ) ;
#41862 = LINE ( 'NONE', #27168, #35458 ) ;
#41863 = FACE_OUTER_BOUND ( 'NONE', #37522, .T. ) ;
#41864 = AXIS2_PLACEMENT_3D ( 'NONE', #19456, #12157, #860 ) ;
#41865 = EDGE_LOOP ( 'NONE', ( #7585, #24674, #47492, #44862 ) ) ;
#41866 = AXIS2_PLACEMENT_3D ( 'NONE', #1974, #13456, #46759 ) ;
#41867 = EDGE_CURVE ( 'NONE', #45054, #5880, #8733, .T. ) ;
#41868 = CARTESIAN_POINT ( 'NONE',  ( 0.000000000000000000, -41.76937507738831812, 62.50329211542423025 ) ) ;
#41869 = EDGE_LOOP ( 'NONE', ( #39653, #15451, #29763, #19628 ) ) ;
#41870 = EDGE_LOOP ( 'NONE', ( #34236, #11631, #33659, #2493 ) ) ;
#41871 = ORIENTED_EDGE ( 'NONE', *, *, #43543, .F. ) ;
#41872 = AXIS2_PLACEMENT_3D ( 'NONE', #5507, #1841, #46872 ) ;
#41873 = VERTEX_POINT ( 'NONE', #6654 ) ;
#41874 = AXIS2_PLACEMENT_3D ( 'NONE', #21351, #32618, #10598 ) ;
#41875 = DIRECTION ( 'NONE',  ( 0.000000000000000000, 0.9876883405951372152, 0.1564344650402346160 ) ) ;
#41876 = ORIENTED_EDGE ( 'NONE', *, *, #17819, .F. ) ;
#41877 = ORIENTED_EDGE ( 'NONE', *, *, #42715, .F. ) ;
#41878 = DIRECTION ( 'NONE',  ( 0.000000000000000000, 0.000000000000000000, 1.000000000000000000 ) ) ;
#41879 = ORIENTED_EDGE ( 'NONE', *, *, #15155, .T. ) ;
#41880 = LINE ( 'NONE', #8332, #28255 ) ;
#41881 = ORIENTED_EDGE ( 'NONE', *, *, #25012, .T. ) ;
#41882 = CARTESIAN_POINT ( 'NONE',  ( 10.00000000000000000, 0.000000000000000000, 0.000000000000000000 ) ) ;
#41883 = CARTESIAN_POINT ( 'NONE',  ( 11.99999999999999822, -11.30684508768284680, -76.66974797899850103 ) ) ;
#41884 = EDGE_LOOP ( 'NONE', ( #8676, #41081, #12398, #7649 ) ) ;
#41885 = CARTESIAN_POINT ( 'NONE',  ( 11.99999999999999822, -80.55351364060599906, 15.33399622253457295 ) ) ;
#41886 = VERTEX_POINT ( 'NONE', #2963 ) ;
#41887 = FACE_OUTER_BOUND ( 'NONE', #40585, .T. ) ;
#41888 = CARTESIAN_POINT ( 'NONE',  ( 0.000000000000000000, 71.21200624218852226, -40.65526001592539984 ) ) ;
#41889 = AXIS2_PLACEMENT_3D ( 'NONE', #29090, #9290, #24222 ) ;
#41890 = VERTEX_POINT ( 'NONE', #29411 ) ;
#41891 = CARTESIAN_POINT ( 'NONE',  ( 2.117611129180199558, -93.54218975225703048, 5.500000000000000000 ) ) ;
#41892 = ORIENTED_EDGE ( 'NONE', *, *, #3920, .F. ) ;
#41893 = ORIENTED_EDGE ( 'NONE', *, *, #14475, .T. ) ;
#41894 = DIRECTION ( 'NONE',  ( -1.000000000000000000, 0.000000000000000000, -0.000000000000000000 ) ) ;
#41895 = LINE ( 'NONE', #8103, #6741 ) ;
#41896 = ORIENTED_EDGE ( 'NONE', *, *, #26376, .F. ) ;
#41897 = EDGE_CURVE ( 'NONE', #36459, #7382, #32591, .T. ) ;
#41898 = CARTESIAN_POINT ( 'NONE',  ( 0.000000000000000000, 74.74816331893477184, -33.71516098798660011 ) ) ;
#41899 = AXIS2_PLACEMENT_3D ( 'NONE', #10156, #21410, #6490 ) ;
#41900 = CARTESIAN_POINT ( 'NONE',  ( -26.53422223201112828, -120.6595836127786043, 5.500000000000000000 ) ) ;
#41901 = LINE ( 'NONE', #42622, #15163 ) ;
#41902 = CIRCLE ( 'NONE', #1260, 12.49999999999999645 ) ;
#41903 = DIRECTION ( 'NONE',  ( 0.000000000000000000, 0.000000000000000000, 1.000000000000000000 ) ) ;
#41904 = ADVANCED_FACE ( 'NONE', ( #3197 ), #29639, .T. ) ;
#41905 = DIRECTION ( 'NONE',  ( 1.000000000000000000, 0.000000000000000000, 0.000000000000000000 ) ) ;
#41906 = DIRECTION ( 'NONE',  ( -1.000000000000000000, -0.000000000000000000, 0.000000000000000000 ) ) ;
#41907 = ORIENTED_EDGE ( 'NONE', *, *, #42437, .T. ) ;
#41908 = CLOSED_SHELL ( 'NONE', ( #31520, #27107, #25519, #36667, #32962, #47561, #47380, #33205, #38859, #41675, #42740, #24622, #43935, #24753, #16749, #3919, #2586, #46496, #6075, #25643, #6813, #1823 ) ) ;
#41909 = DIRECTION ( 'NONE',  ( 0.000000000000000000, -1.000000000000000000, 0.000000000000000000 ) ) ;
#41910 = ADVANCED_FACE ( 'NONE', ( #43845 ), #17892, .T. ) ;
#41911 = CARTESIAN_POINT ( 'NONE',  ( 15.00000000000000000, -10.45096189432344502, -21.10159698893425784 ) ) ;
#41912 = DIRECTION ( 'NONE',  ( 0.000000000000000000, 0.000000000000000000, -1.000000000000000000 ) ) ;
#41913 = ORIENTED_EDGE ( 'NONE', *, *, #26306, .T. ) ;
#41914 = CIRCLE ( 'NONE', #5960, 77.49899999999999523 ) ;
#41915 = DIRECTION ( 'NONE',  ( 1.000000000000000000, 0.000000000000000000, 0.000000000000000000 ) ) ;
#41916 = DIRECTION ( 'NONE',  ( -1.000000000000000000, 0.000000000000000000, -0.000000000000000000 ) ) ;
#41917 = LINE ( 'NONE', #27702, #11566 ) ;
#41918 = CIRCLE ( 'NONE', #33293, 82.00000000000000000 ) ;
#41919 = CARTESIAN_POINT ( 'NONE',  ( 10.00000000000000000, -30.84782396557201878, -21.32104025579148399 ) ) ;
#41920 = ORIENTED_EDGE ( 'NONE', *, *, #32542, .F. ) ;
#41921 = EDGE_CURVE ( 'NONE', #24099, #1474, #7170, .T. ) ;
#41922 = EDGE_LOOP ( 'NONE', ( #15021, #13335, #3417, #2132 ) ) ;
#41923 = CARTESIAN_POINT ( 'NONE',  ( 5.000000000000000000, 2.663952781846149254, 41.91543099594818500 ) ) ;
#41924 = ORIENTED_EDGE ( 'NONE', *, *, #29689, .F. ) ;
#41925 = EDGE_CURVE ( 'NONE', #17779, #45724, #36016, .T. ) ;
#41926 = DIRECTION ( 'NONE',  ( -1.000000000000000000, 0.000000000000000000, 0.000000000000000000 ) ) ;
#41927 = APPLICATION_PROTOCOL_DEFINITION ( 'draft international standard', 'automotive_design', 1998, #45743 ) ;
#41928 = DIRECTION ( 'NONE',  ( 0.000000000000000000, 0.3090169943749480619, -0.9510565162951533091 ) ) ;
#41929 = AXIS2_PLACEMENT_3D ( 'NONE', #42981, #9429, #6260 ) ;
#41930 = ORIENTED_EDGE ( 'NONE', *, *, #7394, .F. ) ;
#41931 = EDGE_CURVE ( 'NONE', #33596, #24133, #41558, .T. ) ;
#41932 = AXIS2_PLACEMENT_3D ( 'NONE', #38137, #46203, #35175 ) ;
#41933 = DIRECTION ( 'NONE',  ( -0.7585478161175716050, -0.6516173805718067369, 0.000000000000000000 ) ) ;
#41934 = AXIS2_PLACEMENT_3D ( 'NONE', #37254, #3718, #3965 ) ;
#41935 = VERTEX_POINT ( 'NONE', #34503 ) ;
#41936 = EDGE_CURVE ( 'NONE', #42659, #28062, #4664, .T. ) ;
#41937 = CARTESIAN_POINT ( 'NONE',  ( 15.00000000000000000, 0.000000000000000000, 0.000000000000000000 ) ) ;
#41938 = CYLINDRICAL_SURFACE ( 'NONE', #1587, 31.99999999999999289 ) ;
#41939 = DIRECTION ( 'NONE',  ( -1.000000000000000000, 0.000000000000000000, 0.000000000000000000 ) ) ;
#41940 = VERTEX_POINT ( 'NONE', #11536 ) ;
#41941 = VECTOR ( 'NONE', #46783, 1000.000000000000000 ) ;
#41942 = CARTESIAN_POINT ( 'NONE',  ( 10.00000000000000000, 46.54456581323805153, 59.03342792756280488 ) ) ;
#41943 = CARTESIAN_POINT ( 'NONE',  ( 0.000000000000000000, 0.000000000000000000, 0.000000000000000000 ) ) ;
#41944 = LINE ( 'NONE', #22113, #43130 ) ;
#41945 = VECTOR ( 'NONE', #48440, 1000.000000000000114 ) ;
#41947 = VERTEX_POINT ( 'NONE', #8090 ) ;
#41946 = CARTESIAN_POINT ( 'NONE',  ( 0.000000000000000000, 12.42422080174688404, -35.38097989696498047 ) ) ;
#41948 = ORIENTED_EDGE ( 'NONE', *, *, #40556, .T. ) ;
#41949 = CARTESIAN_POINT ( 'NONE',  ( 10.00000000000000000, -77.49459641780886443, -0.8261519478439277586 ) ) ;
#41950 = ORIENTED_EDGE ( 'NONE', *, *, #36423, .T. ) ;
#41951 = ORIENTED_EDGE ( 'NONE', *, *, #20906, .F. ) ;
#41952 = EDGE_CURVE ( 'NONE', #35782, #39822, #25156, .T. ) ;
#41953 = CARTESIAN_POINT ( 'NONE',  ( 10.00000000000000000, 6.555932627142418312, 37.01155633439060466 ) ) ;
#41954 = VERTEX_POINT ( 'NONE', #23269 ) ;
#41955 = EDGE_CURVE ( 'NONE', #41296, #37915, #37473, .T. ) ;
#41956 = DIRECTION ( 'NONE',  ( 0.000000000000000000, 0.000000000000000000, -1.000000000000000000 ) ) ;
#41957 = CARTESIAN_POINT ( 'NONE',  ( 11.99999999999999822, -10.30890764327323872, -81.34940948281347062 ) ) ;
#41958 = CARTESIAN_POINT ( 'NONE',  ( -3.961125083139900749, -143.2122702051246677, 2.500000000000000000 ) ) ;
#41959 = EDGE_LOOP ( 'NONE', ( #35248, #8331, #23790, #1774, #21702, #12376, #742, #1466, #36539, #35218, #13276, #8574, #465, #7492, #39467, #41254, #24111, #32955, #14110, #8550, #35344, #39520, #19354, #23282, #24880, #45843, #34302, #8163, #23184, #6956, #30657, #35551, #16887, #38620, #681, #8160, #35176, #36655, #28355, #28572, #46333, #23613, #43631, #18889, #38533, #4389, #26173, #17772, #21968, #12902, #18194, #37503, #17315, #34241, #26857, #21474, #3594, #9012, #40241, #1865, #13002, #8741, #10972, #6331, #26625, #35075, #43480, #40579, #5438, #21883, #30996, #46821, #9282, #30489, #14470, #19777, #16814, #14718, #40446, #22852, #44579, #32205, #17813, #9250, #26863, #16111, #33073, #5797, #30057, #5874, #22647, #36557, #31259, #11812, #47348, #19331, #21850, #48427, #22244, #25947, #17042, #16825, #23047, #8038, #32810, #28372, #18917, #38686, #32805, #3685, #12241, #43335, #25972, #34873, #48176, #47086, #21815, #18487, #23494, #885, #3229, #31526, #44285, #47196, #6435, #41363, #13007, #37212, #45629, #29581, #46583, #9712, #36717, #28867, #38171, #4378, #10170, #1426, #29473, #43621, #13316, #8628, #18600, #39593, #20086, #32030, #29017, #38136, #25188, #39144, #16820, #3317, #11648, #7712, #8919, #30719, #35550, #45509, #45407, #4883, #18800, #2856, #6505, #25036, #21527 ) ) ;
#41960 = CARTESIAN_POINT ( 'NONE',  ( 11.99999999999999822, 0.000000000000000000, 0.000000000000000000 ) ) ;
#41961 = FACE_OUTER_BOUND ( 'NONE', #5551, .T. ) ;
#41962 = EDGE_CURVE ( 'NONE', #25331, #6202, #20447, .T. ) ;
#41963 = LINE ( 'NONE', #9141, #35220 ) ;
#41964 = PLANE ( 'NONE',  #11940 ) ;
#41965 = CARTESIAN_POINT ( 'NONE',  ( 0.000000000000000000, 0.000000000000000000, 0.000000000000000000 ) ) ;
#41966 = AXIS2_PLACEMENT_3D ( 'NONE', #28038, #16529, #24836 ) ;
#41967 = LINE ( 'NONE', #12346, #44205 ) ;
#41969 = EDGE_CURVE ( 'NONE', #46575, #40440, #47793, .T. ) ;
#41968 = CARTESIAN_POINT ( 'NONE',  ( 10.00000000000000000, 34.44570377933598593, 69.42325613327452061 ) ) ;
#41970 = DIRECTION ( 'NONE',  ( 0.000000000000000000, -0.9510565162951565288, 0.3090169943749384029 ) ) ;
#41971 = CIRCLE ( 'NONE', #40390, 31.99999999999999289 ) ;
#41972 = FACE_OUTER_BOUND ( 'NONE', #22470, .T. ) ;
#41973 = FACE_OUTER_BOUND ( 'NONE', #37235, .T. ) ;
#41974 = ORIENTED_EDGE ( 'NONE', *, *, #24553, .T. ) ;
#41975 = ORIENTED_EDGE ( 'NONE', *, *, #38597, .T. ) ;
#41976 = PLANE ( 'NONE',  #29527 ) ;
#41977 = DIRECTION ( 'NONE',  ( -1.000000000000000000, 0.000000000000000000, 0.000000000000000000 ) ) ;
#41978 = ORIENTED_EDGE ( 'NONE', *, *, #25294, .F. ) ;
#41979 = ORIENTED_EDGE ( 'NONE', *, *, #20115, .T. ) ;
#41980 = VECTOR ( 'NONE', #7757, 1000.000000000000000 ) ;
#41981 = LINE ( 'NONE', #26556, #12750 ) ;
#41982 = ORIENTED_EDGE ( 'NONE', *, *, #1384, .F. ) ;
#41983 = VECTOR ( 'NONE', #32269, 1000.000000000000000 ) ;
#41984 = EDGE_CURVE ( 'NONE', #38924, #41064, #24365, .T. ) ;
#41985 = ORIENTED_EDGE ( 'NONE', *, *, #14130, .F. ) ;
#41986 = ORIENTED_EDGE ( 'NONE', *, *, #14321, .T. ) ;
#41987 = CARTESIAN_POINT ( 'NONE',  ( 0.000000000000000000, 33.17418723428333749, -17.67226234102790272 ) ) ;
#41988 = ORIENTED_EDGE ( 'NONE', *, *, #1441, .T. ) ;
#41989 = AXIS2_PLACEMENT_3D ( 'NONE', #26761, #42171, #22605 ) ;
#41990 = DIRECTION ( 'NONE',  ( 0.000000000000000000, 0.000000000000000000, -1.000000000000000000 ) ) ;
#41991 = DIRECTION ( 'NONE',  ( -1.000000000000000000, -0.000000000000000000, 0.000000000000000000 ) ) ;
#41992 = CARTESIAN_POINT ( 'NONE',  ( 11.99999999999999822, 46.53671651294032330, -59.03961581697353012 ) ) ;
#41993 = VERTEX_POINT ( 'NONE', #22544 ) ;
#41994 = VECTOR ( 'NONE', #27157, 1000.000000000000000 ) ;
#41995 = CARTESIAN_POINT ( 'NONE',  ( 10.00000000000000000, 33.79645857604513992, 16.45098606841138178 ) ) ;
#41996 = VERTEX_POINT ( 'NONE', #3942 ) ;
#41997 = ORIENTED_EDGE ( 'NONE', *, *, #4905, .F. ) ;
#41998 = CARTESIAN_POINT ( 'NONE',  ( 0.000000000000000000, 10.41901085202078292, 40.68715046381932865 ) ) ;
#41999 = DIRECTION ( 'NONE',  ( 0.000000000000000000, -0.5224985647159380298, -0.8526401643540988395 ) ) ;
#42000 = VERTEX_POINT ( 'NONE', #34267 ) ;
#42001 = VECTOR ( 'NONE', #25510, 1000.000000000000000 ) ;
#42002 = VERTEX_POINT ( 'NONE', #7848 ) ;
#42003 = FACE_OUTER_BOUND ( 'NONE', #42952, .T. ) ;
#42004 = VERTEX_POINT ( 'NONE', #23024 ) ;
#42005 = EDGE_CURVE ( 'NONE', #39757, #3577, #11897, .T. ) ;
#42006 = DIRECTION ( 'NONE',  ( 1.000000000000000000, 0.000000000000000000, 0.000000000000000000 ) ) ;
#42007 = DIRECTION ( 'NONE',  ( -1.000000000000000000, 0.000000000000000000, 0.000000000000000000 ) ) ;
#42008 = DIRECTION ( 'NONE',  ( -1.000000000000000000, 0.000000000000000000, -0.000000000000000000 ) ) ;
#42009 = CARTESIAN_POINT ( 'NONE',  ( -11.69999999999999929, 0.000000000000000000, 0.000000000000000000 ) ) ;
#42010 = LINE ( 'NONE', #23388, #12639 ) ;
#42011 = EDGE_CURVE ( 'NONE', #22253, #23219, #30141, .T. ) ;
#42012 = LINE ( 'NONE', #38328, #285 ) ;
#42013 = CARTESIAN_POINT ( 'NONE',  ( 10.00000000000000000, 0.000000000000000000, 0.000000000000000000 ) ) ;
#42014 = ORIENTED_EDGE ( 'NONE', *, *, #10678, .F. ) ;
#42015 = DIRECTION ( 'NONE',  ( -1.000000000000000000, 0.000000000000000000, -0.000000000000000000 ) ) ;
#42016 = CARTESIAN_POINT ( 'NONE',  ( 20.85212586905262100, -130.9402397935870965, 5.500000000000000000 ) ) ;
#42017 = AXIS2_PLACEMENT_3D ( 'NONE', #25324, #40285, #14323 ) ;
#42018 = CARTESIAN_POINT ( 'NONE',  ( 11.99999999999999822, 55.20638768913831029, -51.02545421589267960 ) ) ;
#42019 = DIRECTION ( 'NONE',  ( 0.000000000000000000, -0.8526401643540970632, 0.5224985647159411384 ) ) ;
#42020 = ORIENTED_EDGE ( 'NONE', *, *, #12655, .T. ) ;
#42022 = EDGE_CURVE ( 'NONE', #41093, #18791, #38482, .T. ) ;
#42021 = DIRECTION ( 'NONE',  ( 0.000000000000000000, 0.000000000000000000, 1.000000000000000000 ) ) ;
#42023 = DIRECTION ( 'NONE',  ( 0.000000000000000000, 0.9969173337331282969, -0.07845909572784179331 ) ) ;
#42024 = ADVANCED_FACE ( 'NONE', ( #37959 ), #45529, .T. ) ;
#42025 = CARTESIAN_POINT ( 'NONE',  ( -3.000000000000000000, -0.9646360437375307573, 23.52805723605590060 ) ) ;
#42026 = DIRECTION ( 'NONE',  ( 0.7273375899149793211, -0.6862798483830554463, 0.000000000000000000 ) ) ;
#42027 = LINE ( 'NONE', #7987, #45082 ) ;
#42028 = CYLINDRICAL_SURFACE ( 'NONE', #33422, 77.49899999999999523 ) ;
#42029 = AXIS2_PLACEMENT_3D ( 'NONE', #46819, #35067, #47055 ) ;
#42030 = ORIENTED_EDGE ( 'NONE', *, *, #18608, .F. ) ;
#42031 = DIRECTION ( 'NONE',  ( 0.000000000000000000, -0.9723699203976789995, 0.2334453638558957322 ) ) ;
#42032 = CARTESIAN_POINT ( 'NONE',  ( 11.99999999999999822, -18.89407956138204980, -75.16055320797050854 ) ) ;
#42033 = EDGE_CURVE ( 'NONE', #32185, #23315, #739, .T. ) ;
#42034 = ORIENTED_EDGE ( 'NONE', *, *, #46245, .T. ) ;
#42035 = DIRECTION ( 'NONE',  ( -1.000000000000000000, 0.000000000000000000, 0.000000000000000000 ) ) ;
#42036 = ORIENTED_EDGE ( 'NONE', *, *, #8871, .F. ) ;
#42037 = VECTOR ( 'NONE', #35266, 1000.000000000000000 ) ;
#42038 = EDGE_LOOP ( 'NONE', ( #40067, #1572, #32371, #17507 ) ) ;
#42039 = DIRECTION ( 'NONE',  ( 0.000000000000000000, -0.1045284632676558301, -0.9945218953682731788 ) ) ;
#42040 = ORIENTED_EDGE ( 'NONE', *, *, #40807, .T. ) ;
#42041 = VECTOR ( 'NONE', #25201, 1000.000000000000000 ) ;
#42042 = EDGE_LOOP ( 'NONE', ( #18237, #35005, #19861, #31338 ) ) ;
#42043 = ADVANCED_FACE ( 'NONE', ( #34032 ), #14959, .T. ) ;
#42044 = LINE ( 'NONE', #30789, #46844 ) ;
#42045 = DIRECTION ( 'NONE',  ( -1.000000000000000000, 0.000000000000000000, 0.000000000000000000 ) ) ;
#42046 = EDGE_CURVE ( 'NONE', #23067, #1692, #9540, .T. ) ;
#42047 = ORIENTED_EDGE ( 'NONE', *, *, #37382, .T. ) ;
#42048 = VERTEX_POINT ( 'NONE', #41883 ) ;
#42049 = EDGE_CURVE ( 'NONE', #39253, #41636, #30380, .T. ) ;
#42050 = CARTESIAN_POINT ( 'NONE',  ( 0.000000000000000000, 0.000000000000000000, 0.000000000000000000 ) ) ;
#42051 = CARTESIAN_POINT ( 'NONE',  ( 11.99999999999999822, -41.76937507738831812, 62.50329211542423025 ) ) ;
#42052 = CIRCLE ( 'NONE', #2184, 77.49900000000002365 ) ;
#42053 = LINE ( 'NONE', #31050, #27488 ) ;
#42054 = ORIENTED_EDGE ( 'NONE', *, *, #46555, .T. ) ;
#42055 = CARTESIAN_POINT ( 'NONE',  ( 20.85212586905262100, -130.9402397935870965, -5.500000000000000000 ) ) ;
#42056 = ORIENTED_EDGE ( 'NONE', *, *, #34471, .F. ) ;
#42057 = VERTEX_POINT ( 'NONE', #45294 ) ;
#42058 = CARTESIAN_POINT ( 'NONE',  ( 9.984461079971730157, -95.40710393340120277, 5.500000000000000000 ) ) ;
#42059 = CYLINDRICAL_SURFACE ( 'NONE', #8474, 16.00000000000000000 ) ;
#42060 = EDGE_LOOP ( 'NONE', ( #18183, #35387, #47610, #18412 ) ) ;
#42061 = CIRCLE ( 'NONE', #5311, 31.99999999999998224 ) ;
#42062 = DIRECTION ( 'NONE',  ( 0.000000000000000000, -1.000000000000000000, -1.040834085586084257E-14 ) ) ;
#42063 = EDGE_CURVE ( 'NONE', #39780, #1692, #22309, .T. ) ;
#42064 = CYLINDRICAL_SURFACE ( 'NONE', #23664, 31.99999999999999289 ) ;
#42065 = ORIENTED_EDGE ( 'NONE', *, *, #3950, .T. ) ;
#42066 = EDGE_CURVE ( 'NONE', #39318, #31838, #44812, .T. ) ;
#42067 = EDGE_CURVE ( 'NONE', #40235, #31834, #29106, .T. ) ;
#42068 = ORIENTED_EDGE ( 'NONE', *, *, #34867, .F. ) ;
#42069 = DIRECTION ( 'NONE',  ( -1.000000000000000000, -0.000000000000000000, 0.000000000000000000 ) ) ;
#42070 = CARTESIAN_POINT ( 'NONE',  ( 10.00000000000000000, -49.70050353004846500, -59.46389618802017907 ) ) ;
#42071 = ORIENTED_EDGE ( 'NONE', *, *, #37539, .F. ) ;
#42072 = CARTESIAN_POINT ( 'NONE',  ( -10.94538922500103162, 0.000000000000000000, 0.000000000000000000 ) ) ;
#42073 = ORIENTED_EDGE ( 'NONE', *, *, #25018, .T. ) ;
#42074 = LINE ( 'NONE', #5845, #46522 ) ;
#42075 = DIRECTION ( 'NONE',  ( -1.000000000000000000, 0.000000000000000000, 0.000000000000000000 ) ) ;
#42076 = FACE_OUTER_BOUND ( 'NONE', #25440, .T. ) ;
#42077 = EDGE_CURVE ( 'NONE', #25452, #20812, #28144, .T. ) ;
#42078 = CARTESIAN_POINT ( 'NONE',  ( 10.00000000000000000, 40.68715046381944234, -10.41901085202036192 ) ) ;
#42079 = AXIS2_PLACEMENT_3D ( 'NONE', #4160, #11741, #22994 ) ;
#42080 = CARTESIAN_POINT ( 'NONE',  ( 0.000000000000000000, 16.23288003029497162, 33.80338159004289622 ) ) ;
#42081 = CARTESIAN_POINT ( 'NONE',  ( -4.653126046682595884, -146.1313684676804314, 5.500000000000000000 ) ) ;
#42082 = CARTESIAN_POINT ( 'NONE',  ( 12.00000000000000000, 8.688484142254226938, 21.88630264137359305 ) ) ;
#42083 = EDGE_CURVE ( 'NONE', #33821, #43090, #43958, .T. ) ;
#42084 = DIRECTION ( 'NONE',  ( 0.000000000000000000, -0.9876883405951394357, 0.1564344650402205716 ) ) ;
#42085 =( NAMED_UNIT ( * ) SI_UNIT ( $, .STERADIAN. ) SOLID_ANGLE_UNIT ( ) );
#42086 = DIRECTION ( 'NONE',  ( -1.000000000000000000, 0.000000000000000000, 0.000000000000000000 ) ) ;
#42087 = EDGE_LOOP ( 'NONE', ( #16158, #1365, #4264, #15515 ) ) ;
#42088 = CARTESIAN_POINT ( 'NONE',  ( -3.000000000000000000, 22.07842321921492612, -8.187992925817130896 ) ) ;
#42089 = ORIENTED_EDGE ( 'NONE', *, *, #11509, .F. ) ;
#42090 = VECTOR ( 'NONE', #1176, 1000.000000000000114 ) ;
#42091 = CARTESIAN_POINT ( 'NONE',  ( -103.9230484541323705, -180.0000000000004832, 5.500000000000000000 ) ) ;
#42092 = DIRECTION ( 'NONE',  ( 0.9038112904824853189, -0.4279312458752977388, 0.000000000000000000 ) ) ;
#42093 = EDGE_LOOP ( 'NONE', ( #44824, #8264, #40428, #12530 ) ) ;
#42094 = EDGE_CURVE ( 'NONE', #3743, #10782, #15048, .T. ) ;
#42095 = EDGE_CURVE ( 'NONE', #37633, #23915, #36891, .T. ) ;
#42096 = DIRECTION ( 'NONE',  ( 1.000000000000000000, 0.000000000000000000, 0.000000000000000000 ) ) ;
#42097 = ORIENTED_EDGE ( 'NONE', *, *, #4100, .F. ) ;
#42098 = EDGE_CURVE ( 'NONE', #488, #12997, #15807, .T. ) ;
#42099 = ORIENTED_EDGE ( 'NONE', *, *, #12961, .F. ) ;
#42100 = ORIENTED_EDGE ( 'NONE', *, *, #28732, .F. ) ;
#42101 = VERTEX_POINT ( 'NONE', #35730 ) ;
#42102 = ORIENTED_EDGE ( 'NONE', *, *, #37311, .T. ) ;
#42103 = ADVANCED_FACE ( 'NONE', ( #31108 ), #20076, .T. ) ;
#42104 = VECTOR ( 'NONE', #40942, 1000.000000000000000 ) ;
#42105 = DIRECTION ( 'NONE',  ( -0.000000000000000000, -0.000000000000000000, -1.000000000000000000 ) ) ;
#42106 = ORIENTED_EDGE ( 'NONE', *, *, #16026, .T. ) ;
#42107 = LINE ( 'NONE', #38432, #13753 ) ;
#42108 = ORIENTED_EDGE ( 'NONE', *, *, #22162, .T. ) ;
#42109 = CARTESIAN_POINT ( 'NONE',  ( 11.99999999999999822, 77.49459641780886443, -0.8261519478433960728 ) ) ;
#42110 = ORIENTED_EDGE ( 'NONE', *, *, #22026, .F. ) ;
#42111 = DIRECTION ( 'NONE',  ( 0.4279312458752976833, 0.9038112904824853189, -0.000000000000000000 ) ) ;
#42112 = DIRECTION ( 'NONE',  ( 0.000000000000000000, 0.8910065241883690090, -0.4539904997395446395 ) ) ;
#42113 = ORIENTED_EDGE ( 'NONE', *, *, #6957, .F. ) ;
#42114 = ADVANCED_FACE ( 'NONE', ( #5633 ), #16405, .T. ) ;
#42115 = CARTESIAN_POINT ( 'NONE',  ( 10.00000000000000000, -33.00180498840060039, 17.80606268964528027 ) ) ;
#42116 = EDGE_CURVE ( 'NONE', #16392, #1080, #18122, .T. ) ;
#42117 = ORIENTED_EDGE ( 'NONE', *, *, #20163, .F. ) ;
#42118 = CARTESIAN_POINT ( 'NONE',  ( 10.00000000000000000, 0.000000000000000000, 0.000000000000000000 ) ) ;
#42119 = DIRECTION ( 'NONE',  ( 0.000000000000000000, 0.000000000000000000, 1.000000000000000000 ) ) ;
#42120 = VERTEX_POINT ( 'NONE', #1480 ) ;
#42121 = CARTESIAN_POINT ( 'NONE',  ( 0.000000000000000000, 0.000000000000000000, 0.000000000000000000 ) ) ;
#42122 = ORIENTED_EDGE ( 'NONE', *, *, #19217, .F. ) ;
#42123 = AXIS2_PLACEMENT_3D ( 'NONE', #46745, #35717, #24213 ) ;
#42124 = VERTEX_POINT ( 'NONE', #46990 ) ;
#42125 = FACE_OUTER_BOUND ( 'NONE', #28246, .T. ) ;
#42126 = CARTESIAN_POINT ( 'NONE',  ( 11.99999999999999822, 46.54456581323888997, -59.03342792756214408 ) ) ;
#42127 = AXIS2_PLACEMENT_3D ( 'NONE', #42328, #31572, #5136 ) ;
#42128 = DIRECTION ( 'NONE',  ( 1.000000000000000000, 0.000000000000000000, 0.000000000000000000 ) ) ;
#42129 = DIRECTION ( 'NONE',  ( 0.000000000000000000, 0.4067366430758000417, -0.9135454576426009776 ) ) ;
#42130 = DIRECTION ( 'NONE',  ( -1.000000000000000000, -0.000000000000000000, -0.000000000000000000 ) ) ;
#42131 = AXIS2_PLACEMENT_3D ( 'NONE', #25855, #36154, #18273 ) ;
#42132 = CARTESIAN_POINT ( 'NONE',  ( 11.99999999999999822, 75.11764819372149304, 29.05362095685338275 ) ) ;
#42133 = DIRECTION ( 'NONE',  ( -1.000000000000000000, 0.000000000000000000, -0.000000000000000000 ) ) ;
#42134 = EDGE_CURVE ( 'NONE', #37030, #28298, #11132, .T. ) ;
#42135 = CARTESIAN_POINT ( 'NONE',  ( -3.961125083139900749, -143.2122702051246677, 5.500000000000000000 ) ) ;
#42136 = PLANE ( 'NONE',  #38779 ) ;
#42137 = CARTESIAN_POINT ( 'NONE',  ( 11.99999999999999822, -74.65374052328654386, 8.840884882374837161 ) ) ;
#42138 = FACE_OUTER_BOUND ( 'NONE', #32400, .T. ) ;
#42139 = AXIS2_PLACEMENT_3D ( 'NONE', #29317, #47433, #44245 ) ;
#42140 = DIRECTION ( 'NONE',  ( -0.000000000000000000, -0.000000000000000000, 1.000000000000000000 ) ) ;
#42141 = CARTESIAN_POINT ( 'NONE',  ( -34.02017708624681092, -130.1428571428571388, -2.500000000000000000 ) ) ;
#42142 = DIRECTION ( 'NONE',  ( 0.000000000000000000, 0.000000000000000000, 1.000000000000000000 ) ) ;
#42143 = ORIENTED_EDGE ( 'NONE', *, *, #5024, .F. ) ;
#42144 = PLANE ( 'NONE',  #35440 ) ;
#42145 = EDGE_LOOP ( 'NONE', ( #10256, #37336, #14209, #14215 ) ) ;
#42146 = LINE ( 'NONE', #23304, #16633 ) ;
#42147 = FACE_OUTER_BOUND ( 'NONE', #15927, .T. ) ;
#42148 = ORIENTED_EDGE ( 'NONE', *, *, #34429, .T. ) ;
#42149 = AXIS2_PLACEMENT_3D ( 'NONE', #14983, #6908, #29899 ) ;
#42150 = CIRCLE ( 'NONE', #15560, 32.00000000000000711 ) ;
#42151 = ORIENTED_EDGE ( 'NONE', *, *, #30554, .F. ) ;
#42152 = LINE ( 'NONE', #34079, #9735 ) ;
#42154 = EDGE_CURVE ( 'NONE', #27731, #9130, #39412, .T. ) ;
#42153 = VECTOR ( 'NONE', #27346, 1000.000000000000000 ) ;
#42155 = ORIENTED_EDGE ( 'NONE', *, *, #26060, .F. ) ;
#42156 = EDGE_CURVE ( 'NONE', #13285, #36037, #28308, .T. ) ;
#42157 = DIRECTION ( 'NONE',  ( 1.000000000000000000, 0.000000000000000000, 0.000000000000000000 ) ) ;
#42158 = AXIS2_PLACEMENT_3D ( 'NONE', #9966, #9716, #6070 ) ;
#42159 = CARTESIAN_POINT ( 'NONE',  ( 5.000000000000000000, -32.34446384429951138, -26.79245525562750530 ) ) ;
#42160 = ORIENTED_EDGE ( 'NONE', *, *, #30753, .T. ) ;
#42162 = ORIENTED_EDGE ( 'NONE', *, *, #6221, .T. ) ;
#42161 = DIRECTION ( 'NONE',  ( 9.814797785686868941E-17, 1.000000000000000000, -0.000000000000000000 ) ) ;
#42163 = VERTEX_POINT ( 'NONE', #4899 ) ;
#42164 = EDGE_CURVE ( 'NONE', #30064, #14957, #12706, .T. ) ;
#42165 = CARTESIAN_POINT ( 'NONE',  ( 10.00000000000000000, 33.80338159004283938, 16.23288003029508886 ) ) ;
#42166 = DIRECTION ( 'NONE',  ( -1.000000000000000000, 0.000000000000000000, 0.000000000000000000 ) ) ;
#42167 = ADVANCED_FACE ( 'NONE', ( #27669 ), #42844, .T. ) ;
#42168 = DIRECTION ( 'NONE',  ( 0.000000000000000000, 0.000000000000000000, 1.000000000000000000 ) ) ;
#42169 = LINE ( 'NONE', #34099, #10897 ) ;
#42170 = ORIENTED_EDGE ( 'NONE', *, *, #25136, .F. ) ;
#42171 = DIRECTION ( 'NONE',  ( -1.000000000000000000, -0.000000000000000000, -0.000000000000000000 ) ) ;
#42172 = EDGE_LOOP ( 'NONE', ( #40783, #16612, #20233, #45898 ) ) ;
#42173 = VERTEX_POINT ( 'NONE', #34757 ) ;
#42174 = EDGE_CURVE ( 'NONE', #46331, #26170, #14226, .T. ) ;
#42175 = DIRECTION ( 'NONE',  ( 1.000000000000000000, 0.000000000000000000, 0.000000000000000000 ) ) ;
#42176 = CARTESIAN_POINT ( 'NONE',  ( 0.000000000000000000, 16.83928648764923253, 16.46020748918050458 ) ) ;
#42177 = DIRECTION ( 'NONE',  ( 0.000000000000000000, 0.000000000000000000, 1.000000000000000000 ) ) ;
#42178 = CARTESIAN_POINT ( 'NONE',  ( 11.99999999999999822, -66.50666863322028632, 39.78640506895582973 ) ) ;
#42179 = ORIENTED_EDGE ( 'NONE', *, *, #42899, .F. ) ;
#42180 = LINE ( 'NONE', #5462, #21381 ) ;
#42181 = CARTESIAN_POINT ( 'NONE',  ( 10.00000000000000000, 22.48208911017551515, -35.47612816024499693 ) ) ;
#42182 = DIRECTION ( 'NONE',  ( 0.000000000000000000, 0.000000000000000000, 1.000000000000000000 ) ) ;
#42183 = CARTESIAN_POINT ( 'NONE',  ( 10.00000000000000000, 59.03342792756328095, -46.54456581323744757 ) ) ;
#42184 = ADVANCED_FACE ( 'NONE', ( #24469 ), #24000, .T. ) ;
#42186 = CIRCLE ( 'NONE', #7795, 31.99999999999998579 ) ;
#42185 = CARTESIAN_POINT ( 'NONE',  ( 0.000000000000000000, -120.0000000000000000, 5.500000000000000888 ) ) ;
#42187 = CIRCLE ( 'NONE', #48426, 82.00000000000000000 ) ;
#42188 = CARTESIAN_POINT ( 'NONE',  ( 10.00000000000000000, 26.08949754953062694, -27.05870788708203989 ) ) ;
#42189 = DIRECTION ( 'NONE',  ( 0.000000000000000000, 0.000000000000000000, 1.000000000000000000 ) ) ;
#42190 = AXIS2_PLACEMENT_3D ( 'NONE', #24274, #24984, #4533 ) ;
#42191 = LINE ( 'NONE', #46116, #26773 ) ;
#42192 = CARTESIAN_POINT ( 'NONE',  ( 15.00000000000000000, -0.9646360437375368635, -23.52805723605589705 ) ) ;
#42193 = VECTOR ( 'NONE', #22672, 1000.000000000000000 ) ;
#42194 = ORIENTED_EDGE ( 'NONE', *, *, #18152, .T. ) ;
#42195 = VERTEX_POINT ( 'NONE', #38935 ) ;
#42196 = CYLINDRICAL_SURFACE ( 'NONE', #23804, 31.99999999999998579 ) ;
#42197 = ORIENTED_EDGE ( 'NONE', *, *, #33598, .F. ) ;
#42198 = ORIENTED_EDGE ( 'NONE', *, *, #28398, .F. ) ;
#42199 = DIRECTION ( 'NONE',  ( -0.4796670183876317051, 0.8774505977381971134, 0.000000000000000000 ) ) ;
#42200 = FACE_OUTER_BOUND ( 'NONE', #42852, .T. ) ;
#42201 = ORIENTED_EDGE ( 'NONE', *, *, #36084, .F. ) ;
#42202 = ADVANCED_FACE ( 'NONE', ( #19818 ), #1719, .T. ) ;
#42203 = ORIENTED_EDGE ( 'NONE', *, *, #18464, .F. ) ;
#42204 = EDGE_CURVE ( 'NONE', #38800, #5676, #8774, .T. ) ;
#42205 = ORIENTED_EDGE ( 'NONE', *, *, #41526, .T. ) ;
#42206 = EDGE_CURVE ( 'NONE', #33821, #32703, #24944, .T. ) ;
#42207 = ORIENTED_EDGE ( 'NONE', *, *, #36938, .T. ) ;
#42208 = EDGE_CURVE ( 'NONE', #17290, #10381, #10354, .T. ) ;
#42209 = CIRCLE ( 'NONE', #7051, 31.99999999999998224 ) ;
#42210 = PLANE ( 'NONE',  #46494 ) ;
#42211 = EDGE_CURVE ( 'NONE', #26390, #43790, #174, .T. ) ;
#42212 = VECTOR ( 'NONE', #41440, 1000.000000000000000 ) ;
#42213 = EDGE_CURVE ( 'NONE', #10349, #37347, #35365, .T. ) ;
#42214 = CARTESIAN_POINT ( 'NONE',  ( 10.00000000000000000, 27.75498641678786527, -31.52238457039571173 ) ) ;
#42215 = LINE ( 'NONE', #8673, #43359 ) ;
#42216 = AXIS2_PLACEMENT_3D ( 'NONE', #5379, #13444, #46251 ) ;
#42217 = VERTEX_POINT ( 'NONE', #2912 ) ;
#42218 = CARTESIAN_POINT ( 'NONE',  ( 6.377742925735834234, -145.7647898336708181, -5.500000000000000000 ) ) ;
#42219 = ORIENTED_EDGE ( 'NONE', *, *, #4232, .T. ) ;
#42220 = ORIENTED_EDGE ( 'NONE', *, *, #37069, .F. ) ;
#42221 = VECTOR ( 'NONE', #28431, 1000.000000000000000 ) ;
#42222 = DIRECTION ( 'NONE',  ( -1.000000000000000000, -0.000000000000000000, 0.000000000000000000 ) ) ;
#42223 = CARTESIAN_POINT ( 'NONE',  ( 11.99999999999999822, 75.11764819372149304, -2.946379043146603482 ) ) ;
#42224 = AXIS2_PLACEMENT_3D ( 'NONE', #29710, #37541, #15752 ) ;
#42225 = DIRECTION ( 'NONE',  ( 0.000000000000000000, 0.000000000000000000, 1.000000000000000000 ) ) ;
#42226 = ORIENTED_EDGE ( 'NONE', *, *, #31629, .T. ) ;
#42227 = VERTEX_POINT ( 'NONE', #21989 ) ;
#42228 = ORIENTED_EDGE ( 'NONE', *, *, #38814, .T. ) ;
#42229 = VECTOR ( 'NONE', #30148, 1000.000000000000000 ) ;
#42230 = CARTESIAN_POINT ( 'NONE',  ( 10.00000000000000000, 62.50329211542494789, -41.76937507738723099 ) ) ;
#42231 = VERTEX_POINT ( 'NONE', #21524 ) ;
#42232 = EDGE_CURVE ( 'NONE', #34023, #19441, #36202, .T. ) ;
#42233 = CYLINDRICAL_SURFACE ( 'NONE', #23856, 77.49899999999999523 ) ;
#42234 = CARTESIAN_POINT ( 'NONE',  ( 11.99999999999999822, 50.95692526931329525, 58.39081064771768581 ) ) ;
#42235 = CARTESIAN_POINT ( 'NONE',  ( 2.500000000000000444, 8.494897427831771708, -19.01812422950394676 ) ) ;
#42236 = CARTESIAN_POINT ( 'NONE',  ( 10.00000000000000000, -23.16143007188376757, -73.95703589263997912 ) ) ;
#42237 = CARTESIAN_POINT ( 'NONE',  ( 0.000000000000000000, -12.93880638057258814, -76.41127070299285151 ) ) ;
#42238 = CARTESIAN_POINT ( 'NONE',  ( 0.000000000000000000, -17.67226234102849958, 33.17418723428301774 ) ) ;
#42239 = CARTESIAN_POINT ( 'NONE',  ( -3.000000000000000000, -20.55727247249748046, 16.78983467731285018 ) ) ;
#42240 = CARTESIAN_POINT ( 'NONE',  ( 11.99999999999999822, 20.41045688087930898, -72.35160999960793049 ) ) ;
#42241 = DIRECTION ( 'NONE',  ( -1.000000000000000000, -0.000000000000000000, 0.000000000000000000 ) ) ;
#42242 = FACE_OUTER_BOUND ( 'NONE', #42655, .T. ) ;
#42243 = EDGE_CURVE ( 'NONE', #39592, #48218, #17598, .T. ) ;
#42244 = CARTESIAN_POINT ( 'NONE',  ( 15.00000000000000000, 16.61724383029390140, 20.69703378468902955 ) ) ;
#42245 = ORIENTED_EDGE ( 'NONE', *, *, #2355, .F. ) ;
#42246 = ORIENTED_EDGE ( 'NONE', *, *, #7946, .T. ) ;
#42247 = DIRECTION ( 'NONE',  ( 1.000000000000000000, 0.000000000000000000, 0.000000000000000000 ) ) ;
#42248 = DIRECTION ( 'NONE',  ( 0.000000000000000000, 0.000000000000000000, 1.000000000000000000 ) ) ;
#42249 = CARTESIAN_POINT ( 'NONE',  ( 10.00000000000000000, 0.9569279952884557350, -2.499999999999984457 ) ) ;
#42250 = CARTESIAN_POINT ( 'NONE',  ( 12.00000000000000000, -10.45096189432314127, 21.10159698893440350 ) ) ;
#42251 = ADVANCED_FACE ( 'NONE', ( #36677 ), #32302, .T. ) ;
#42252 = DIRECTION ( 'NONE',  ( -0.000000000000000000, -0.4067366430757898277, -0.9135454576426055295 ) ) ;
#42253 = DIRECTION ( 'NONE',  ( 0.000000000000000000, 0.000000000000000000, -1.000000000000000000 ) ) ;
#42254 = AXIS2_PLACEMENT_3D ( 'NONE', #26336, #41268, #7723 ) ;
#42255 = EDGE_CURVE ( 'NONE', #30674, #16029, #32541, .T. ) ;
#42256 = CARTESIAN_POINT ( 'NONE',  ( 10.00000000000000000, -27.13269053701114331, 25.88420570971391754 ) ) ;
#42257 = CARTESIAN_POINT ( 'NONE',  ( 11.99999999999999822, 49.70050353004975818, -59.46389618801909904 ) ) ;
#42258 = VECTOR ( 'NONE', #791, 1000.000000000000000 ) ;
#42259 = EDGE_LOOP ( 'NONE', ( #22020, #29080, #38393, #2635 ) ) ;
#42260 = VECTOR ( 'NONE', #3528, 1000.000000000000000 ) ;
#42261 = CIRCLE ( 'NONE', #44601, 42.00000000000000000 ) ;
#42262 = ORIENTED_EDGE ( 'NONE', *, *, #6507, .T. ) ;
#42263 = DIRECTION ( 'NONE',  ( -1.000000000000000000, -0.000000000000000000, -0.000000000000000000 ) ) ;
#42264 = CIRCLE ( 'NONE', #32921, 21.00000000000000000 ) ;
#42265 = ORIENTED_EDGE ( 'NONE', *, *, #1957, .F. ) ;
#42266 = AXIS2_PLACEMENT_3D ( 'NONE', #32380, #6671, #21600 ) ;
#42267 = EDGE_CURVE ( 'NONE', #42195, #28886, #2663, .T. ) ;
#42268 = ORIENTED_EDGE ( 'NONE', *, *, #9821, .T. ) ;
#42269 = AXIS2_PLACEMENT_3D ( 'NONE', #46466, #27376, #23692 ) ;
#42270 = EDGE_CURVE ( 'NONE', #40406, #13266, #33260, .T. ) ;
#42271 = VERTEX_POINT ( 'NONE', #39886 ) ;
#42272 = DIRECTION ( 'NONE',  ( -1.000000000000000000, 0.000000000000000000, 0.000000000000000000 ) ) ;
#42273 = EDGE_CURVE ( 'NONE', #13379, #19466, #21752, .T. ) ;
#42274 = ORIENTED_EDGE ( 'NONE', *, *, #14746, .T. ) ;
#42275 = ORIENTED_EDGE ( 'NONE', *, *, #48451, .T. ) ;
#42276 = EDGE_CURVE ( 'NONE', #43286, #11880, #32988, .T. ) ;
#42277 = CARTESIAN_POINT ( 'NONE',  ( -12.49999999999999822, -120.0000000000000000, -125.0000000000000000 ) ) ;
#42278 = CYLINDRICAL_SURFACE ( 'NONE', #1926, 82.00000000000000000 ) ;
#42279 = EDGE_LOOP ( 'NONE', ( #17688, #39056, #21195, #42373 ) ) ;
#42280 = EDGE_LOOP ( 'NONE', ( #39342, #25428, #16453, #3707 ) ) ;
#42281 = CARTESIAN_POINT ( 'NONE',  ( 10.00000000000000000, -35.53030884539077050, -12.26510123303296851 ) ) ;
#42283 = ORIENTED_EDGE ( 'NONE', *, *, #2874, .F. ) ;
#42282 = CARTESIAN_POINT ( 'NONE',  ( 10.00000000000000000, 72.35432306680455383, 20.40083707023012494 ) ) ;
#42284 = VECTOR ( 'NONE', #1836, 1000.000000000000000 ) ;
#42285 = DIRECTION ( 'NONE',  ( 0.000000000000000000, 0.000000000000000000, 1.000000000000000000 ) ) ;
#42286 = ORIENTED_EDGE ( 'NONE', *, *, #23360, .T. ) ;
#42288 = EDGE_LOOP ( 'NONE', ( #38694, #3698, #9036, #18803 ) ) ;
#42287 = AXIS2_PLACEMENT_3D ( 'NONE', #7781, #184, #41567 ) ;
#42289 = DIRECTION ( 'NONE',  ( 0.1736481776669309696, -0.9848077530122080203, 0.000000000000000000 ) ) ;
#42290 = VERTEX_POINT ( 'NONE', #43326 ) ;
#42291 = ORIENTED_EDGE ( 'NONE', *, *, #43924, .T. ) ;
#42292 = DIRECTION ( 'NONE',  ( 1.000000000000000000, 0.000000000000000000, -0.000000000000000000 ) ) ;
#42293 = AXIS2_PLACEMENT_3D ( 'NONE', #9297, #39416, #46992 ) ;
#42294 = VECTOR ( 'NONE', #18064, 1000.000000000000000 ) ;
#42295 = CARTESIAN_POINT ( 'NONE',  ( -3.000000000000000000, -3.948201729842038432, -23.21447184625298021 ) ) ;
#42296 = VERTEX_POINT ( 'NONE', #9779 ) ;
#42297 = CARTESIAN_POINT ( 'NONE',  ( 0.000000000000000000, -33.80338159004273280, -16.23288003029533044 ) ) ;
#42298 = DIRECTION ( 'NONE',  ( 1.000000000000000000, 0.000000000000000000, 0.000000000000000000 ) ) ;
#42299 = CARTESIAN_POINT ( 'NONE',  ( 0.000000000000000000, 22.64427369931169309, 30.00120703465213623 ) ) ;
#42300 = ORIENTED_EDGE ( 'NONE', *, *, #24401, .T. ) ;
#42301 = AXIS2_PLACEMENT_3D ( 'NONE', #8519, #1674, #16595 ) ;
#42302 = VERTEX_POINT ( 'NONE', #43789 ) ;
#42303 = CIRCLE ( 'NONE', #846, 31.99999999999999289 ) ;
#42304 = CARTESIAN_POINT ( 'NONE',  ( 10.00000000000000000, 35.38097989696512968, 12.42422080174651100 ) ) ;
#42305 = DIRECTION ( 'NONE',  ( -1.000000000000000000, 0.000000000000000000, 0.000000000000000000 ) ) ;
#42306 = VERTEX_POINT ( 'NONE', #39665 ) ;
#42307 = CIRCLE ( 'NONE', #17994, 77.49900000000000944 ) ;
#42308 = LINE ( 'NONE', #8521, #22074 ) ;
#42309 = ORIENTED_EDGE ( 'NONE', *, *, #13825, .F. ) ;
#42310 = CARTESIAN_POINT ( 'NONE',  ( 10.00000000000000000, 0.000000000000000000, 0.000000000000000000 ) ) ;
#42311 = CYLINDRICAL_SURFACE ( 'NONE', #31824, 77.49899999999999523 ) ;
#42312 = CARTESIAN_POINT ( 'NONE',  ( -3.000000000000000000, -18.13022148937243472, -15.02647892043568767 ) ) ;
#42313 = DIRECTION ( 'NONE',  ( -1.000000000000000000, -0.000000000000000000, 0.000000000000000000 ) ) ;
#42314 = DIRECTION ( 'NONE',  ( -1.000000000000000000, 0.000000000000000000, 0.000000000000000000 ) ) ;
#42315 = CARTESIAN_POINT ( 'NONE',  ( 11.99999999999999822, 59.75363087400153006, -56.15606465354896670 ) ) ;
#42316 = DIRECTION ( 'NONE',  ( 0.000000000000000000, -0.8910065241883627918, -0.4539904997395569630 ) ) ;
#42317 = DIRECTION ( 'NONE',  ( 1.000000000000000000, 0.000000000000000000, 0.000000000000000000 ) ) ;
#42318 = ORIENTED_EDGE ( 'NONE', *, *, #35146, .T. ) ;
#42319 = DIRECTION ( 'NONE',  ( -1.000000000000000000, 0.000000000000000000, 0.000000000000000000 ) ) ;
#42320 = ORIENTED_EDGE ( 'NONE', *, *, #1289, .T. ) ;
#42321 = ORIENTED_EDGE ( 'NONE', *, *, #7786, .F. ) ;
#42322 = CIRCLE ( 'NONE', #47750, 31.99999999999999289 ) ;
#42323 = LINE ( 'NONE', #8779, #15203 ) ;
#42324 = ORIENTED_EDGE ( 'NONE', *, *, #4537, .F. ) ;
#42325 = CIRCLE ( 'NONE', #39961, 42.00000000000000000 ) ;
#42326 = VECTOR ( 'NONE', #31285, 1000.000000000000000 ) ;
#42327 = EDGE_LOOP ( 'NONE', ( #12636, #12446, #502, #27917 ) ) ;
#42328 = CARTESIAN_POINT ( 'NONE',  ( 0.000000000000000000, 17.67226234102826510, 33.17418723428314564 ) ) ;
#42329 = EDGE_CURVE ( 'NONE', #45805, #33355, #44002, .T. ) ;
#42330 = FACE_OUTER_BOUND ( 'NONE', #10581, .T. ) ;
#42331 = VERTEX_POINT ( 'NONE', #21031 ) ;
#42332 = AXIS2_PLACEMENT_3D ( 'NONE', #7260, #36636, #3097 ) ;
#42333 = EDGE_CURVE ( 'NONE', #44620, #12035, #40131, .T. ) ;
#42334 = AXIS2_PLACEMENT_3D ( 'NONE', #33860, #26766, #34332 ) ;
#42335 = ADVANCED_FACE ( 'NONE', ( #13703 ), #36447, .T. ) ;
#42336 = CARTESIAN_POINT ( 'NONE',  ( 10.00000000000000000, -39.78640506895653317, 66.50666863321987421 ) ) ;
#42337 = EDGE_LOOP ( 'NONE', ( #27173, #21452, #21912, #46965 ) ) ;
#42338 = AXIS2_PLACEMENT_3D ( 'NONE', #23021, #45525, #12019 ) ;
#42339 = ORIENTED_EDGE ( 'NONE', *, *, #10847, .F. ) ;
#42340 = VERTEX_POINT ( 'NONE', #26163 ) ;
#42341 = ORIENTED_EDGE ( 'NONE', *, *, #43061, .F. ) ;
#42342 = EDGE_CURVE ( 'NONE', #29523, #13751, #12734, .T. ) ;
#42343 = ORIENTED_EDGE ( 'NONE', *, *, #24259, .F. ) ;
#42344 = LINE ( 'NONE', #28135, #10240 ) ;
#42345 = ORIENTED_EDGE ( 'NONE', *, *, #39810, .F. ) ;
#42346 = CARTESIAN_POINT ( 'NONE',  ( 4.999999999999999112, -40.98264845739755202, 9.188173127307159405 ) ) ;
#42347 = VERTEX_POINT ( 'NONE', #4610 ) ;
#42348 = CARTESIAN_POINT ( 'NONE',  ( 10.00000000000000000, 71.21200624218795383, 40.65526001592638039 ) ) ;
#42349 = DIRECTION ( 'NONE',  ( -1.000000000000000000, -0.000000000000000000, -0.000000000000000000 ) ) ;
#42350 = DIRECTION ( 'NONE',  ( -1.000000000000000000, 0.000000000000000000, 0.000000000000000000 ) ) ;
#42351 = VERTEX_POINT ( 'NONE', #41578 ) ;
#42352 = DIRECTION ( 'NONE',  ( -1.000000000000000000, -0.000000000000000000, 0.000000000000000000 ) ) ;
#42353 = ORIENTED_EDGE ( 'NONE', *, *, #1723, .F. ) ;
#42354 = EDGE_CURVE ( 'NONE', #25698, #10994, #36923, .T. ) ;
#42355 = AXIS2_PLACEMENT_3D ( 'NONE', #7984, #653, #15582 ) ;
#42356 = CARTESIAN_POINT ( 'NONE',  ( 15.00000000000000000, 20.85821328998756385, 10.92862929874494249 ) ) ;
#42357 = CYLINDRICAL_SURFACE ( 'NONE', #29747, 16.00000000000000000 ) ;
#42358 = ORIENTED_EDGE ( 'NONE', *, *, #4645, .T. ) ;
#42359 = CIRCLE ( 'NONE', #41556, 42.00000000000000000 ) ;
#42360 = CARTESIAN_POINT ( 'NONE',  ( 11.99999999999999822, -46.53671651293991118, 59.03961581697383565 ) ) ;
#42361 = ORIENTED_EDGE ( 'NONE', *, *, #26048, .T. ) ;
#42362 = ORIENTED_EDGE ( 'NONE', *, *, #40565, .F. ) ;
#42363 = DIRECTION ( 'NONE',  ( -0.000000000000000000, -0.000000000000000000, -1.000000000000000000 ) ) ;
#42364 = DIRECTION ( 'NONE',  ( 0.000000000000000000, 0.000000000000000000, 1.000000000000000000 ) ) ;
#42365 = VECTOR ( 'NONE', #18384, 1000.000000000000000 ) ;
#42366 = DIRECTION ( 'NONE',  ( 0.000000000000000000, 0.000000000000000000, 1.000000000000000000 ) ) ;
#42367 = DIRECTION ( 'NONE',  ( -1.000000000000000000, 0.000000000000000000, 0.000000000000000000 ) ) ;
#42368 = DIRECTION ( 'NONE',  ( 0.4279312458752976833, 0.9038112904824853189, -0.000000000000000000 ) ) ;
#42369 = DIRECTION ( 'NONE',  ( 0.000000000000000000, 0.9510565162951544194, -0.3090169943749446757 ) ) ;
#42371 = EDGE_CURVE ( 'NONE', #34724, #6953, #36169, .T. ) ;
#42370 = DIRECTION ( 'NONE',  ( 0.000000000000000000, -0.8090169943749401238, -0.5877852522924831291 ) ) ;
#42372 = DIRECTION ( 'NONE',  ( 1.000000000000000000, 0.000000000000000000, -0.000000000000000000 ) ) ;
#42373 = ORIENTED_EDGE ( 'NONE', *, *, #667, .T. ) ;
#42374 = EDGE_CURVE ( 'NONE', #1298, #4855, #27586, .T. ) ;
#42375 = FACE_OUTER_BOUND ( 'NONE', #30006, .T. ) ;
#42376 = CARTESIAN_POINT ( 'NONE',  ( 10.00000000000000000, 18.89407956138256139, 75.16055320797038064 ) ) ;
#42377 = FACE_OUTER_BOUND ( 'NONE', #24107, .T. ) ;
#42378 = AXIS2_PLACEMENT_3D ( 'NONE', #687, #44747, #30805 ) ;
#42379 = EDGE_CURVE ( 'NONE', #37110, #40588, #6478, .T. ) ;
#42380 = DIRECTION ( 'NONE',  ( -1.000000000000000000, 0.000000000000000000, 0.000000000000000000 ) ) ;
#42381 = DIRECTION ( 'NONE',  ( 0.000000000000000000, 1.000000000000000000, 3.491481338843133355E-15 ) ) ;
#42382 = DIRECTION ( 'NONE',  ( 0.000000000000000000, -0.8090169943749531134, 0.5877852522924653655 ) ) ;
#42383 = DIRECTION ( 'NONE',  ( -0.000000000000000000, 0.5000000000000038858, 0.8660254037844363761 ) ) ;
#42384 = ADVANCED_FACE ( 'NONE', ( #45476 ), #41105, .T. ) ;
#42385 = VERTEX_POINT ( 'NONE', #37414 ) ;
#42386 = CARTESIAN_POINT ( 'NONE',  ( 0.000000000000000000, 21.53537804866081373, 30.80686688397018358 ) ) ;
#42387 = ORIENTED_EDGE ( 'NONE', *, *, #19769, .T. ) ;
#42388 = CARTESIAN_POINT ( 'NONE',  ( 10.00000000000000000, 58.39081064771823293, -50.95692526931266286 ) ) ;
#42389 = AXIS2_PLACEMENT_3D ( 'NONE', #37914, #26900, #41351 ) ;
#42390 = SHAPE_DEFINITION_REPRESENTATION ( #2266, #37520 ) ;
#42391 = LINE ( 'NONE', #10291, #25306 ) ;
#42392 = VERTEX_POINT ( 'NONE', #15398 ) ;
#42393 = ADVANCED_FACE ( 'NONE', ( #25905 ), #4387, .T. ) ;
#42394 = EDGE_CURVE ( 'NONE', #31838, #7679, #45243, .T. ) ;
#42395 = CIRCLE ( 'NONE', #32232, 31.99999999999999289 ) ;
#42396 = AXIS2_PLACEMENT_3D ( 'NONE', #14423, #2426, #40598 ) ;
#42397 = ORIENTED_EDGE ( 'NONE', *, *, #2251, .T. ) ;
#42398 = CARTESIAN_POINT ( 'NONE',  ( 0.9774260708577211521, -121.1378217241763622, -2.500000000000000000 ) ) ;
#42399 = VERTEX_POINT ( 'NONE', #19511 ) ;
#42400 = CYLINDRICAL_SURFACE ( 'NONE', #16446, 31.99999999999998579 ) ;
#42401 = VECTOR ( 'NONE', #30341, 1000.000000000000000 ) ;
#42402 = ADVANCED_FACE ( 'NONE', ( #19044 ), #11960, .F. ) ;
#42403 = DIRECTION ( 'NONE',  ( 0.000000000000000000, -0.07845909572783058006, -0.9969173337331290741 ) ) ;
#42404 = EDGE_LOOP ( 'NONE', ( #47092, #14778, #3927, #14941 ) ) ;
#42405 = CARTESIAN_POINT ( 'NONE',  ( 10.00000000000000000, 78.73519480814985627, -22.90783923731548910 ) ) ;
#42406 = ORIENTED_EDGE ( 'NONE', *, *, #26790, .F. ) ;
#42408 = ORIENTED_EDGE ( 'NONE', *, *, #4943, .F. ) ;
#42407 = DIRECTION ( 'NONE',  ( -0.000000000000000000, -1.000000000000000000, -1.445602896647339656E-16 ) ) ;
#42409 = AXIS2_PLACEMENT_3D ( 'NONE', #28066, #31506, #46425 ) ;
#42410 = ORIENTED_EDGE ( 'NONE', *, *, #36623, .T. ) ;
#42411 = PLANE ( 'NONE',  #34518 ) ;
#42412 = CARTESIAN_POINT ( 'NONE',  ( 11.99999999999999822, -58.39081064771713869, -50.95692526931392052 ) ) ;
#42413 = DIRECTION ( 'NONE',  ( -0.000000000000000000, -1.000000000000000000, -1.445602896647339656E-16 ) ) ;
#42414 = CARTESIAN_POINT ( 'NONE',  ( 0.000000000000000000, -6.555932627142143865, -37.01155633439065440 ) ) ;
#42415 = DIRECTION ( 'NONE',  ( -1.000000000000000000, 0.000000000000000000, 0.000000000000000000 ) ) ;
#42416 = ORIENTED_EDGE ( 'NONE', *, *, #31157, .F. ) ;
#42417 = CARTESIAN_POINT ( 'NONE',  ( 6.000000000000000000, 74.18225833017888249, 34.94270380257665209 ) ) ;
#42418 = ORIENTED_EDGE ( 'NONE', *, *, #1225, .F. ) ;
#42419 = CARTESIAN_POINT ( 'NONE',  ( 0.000000000000000000, 56.15606465354959198, 59.75363087400094741 ) ) ;
#42420 = AXIS2_PLACEMENT_3D ( 'NONE', #22258, #14184, #11245 ) ;
#42421 = DIRECTION ( 'NONE',  ( -1.000000000000000000, 0.000000000000000000, 0.000000000000000000 ) ) ;
#42422 = DIRECTION ( 'NONE',  ( -1.000000000000000000, 0.000000000000000000, -0.000000000000000000 ) ) ;
#42423 = LINE ( 'NONE', #42178, #2407 ) ;
#42424 = VERTEX_POINT ( 'NONE', #44511 ) ;
#42425 = DIRECTION ( 'NONE',  ( 0.000000000000000000, 0.000000000000000000, 1.000000000000000000 ) ) ;
#42426 = DIRECTION ( 'NONE',  ( 0.000000000000000000, -0.9135454576426050854, -0.4067366430757908824 ) ) ;
#42427 = DIRECTION ( 'NONE',  ( 0.000000000000000000, 0.000000000000000000, -1.000000000000000000 ) ) ;
#42428 = AXIS2_PLACEMENT_3D ( 'NONE', #12350, #823, #15767 ) ;
#42429 = DIRECTION ( 'NONE',  ( -1.000000000000000000, 0.000000000000000000, 0.000000000000000000 ) ) ;
#42430 = DIRECTION ( 'NONE',  ( -1.000000000000000000, -0.000000000000000000, -0.000000000000000000 ) ) ;
#42431 = VECTOR ( 'NONE', #7627, 1000.000000000000000 ) ;
#42432 = EDGE_CURVE ( 'NONE', #21150, #40230, #3882, .T. ) ;
#42433 = CARTESIAN_POINT ( 'NONE',  ( 10.05638427806949586, -98.76043467366159234, 2.500000000000000000 ) ) ;
#42434 = DIRECTION ( 'NONE',  ( 0.000000000000000000, -0.3090169943749548342, 0.9510565162951511997 ) ) ;
#42435 = CARTESIAN_POINT ( 'NONE',  ( -3.000000000000000000, -13.04903810567647682, -19.60159698893442481 ) ) ;
#42436 = CIRCLE ( 'NONE', #7235, 31.99999999999999289 ) ;
#42437 = EDGE_CURVE ( 'NONE', #30863, #7503, #196, .T. ) ;
#42438 = VECTOR ( 'NONE', #27371, 1000.000000000000000 ) ;
#42439 = CARTESIAN_POINT ( 'NONE',  ( 0.000000000000000000, -25.60904388321916514, -6.976881207771517879 ) ) ;
#42440 = DIRECTION ( 'NONE',  ( -1.000000000000000000, -0.000000000000000000, -0.000000000000000000 ) ) ;
#42441 = EDGE_CURVE ( 'NONE', #1423, #38423, #37752, .T. ) ;
#42442 = AXIS2_PLACEMENT_3D ( 'NONE', #12699, #45490, #20034 ) ;
#42443 = EDGE_LOOP ( 'NONE', ( #15715, #40169, #4520, #41547 ) ) ;
#42444 = CARTESIAN_POINT ( 'NONE',  ( 10.00000000000000000, 74.65491531819118620, -8.830959090342659579 ) ) ;
#42445 = CIRCLE ( 'NONE', #44805, 77.49900000000002365 ) ;
#42446 = ORIENTED_EDGE ( 'NONE', *, *, #21723, .T. ) ;
#42447 = LINE ( 'NONE', #5728, #11151 ) ;
#42448 = AXIS2_PLACEMENT_3D ( 'NONE', #16502, #35097, #2069 ) ;
#42449 = DIRECTION ( 'NONE',  ( -1.000000000000000000, 0.000000000000000000, 0.000000000000000000 ) ) ;
#42450 = VERTEX_POINT ( 'NONE', #29824 ) ;
#42451 = EDGE_CURVE ( 'NONE', #33614, #25524, #38527, .T. ) ;
#42452 = EDGE_CURVE ( 'NONE', #43260, #26882, #30082, .T. ) ;
#42453 = VERTEX_POINT ( 'NONE', #7307 ) ;
#42454 = VECTOR ( 'NONE', #28176, 1000.000000000000000 ) ;
#42455 = VERTEX_POINT ( 'NONE', #41341 ) ;
#42456 = ORIENTED_EDGE ( 'NONE', *, *, #15758, .T. ) ;
#42457 = CIRCLE ( 'NONE', #16637, 35.50000000000000711 ) ;
#42458 = EDGE_CURVE ( 'NONE', #4911, #32425, #4142, .T. ) ;
#42459 = DIRECTION ( 'NONE',  ( -1.000000000000000000, 0.000000000000000000, 0.000000000000000000 ) ) ;
#42460 = FACE_OUTER_BOUND ( 'NONE', #40140, .T. ) ;
#42461 = AXIS2_PLACEMENT_3D ( 'NONE', #15095, #34167, #15348 ) ;
#42462 = VECTOR ( 'NONE', #3699, 1000.000000000000000 ) ;
#42463 = CARTESIAN_POINT ( 'NONE',  ( 11.99999999999999822, 0.000000000000000000, 0.000000000000000000 ) ) ;
#42464 = EDGE_LOOP ( 'NONE', ( #15997, #11892, #38474, #7979 ) ) ;
#42465 = DIRECTION ( 'NONE',  ( 0.9730327541852493711, -0.2306669878475637314, 0.000000000000000000 ) ) ;
#42466 = CIRCLE ( 'NONE', #33864, 11.59999999999999787 ) ;
#42467 = VERTEX_POINT ( 'NONE', #22721 ) ;
#42468 = DIRECTION ( 'NONE',  ( 0.000000000000000000, 0.000000000000000000, 1.000000000000000000 ) ) ;
#42469 = DIRECTION ( 'NONE',  ( 0.000000000000000000, 0.000000000000000000, 1.000000000000000000 ) ) ;
#42470 = FACE_OUTER_BOUND ( 'NONE', #30378, .T. ) ;
#42471 = EDGE_LOOP ( 'NONE', ( #36216, #36743, #10230, #16308 ) ) ;
#42472 = CIRCLE ( 'NONE', #6628, 82.00000000000000000 ) ;
#42473 = VECTOR ( 'NONE', #12114, 1000.000000000000000 ) ;
#42474 = ORIENTED_EDGE ( 'NONE', *, *, #33585, .T. ) ;
#42475 = EDGE_LOOP ( 'NONE', ( #21462, #29264, #5169, #15457 ) ) ;
#42476 = CARTESIAN_POINT ( 'NONE',  ( 0.000000000000000000, -44.99326035066006568, -68.55367621811190304 ) ) ;
#42477 = ORIENTED_EDGE ( 'NONE', *, *, #48043, .F. ) ;
#42478 = DIRECTION ( 'NONE',  ( 0.000000000000000000, 0.000000000000000000, 1.000000000000000000 ) ) ;
#42479 = AXIS2_PLACEMENT_3D ( 'NONE', #30185, #45106, #41670 ) ;
#42480 = PLANE ( 'NONE',  #31112 ) ;
#42481 = DIRECTION ( 'NONE',  ( 0.000000000000000000, 0.000000000000000000, 1.000000000000000000 ) ) ;
#42482 = CARTESIAN_POINT ( 'NONE',  ( -14.87942725330654348, -141.9795960975983178, 2.500000000000000000 ) ) ;
#42483 = CARTESIAN_POINT ( 'NONE',  ( 0.000000000000000000, 65.64334221924909230, 41.19522573413756561 ) ) ;
#42484 = DIRECTION ( 'NONE',  ( 0.000000000000000000, 0.000000000000000000, 1.000000000000000000 ) ) ;
#42485 = AXIS2_PLACEMENT_3D ( 'NONE', #36072, #10623, #47800 ) ;
#42486 = DIRECTION ( 'NONE',  ( -0.000000000000000000, 0.9781476007338069101, -0.2079116908177532363 ) ) ;
#42487 = ORIENTED_EDGE ( 'NONE', *, *, #5850, .T. ) ;
#42488 = DIRECTION ( 'NONE',  ( 1.000000000000000000, 0.000000000000000000, 0.000000000000000000 ) ) ;
#42489 = CARTESIAN_POINT ( 'NONE',  ( 10.00000000000000000, -0.6853352020793173072, 37.58145647212453611 ) ) ;
#42490 = DIRECTION ( 'NONE',  ( 0.000000000000000000, -0.7431448254773954654, 0.6691306063588569053 ) ) ;
#42491 = DIRECTION ( 'NONE',  ( 0.000000000000000000, 0.3090169943749482839, -0.9510565162951533091 ) ) ;
#42492 = ORIENTED_EDGE ( 'NONE', *, *, #7540, .F. ) ;
#42493 = DIRECTION ( 'NONE',  ( 0.000000000000000000, 0.5877852522924684742, 0.8090169943749506709 ) ) ;
#42494 = EDGE_CURVE ( 'NONE', #24283, #42613, #35399, .T. ) ;
#42495 = DIRECTION ( 'NONE',  ( 1.000000000000000000, -0.000000000000000000, -0.000000000000000000 ) ) ;
#42496 = DIRECTION ( 'NONE',  ( 1.000000000000000000, 0.000000000000000000, -0.000000000000000000 ) ) ;
#42497 = EDGE_CURVE ( 'NONE', #13195, #40856, #46707, .T. ) ;
#42498 = ADVANCED_FACE ( 'NONE', ( #9247 ), #4854, .T. ) ;
#42499 = CARTESIAN_POINT ( 'NONE',  ( 50.00005079999999680, 0.000000000000000000, 0.000000000000000000 ) ) ;
#42501 = CIRCLE ( 'NONE', #33088, 42.00000000000000000 ) ;
#42500 = CARTESIAN_POINT ( 'NONE',  ( 5.822613034544236399, -142.8165987265839760, 5.500000000000000000 ) ) ;
#42502 = ADVANCED_FACE ( 'NONE', ( #9009 ), #31297, .T. ) ;
#42503 = DIRECTION ( 'NONE',  ( 0.000000000000000000, 0.000000000000000000, 1.000000000000000000 ) ) ;
#42504 = DIRECTION ( 'NONE',  ( -1.000000000000000000, 0.000000000000000000, 0.000000000000000000 ) ) ;
#42506 = EDGE_CURVE ( 'NONE', #37720, #47426, #42436, .T. ) ;
#42505 = VERTEX_POINT ( 'NONE', #5581 ) ;
#42507 = CIRCLE ( 'NONE', #11230, 31.99999999999998579 ) ;
#42508 = AXIS2_PLACEMENT_3D ( 'NONE', #41520, #38326, #45193 ) ;
#42509 = VECTOR ( 'NONE', #35764, 1000.000000000000000 ) ;
#42510 = ORIENTED_EDGE ( 'NONE', *, *, #4372, .T. ) ;
#42511 = DIRECTION ( 'NONE',  ( 0.000000000000000000, 0.000000000000000000, 1.000000000000000000 ) ) ;
#42512 = EDGE_LOOP ( 'NONE', ( #14187, #27122 ) ) ;
#42513 = ORIENTED_EDGE ( 'NONE', *, *, #3713, .F. ) ;
#42514 = EDGE_CURVE ( 'NONE', #8618, #14862, #27373, .T. ) ;
#42515 = AXIS2_PLACEMENT_3D ( 'NONE', #32803, #36488, #6641 ) ;
#42516 = AXIS2_PLACEMENT_3D ( 'NONE', #14262, #14752, #48274 ) ;
#42517 = EDGE_CURVE ( 'NONE', #13398, #361, #2548, .T. ) ;
#42518 = AXIS2_PLACEMENT_3D ( 'NONE', #37728, #4207, #34052 ) ;
#42519 = EDGE_LOOP ( 'NONE', ( #17294, #42877, #14376, #12267 ) ) ;
#42520 = AXIS2_PLACEMENT_3D ( 'NONE', #11519, #41375, #41606 ) ;
#42521 = DIRECTION ( 'NONE',  ( -1.000000000000000000, 0.000000000000000000, 0.000000000000000000 ) ) ;
#42522 = EDGE_LOOP ( 'NONE', ( #26392, #37876, #40379, #18918 ) ) ;
#42523 = CIRCLE ( 'NONE', #44858, 82.00000000000000000 ) ;
#42524 = VERTEX_POINT ( 'NONE', #39349 ) ;
#42525 = ADVANCED_FACE ( 'NONE', ( #15870 ), #16356, .T. ) ;
#42526 = CYLINDRICAL_SURFACE ( 'NONE', #28114, 12.49999999999999645 ) ;
#42528 = VERTEX_POINT ( 'NONE', #9478 ) ;
#42527 = CARTESIAN_POINT ( 'NONE',  ( 5.000000000000000000, -26.79245525562738095, 32.34446384429961796 ) ) ;
#42529 = ORIENTED_EDGE ( 'NONE', *, *, #18169, .T. ) ;
#42530 = ORIENTED_EDGE ( 'NONE', *, *, #47613, .T. ) ;
#42531 = VECTOR ( 'NONE', #29795, 1000.000000000000000 ) ;
#42532 = LINE ( 'NONE', #24650, #9248 ) ;
#42533 = CARTESIAN_POINT ( 'NONE',  ( -23.54415474984308787, -120.4156646670583086, -5.500000000000000000 ) ) ;
#42534 = EDGE_CURVE ( 'NONE', #28171, #10773, #1181, .T. ) ;
#42536 = CARTESIAN_POINT ( 'NONE',  ( 12.00000000000000000, -25.60904388321915803, 6.976881207771517879 ) ) ;
#42535 = CIRCLE ( 'NONE', #26111, 16.00000000000000355 ) ;
#42537 = VERTEX_POINT ( 'NONE', #5835 ) ;
#42538 = ORIENTED_EDGE ( 'NONE', *, *, #1187, .F. ) ;
#42539 = CARTESIAN_POINT ( 'NONE',  ( 0.000000000000000000, -33.17418723428319538, 17.67226234102814431 ) ) ;
#42540 = VERTEX_POINT ( 'NONE', #1921 ) ;
#42541 = VERTEX_POINT ( 'NONE', #31060 ) ;
#42542 = DIRECTION ( 'NONE',  ( -1.000000000000000000, -0.000000000000000000, -0.000000000000000000 ) ) ;
#42543 = AXIS2_PLACEMENT_3D ( 'NONE', #19300, #37665, #15408 ) ;
#42544 = CARTESIAN_POINT ( 'NONE',  ( -22.53294031248082163, -134.0273518838794757, -5.500000000000000000 ) ) ;
#42545 = CIRCLE ( 'NONE', #22203, 12.50000000000000000 ) ;
#42546 = ORIENTED_EDGE ( 'NONE', *, *, #23929, .F. ) ;
#42547 = CARTESIAN_POINT ( 'NONE',  ( 12.00000000000000000, 14.60985201121729737, 18.46759930825687590 ) ) ;
#42548 = CARTESIAN_POINT ( 'NONE',  ( 10.00000000000000000, -26.08949754953005495, -27.05870788708258701 ) ) ;
#42549 = DIRECTION ( 'NONE',  ( 0.000000000000000000, 0.000000000000000000, 1.000000000000000000 ) ) ;
#42550 = ORIENTED_EDGE ( 'NONE', *, *, #45939, .F. ) ;
#42551 = VERTEX_POINT ( 'NONE', #34949 ) ;
#42552 = CARTESIAN_POINT ( 'NONE',  ( 4.999999999999999112, 9.188173127307294408, 40.98264845739752360 ) ) ;
#42553 = CARTESIAN_POINT ( 'NONE',  ( 0.000000000000000000, 0.000000000000000000, 53.20000000000001705 ) ) ;
#42554 = AXIS2_PLACEMENT_3D ( 'NONE', #20772, #10226, #6559 ) ;
#42555 = AXIS2_PLACEMENT_3D ( 'NONE', #25513, #29669, #22341 ) ;
#42556 = VERTEX_POINT ( 'NONE', #16591 ) ;
#42557 = VECTOR ( 'NONE', #23227, 1000.000000000000000 ) ;
#42558 = EDGE_CURVE ( 'NONE', #41796, #36392, #30812, .T. ) ;
#42559 = LINE ( 'NONE', #39118, #39762 ) ;
#42560 = ORIENTED_EDGE ( 'NONE', *, *, #29612, .T. ) ;
#42561 = CIRCLE ( 'NONE', #33942, 31.99999999999999289 ) ;
#42562 = DIRECTION ( 'NONE',  ( 0.000000000000000000, 0.000000000000000000, 1.000000000000000000 ) ) ;
#42563 = EDGE_CURVE ( 'NONE', #18691, #34257, #12213, .T. ) ;
#42564 = CARTESIAN_POINT ( 'NONE',  ( 10.00000000000000000, 0.000000000000000000, 0.000000000000000000 ) ) ;
#42565 = DIRECTION ( 'NONE',  ( 0.000000000000000000, 0.000000000000000000, 1.000000000000000000 ) ) ;
#42566 = LINE ( 'NONE', #31076, #40897 ) ;
#42567 = AXIS2_PLACEMENT_3D ( 'NONE', #3837, #7976, #38098 ) ;
#42568 = ADVANCED_FACE ( 'NONE', ( #922 ), #20753, .F. ) ;
#42569 = LINE ( 'NONE', #46481, #11850 ) ;
#42570 = DIRECTION ( 'NONE',  ( -1.000000000000000000, 0.000000000000000000, 0.000000000000000000 ) ) ;
#42571 = DIRECTION ( 'NONE',  ( -1.000000000000000000, -0.000000000000000000, 0.000000000000000000 ) ) ;
#42572 = DIRECTION ( 'NONE',  ( 0.000000000000000000, 0.7604059656000276002, 0.6494480483301875440 ) ) ;
#42573 = EDGE_CURVE ( 'NONE', #28599, #46997, #47108, .T. ) ;
#42574 = LINE ( 'NONE', #37929, #20580 ) ;
#42575 = CIRCLE ( 'NONE', #17532, 16.00000000000000000 ) ;
#42576 = ORIENTED_EDGE ( 'NONE', *, *, #44281, .T. ) ;
#42577 = VERTEX_POINT ( 'NONE', #35429 ) ;
#42578 = VERTEX_POINT ( 'NONE', #13165 ) ;
#42579 = VECTOR ( 'NONE', #23224, 1000.000000000000000 ) ;
#42580 = LINE ( 'NONE', #4638, #37093 ) ;
#42581 = AXIS2_PLACEMENT_3D ( 'NONE', #8670, #26804, #19216 ) ;
#42582 = CIRCLE ( 'NONE', #12884, 31.99999999999999645 ) ;
#42583 = DIRECTION ( 'NONE',  ( -1.000000000000000000, 0.000000000000000000, 0.000000000000000000 ) ) ;
#42584 = CARTESIAN_POINT ( 'NONE',  ( 0.000000000000000000, 65.64334221924964652, -41.19522573413665611 ) ) ;
#42585 = ORIENTED_EDGE ( 'NONE', *, *, #4365, .T. ) ;
#42586 = CIRCLE ( 'NONE', #38680, 12.49999999999999645 ) ;
#42587 = VECTOR ( 'NONE', #30642, 1000.000000000000000 ) ;
#42588 = CIRCLE ( 'NONE', #12898, 31.99999999999999645 ) ;
#42589 = CARTESIAN_POINT ( 'NONE',  ( 0.000000000000000000, -66.50666863322028632, 39.78640506895582973 ) ) ;
#42590 = VECTOR ( 'NONE', #41933, 1000.000000000000000 ) ;
#42591 = ORIENTED_EDGE ( 'NONE', *, *, #28946, .T. ) ;
#42592 = ORIENTED_EDGE ( 'NONE', *, *, #1583, .T. ) ;
#42593 = VECTOR ( 'NONE', #45077, 1000.000000000000114 ) ;
#42594 = ORIENTED_EDGE ( 'NONE', *, *, #18217, .T. ) ;
#42595 = CIRCLE ( 'NONE', #5072, 16.00000000000000355 ) ;
#42596 = ADVANCED_FACE ( 'NONE', ( #28096 ), #42064, .T. ) ;
#42597 = LINE ( 'NONE', #42835, #20341 ) ;
#42598 = ORIENTED_EDGE ( 'NONE', *, *, #13830, .T. ) ;
#42599 = CARTESIAN_POINT ( 'NONE',  ( 10.00000000000000000, 0.000000000000000000, 0.000000000000000000 ) ) ;
#42600 = ORIENTED_EDGE ( 'NONE', *, *, #28424, .T. ) ;
#42601 = DIRECTION ( 'NONE',  ( -1.000000000000000000, -0.000000000000000000, -0.000000000000000000 ) ) ;
#42602 = DIRECTION ( 'NONE',  ( 0.000000000000000000, 0.000000000000000000, 1.000000000000000000 ) ) ;
#42603 = DIRECTION ( 'NONE',  ( 0.000000000000000000, 0.000000000000000000, 1.000000000000000000 ) ) ;
#42604 = EDGE_LOOP ( 'NONE', ( #24872, #8866, #4605, #2721 ) ) ;
#42605 = CARTESIAN_POINT ( 'NONE',  ( 0.000000000000000000, 0.000000000000000000, 0.000000000000000000 ) ) ;
#42606 = ORIENTED_EDGE ( 'NONE', *, *, #10228, .F. ) ;
#42607 = ORIENTED_EDGE ( 'NONE', *, *, #45847, .F. ) ;
#42608 = DIRECTION ( 'NONE',  ( -1.000000000000000000, -0.000000000000000000, 0.000000000000000000 ) ) ;
#42609 = EDGE_CURVE ( 'NONE', #16641, #17111, #38642, .T. ) ;
#42610 = CARTESIAN_POINT ( 'NONE',  ( 0.000000000000000000, 50.95692526931329525, 58.39081064771768581 ) ) ;
#42611 = VERTEX_POINT ( 'NONE', #1430 ) ;
#42612 = CARTESIAN_POINT ( 'NONE',  ( -3.000000000000000000, 0.000000000000000000, 0.000000000000000000 ) ) ;
#42613 = VERTEX_POINT ( 'NONE', #21469 ) ;
#42614 = ORIENTED_EDGE ( 'NONE', *, *, #2164, .T. ) ;
#42615 = ADVANCED_FACE ( 'NONE', ( #14126 ), #32957, .T. ) ;
#42616 = DIRECTION ( 'NONE',  ( -1.000000000000000000, -0.000000000000000000, -0.000000000000000000 ) ) ;
#42617 = AXIS2_PLACEMENT_3D ( 'NONE', #43396, #20146, #39730 ) ;
#42618 = CARTESIAN_POINT ( 'NONE',  ( -10.00000000000000000, 0.000000000000000000, 0.000000000000000000 ) ) ;
#42619 = ORIENTED_EDGE ( 'NONE', *, *, #28013, .T. ) ;
#42620 = DIRECTION ( 'NONE',  ( -1.000000000000000000, -0.000000000000000000, -0.000000000000000000 ) ) ;
#42621 = DIRECTION ( 'NONE',  ( 0.000000000000000000, 1.000000000000000000, 0.000000000000000000 ) ) ;
#42622 = CARTESIAN_POINT ( 'NONE',  ( 10.00000000000000000, 35.92658777277511462, 10.74501242461295014 ) ) ;
#42623 = EDGE_CURVE ( 'NONE', #929, #46997, #39283, .T. ) ;
#42624 = CARTESIAN_POINT ( 'NONE',  ( 89.17737905728634473, -39.70432723693593857, -5.500000000000000000 ) ) ;
#42625 = CARTESIAN_POINT ( 'NONE',  ( 10.00000000000000000, 33.80338159004307386, -16.23288003029461279 ) ) ;
#42626 = LINE ( 'NONE', #30889, #21627 ) ;
#42627 = VECTOR ( 'NONE', #28024, 1000.000000000000000 ) ;
#42628 = AXIS2_PLACEMENT_3D ( 'NONE', #11986, #35147, #16808 ) ;
#42629 = DIRECTION ( 'NONE',  ( 0.000000000000000000, 0.000000000000000000, 1.000000000000000000 ) ) ;
#42630 = CARTESIAN_POINT ( 'NONE',  ( 0.000000000000000000, 0.000000000000000000, -56.19999999999998863 ) ) ;
#42631 = CARTESIAN_POINT ( 'NONE',  ( 11.99999999999999822, 0.000000000000000000, 0.000000000000000000 ) ) ;
#42632 = ADVANCED_FACE ( 'NONE', ( #28581 ), #47417, .T. ) ;
#42633 = CIRCLE ( 'NONE', #24630, 77.49899999999999523 ) ;
#42634 = EDGE_CURVE ( 'NONE', #29332, #42541, #19729, .T. ) ;
#42635 = DIRECTION ( 'NONE',  ( 0.000000000000000000, 0.5877852522924684742, 0.8090169943749506709 ) ) ;
#42636 = DIRECTION ( 'NONE',  ( -1.000000000000000000, -0.000000000000000000, -0.000000000000000000 ) ) ;
#42637 = SURFACE_STYLE_USAGE ( .BOTH. , #19849 ) ;
#42638 = CARTESIAN_POINT ( 'NONE',  ( 11.99999999999999822, -76.69515212746036070, 29.01471420065536932 ) ) ;
#42639 = EDGE_LOOP ( 'NONE', ( #11243, #8429, #15393, #5062 ) ) ;
#42640 = VERTEX_POINT ( 'NONE', #43266 ) ;
#42641 = CIRCLE ( 'NONE', #16086, 12.50000000000000000 ) ;
#42642 = DIRECTION ( 'NONE',  ( -1.000000000000000000, 0.000000000000000000, 0.000000000000000000 ) ) ;
#42643 = DIRECTION ( 'NONE',  ( -1.000000000000000000, 0.000000000000000000, 0.000000000000000000 ) ) ;
#42644 = SHAPE_DEFINITION_REPRESENTATION ( #8582, #2782 ) ;
#42645 = AXIS2_PLACEMENT_3D ( 'NONE', #30346, #11738, #8051 ) ;
#42646 = DIRECTION ( 'NONE',  ( 0.000000000000000000, 0.000000000000000000, 1.000000000000000000 ) ) ;
#42647 = VERTEX_POINT ( 'NONE', #13891 ) ;
#42648 = CIRCLE ( 'NONE', #24640, 16.00000000000000000 ) ;
#42649 = CARTESIAN_POINT ( 'NONE',  ( 0.000000000000000000, 51.03279382321088065, 55.19960302592086521 ) ) ;
#42650 = VERTEX_POINT ( 'NONE', #28812 ) ;
#42651 =( NAMED_UNIT ( * ) PLANE_ANGLE_UNIT ( ) SI_UNIT ( $, .RADIAN. ) );
#42652 = ADVANCED_FACE ( 'NONE', ( #47883 ), #6074, .T. ) ;
#42653 = VECTOR ( 'NONE', #33375, 1000.000000000000000 ) ;
#42654 = DIRECTION ( 'NONE',  ( -0.000000000000000000, -0.000000000000000000, -1.000000000000000000 ) ) ;
#42655 = EDGE_LOOP ( 'NONE', ( #48420, #19917, #36478, #43953 ) ) ;
#42656 = CYLINDRICAL_SURFACE ( 'NONE', #27412, 31.99999999999998579 ) ;
#42657 = ORIENTED_EDGE ( 'NONE', *, *, #23585, .T. ) ;
#42659 = VERTEX_POINT ( 'NONE', #35682 ) ;
#42658 = CYLINDRICAL_SURFACE ( 'NONE', #434, 31.99999999999999289 ) ;
#42660 = EDGE_CURVE ( 'NONE', #30819, #40068, #20986, .T. ) ;
#42661 = ORIENTED_EDGE ( 'NONE', *, *, #39943, .F. ) ;
#42662 = VECTOR ( 'NONE', #29485, 1000.000000000000114 ) ;
#42663 = CARTESIAN_POINT ( 'NONE',  ( 11.99999999999999822, -74.65491531819111515, 23.16904090965678265 ) ) ;
#42664 = EDGE_CURVE ( 'NONE', #19470, #19520, #15116, .T. ) ;
#42665 = VECTOR ( 'NONE', #39727, 1000.000000000000000 ) ;
#42666 = DIRECTION ( 'NONE',  ( 0.000000000000000000, 0.000000000000000000, 1.000000000000000000 ) ) ;
#42667 = CARTESIAN_POINT ( 'NONE',  ( 5.999999999999999112, -56.15606465354916566, -59.75363087400133111 ) ) ;
#42668 = CARTESIAN_POINT ( 'NONE',  ( 11.99999999999999822, 0.000000000000000000, 0.000000000000000000 ) ) ;
#42669 = CARTESIAN_POINT ( 'NONE',  ( 0.000000000000000000, 74.74816331893477184, -33.71516098798660011 ) ) ;
#42670 = VERTEX_POINT ( 'NONE', #24667 ) ;
#42671 = CARTESIAN_POINT ( 'NONE',  ( 15.00000000000000000, -23.29833615347109088, -3.418703333116486665 ) ) ;
#42672 = ORIENTED_EDGE ( 'NONE', *, *, #20947, .T. ) ;
#42673 = DIRECTION ( 'NONE',  ( 1.000000000000000000, 0.000000000000000000, 0.000000000000000000 ) ) ;
#42674 = ORIENTED_EDGE ( 'NONE', *, *, #2445, .F. ) ;
#42675 = CYLINDRICAL_SURFACE ( 'NONE', #38626, 42.00000000000000000 ) ;
#42676 = AXIS2_PLACEMENT_3D ( 'NONE', #17318, #40097, #32271 ) ;
#42677 = CARTESIAN_POINT ( 'NONE',  ( 0.000000000000000000, -32.34446384429951138, -26.79245525562750530 ) ) ;
#42678 = CARTESIAN_POINT ( 'NONE',  ( 0.000000000000000000, 41.19522573413732403, 65.64334221924923440 ) ) ;
#42679 = ORIENTED_EDGE ( 'NONE', *, *, #36242, .F. ) ;
#42680 = LINE ( 'NONE', #4506, #44870 ) ;
#42681 = ADVANCED_FACE ( 'NONE', ( #17067 ), #6541, .T. ) ;
#42682 = DIRECTION ( 'NONE',  ( 0.000000000000000000, 0.000000000000000000, 1.000000000000000000 ) ) ;
#42683 = EDGE_CURVE ( 'NONE', #34175, #6187, #40554, .T. ) ;
#42684 = ADVANCED_FACE ( 'NONE', ( #2371 ), #2863, .F. ) ;
#42685 = LINE ( 'NONE', #15760, #61 ) ;
#42686 = DIRECTION ( 'NONE',  ( -1.000000000000000000, 0.000000000000000000, -0.000000000000000000 ) ) ;
#42687 = CARTESIAN_POINT ( 'NONE',  ( 0.000000000000000000, -5.256550761632340141, -77.32052557432847095 ) ) ;
#42688 = DIRECTION ( 'NONE',  ( 0.000000000000000000, 0.000000000000000000, -1.000000000000000000 ) ) ;
#42689 = DIRECTION ( 'NONE',  ( -1.000000000000000000, 0.000000000000000000, 0.000000000000000000 ) ) ;
#42690 = DIRECTION ( 'NONE',  ( 0.000000000000000000, 1.000000000000000000, 7.228014483236689653E-16 ) ) ;
#42691 = DIRECTION ( 'NONE',  ( -1.000000000000000000, 0.000000000000000000, 0.000000000000000000 ) ) ;
#42692 = DIRECTION ( 'NONE',  ( 1.000000000000000000, 0.000000000000000000, 0.000000000000000000 ) ) ;
#42693 = CIRCLE ( 'NONE', #15332, 37.49900000000000233 ) ;
#42694 = VERTEX_POINT ( 'NONE', #32253 ) ;
#42695 = AXIS2_PLACEMENT_3D ( 'NONE', #34752, #8799, #16173 ) ;
#42696 = DIRECTION ( 'NONE',  ( -1.000000000000000000, 0.000000000000000000, 0.000000000000000000 ) ) ;
#42697 = ORIENTED_EDGE ( 'NONE', *, *, #41611, .T. ) ;
#42698 = DIRECTION ( 'NONE',  ( -0.1850432970638656582, 0.9827303690289285187, 0.000000000000000000 ) ) ;
#42699 = VECTOR ( 'NONE', #30165, 1000.000000000000000 ) ;
#42700 = FACE_OUTER_BOUND ( 'NONE', #42519, .T. ) ;
#42701 = EDGE_LOOP ( 'NONE', ( #10978, #15867, #28550, #27657 ) ) ;
#42702 = CLOSED_SHELL ( 'NONE', ( #41456, #26479, #15976, #32741, #26511, #7172, #32348, #6321, #24359, #45093, #47888, #29510, #36208, #9393, #20408, #27687, #17013, #5928, #33118, #15262, #45363, #16867, #44197, #43159, #38643, #23368, #26302, #42632, #13380, #24429, #21861, #48224, #19817, #36303, #7332, #24865, #17573, #44885, #41854, #5919, #46127, #37143, #15816, #36797, #27828, #22494, #27278, #16322, #45047, #27778, #25694, #8131, #34608, #46597, #32272, #31880, #41904, #26324, #42652, #28696, #43705, #20781, #21724, #19124, #9132, #1899, #2279, #38532, #11137, #8545, #7993, #13202, #36642, #18110, #30243, #16100, #23310, #30436, #4329, #27297, #30736, #41392, #32479, #38020, #34014, #7812, #25133, #32113, #5485, #1522, #36310, #10196, #7940, #10002, #21454, #19279, #3744, #7466, #25736, #9560, #48406, #8850, #30237, #7111, #26624, #45423, #48058, #27405, #11517, #34362, #10057, #35761, #2416, #28634, #6274, #11463, #41604, #3420, #36724, #29383, #30329, #24167, #24914, #31818, #46981, #17268, #22598, #13873, #42114, #10453, #3253, #32170, #15641, #18178, #13241, #38516, #30666, #20990, #31854, #29825, #43172, #44157, #17334, #18836, #29841, #39288, #47790, #30131, #31949, #835, #35845, #36178, #21308, #4055, #23394, #29180, #277, #32626, #20118, #45153, #40141, #40574, #20608, #21220, #47831, #14944, #13247, #920, #8836, #37890, #15855, #608, #34459, #8095, #47030, #10901, #10810, #43936, #3119, #43815, #9272, #31250, #12300, #19333, #31649, #9162, #27973, #28558, #5875, #38918, #5440, #48293, #29402, #28330, #31278, #477, #35806, #7833, #40282, #9224, #21173, #20658, #39240, #25965, #39906, #38941, #15625, #37518, #43714, #41182, #17874, #20001, #36122, #26490, #2459, #34419, #11288, #13268, #7778, #8838, #3493, #40724, #43983, #46029, #29359, #752, #33317, #2267, #19066, #32037, #29814, #17792, #29014, #23044, #11367, #14235, #10667, #35346, #18100, #26637, #18408, #21624, #20961, #39848 ) ) ;
#42703 = FACE_OUTER_BOUND ( 'NONE', #2905, .T. ) ;
#42704 = AXIS2_PLACEMENT_3D ( 'NONE', #44120, #37004, #3482 ) ;
#42705 = EDGE_LOOP ( 'NONE', ( #38983, #13870, #45853, #33702 ) ) ;
#42706 = CIRCLE ( 'NONE', #46622, 31.99999999999999645 ) ;
#42707 = EDGE_LOOP ( 'NONE', ( #18729, #21497, #40810, #6065 ) ) ;
#42708 = EDGE_CURVE ( 'NONE', #17599, #48430, #30725, .T. ) ;
#42709 = CIRCLE ( 'NONE', #46624, 31.99999999999998579 ) ;
#42710 = EDGE_CURVE ( 'NONE', #5318, #39340, #44231, .T. ) ;
#42711 = CARTESIAN_POINT ( 'NONE',  ( 0.000000000000000000, -81.34940948281328588, -10.30890764327469000 ) ) ;
#42712 = LINE ( 'NONE', #27298, #26564 ) ;
#42714 = EDGE_LOOP ( 'NONE', ( #2651, #28286, #39636, #7546, #33832, #9093 ) ) ;
#42713 = LINE ( 'NONE', #46374, #27779 ) ;
#42715 = EDGE_CURVE ( 'NONE', #29358, #44403, #5719, .T. ) ;
#42716 = ORIENTED_EDGE ( 'NONE', *, *, #11908, .F. ) ;
#42717 = DIRECTION ( 'NONE',  ( -0.000000000000000000, -0.000000000000000000, -1.000000000000000000 ) ) ;
#42718 = ORIENTED_EDGE ( 'NONE', *, *, #41921, .T. ) ;
#42719 = ADVANCED_FACE ( 'NONE', ( #32492 ), #7014, .T. ) ;
#42720 = ORIENTED_EDGE ( 'NONE', *, *, #32509, .T. ) ;
#42721 = CARTESIAN_POINT ( 'NONE',  ( 10.00000000000000000, -37.22597642581153821, 10.79786254984320415 ) ) ;
#42722 = DIRECTION ( 'NONE',  ( 0.000000000000000000, -0.1564344650402381132, 0.9876883405951365491 ) ) ;
#42723 = DIRECTION ( 'NONE',  ( 0.000000000000000000, 0.000000000000000000, 1.000000000000000000 ) ) ;
#42725 = ORIENTED_EDGE ( 'NONE', *, *, #42839, .F. ) ;
#42724 = AXIS2_PLACEMENT_3D ( 'NONE', #24172, #32485, #43257 ) ;
#42726 = ORIENTED_EDGE ( 'NONE', *, *, #41435, .F. ) ;
#42727 = ORIENTED_EDGE ( 'NONE', *, *, #2709, .F. ) ;
#42728 = DIRECTION ( 'NONE',  ( -1.000000000000000000, -0.000000000000000000, 0.000000000000000000 ) ) ;
#42729 = ORIENTED_EDGE ( 'NONE', *, *, #5477, .T. ) ;
#42730 = CARTESIAN_POINT ( 'NONE',  ( 11.99999999999999822, 0.000000000000000000, 0.000000000000000000 ) ) ;
#42731 = AXIS2_PLACEMENT_3D ( 'NONE', #29842, #40866, #44774 ) ;
#42732 = DIRECTION ( 'NONE',  ( 0.000000000000000000, 0.9510565162951521989, 0.3090169943749515591 ) ) ;
#42733 = DIRECTION ( 'NONE',  ( -1.000000000000000000, -0.000000000000000000, 0.000000000000000000 ) ) ;
#42734 = CYLINDRICAL_SURFACE ( 'NONE', #19845, 16.00000000000000000 ) ;
#42735 = CARTESIAN_POINT ( 'NONE',  ( 15.00000000000000000, -3.948201729842032215, 23.21447184625297666 ) ) ;
#42736 = DIRECTION ( 'NONE',  ( -1.000000000000000000, 0.000000000000000000, 0.000000000000000000 ) ) ;
#42737 = FACE_OUTER_BOUND ( 'NONE', #18385, .T. ) ;
#42738 = ADVANCED_FACE ( 'NONE', ( #46937 ), #13405, .T. ) ;
#42739 = ORIENTED_EDGE ( 'NONE', *, *, #28784, .T. ) ;
#42740 = ADVANCED_FACE ( 'NONE', ( #36867 ), #19242, .T. ) ;
#42741 = FACE_OUTER_BOUND ( 'NONE', #23485, .T. ) ;
#42742 = CARTESIAN_POINT ( 'NONE',  ( -10.00000000000000000, 0.000000000000000000, 0.000000000000000000 ) ) ;
#42743 = CARTESIAN_POINT ( 'NONE',  ( 10.00000000000000000, -6.555932627142143865, -37.01155633439065440 ) ) ;
#42744 = LINE ( 'NONE', #5296, #47306 ) ;
#42745 = ORIENTED_EDGE ( 'NONE', *, *, #3798, .F. ) ;
#42746 = CIRCLE ( 'NONE', #10697, 12.49999999999999822 ) ;
#42747 = CARTESIAN_POINT ( 'NONE',  ( 0.000000000000000000, 0.000000000000000000, 0.000000000000000000 ) ) ;
#42748 = CARTESIAN_POINT ( 'NONE',  ( 10.00000000000000000, 0.000000000000000000, 0.000000000000000000 ) ) ;
#42749 = LINE ( 'NONE', #23897, #39370 ) ;
#42750 = AXIS2_PLACEMENT_3D ( 'NONE', #4348, #11678, #15830 ) ;
#42751 = CARTESIAN_POINT ( 'NONE',  ( 0.000000000000000000, 0.000000000000000000, 0.000000000000000000 ) ) ;
#42752 = CYLINDRICAL_SURFACE ( 'NONE', #39698, 82.00000000000000000 ) ;
#42753 = EDGE_CURVE ( 'NONE', #22493, #20399, #29181, .T. ) ;
#42754 = AXIS2_PLACEMENT_3D ( 'NONE', #39855, #2623, #36417 ) ;
#42755 = CARTESIAN_POINT ( 'NONE',  ( 10.00000000000000000, 0.000000000000000000, 0.000000000000000000 ) ) ;
#42756 = CARTESIAN_POINT ( 'NONE',  ( 0.000000000000000000, -80.28980883073769803, 16.65972982744906261 ) ) ;
#42757 = ORIENTED_EDGE ( 'NONE', *, *, #8016, .F. ) ;
#42758 = DIRECTION ( 'NONE',  ( -1.000000000000000000, 0.000000000000000000, -0.000000000000000000 ) ) ;
#42759 = ORIENTED_EDGE ( 'NONE', *, *, #35475, .T. ) ;
#42760 = CARTESIAN_POINT ( 'NONE',  ( 10.00000000000000000, -77.49459641780886443, -0.8261519478439277586 ) ) ;
#42761 = ORIENTED_EDGE ( 'NONE', *, *, #5715, .T. ) ;
#42762 = VERTEX_POINT ( 'NONE', #26352 ) ;
#42763 = VECTOR ( 'NONE', #33872, 1000.000000000000000 ) ;
#42764 = AXIS2_PLACEMENT_3D ( 'NONE', #4789, #34628, #1110 ) ;
#42765 = EDGE_LOOP ( 'NONE', ( #37014, #7900, #19796, #7602, #22676, #44493, #4783, #31601, #15430, #4770, #29590, #4639, #45413, #35431, #12990, #18972, #13895, #46437, #3446, #25657, #10322, #17124, #34268, #41111, #35709, #9164, #20502, #27046, #39331, #35119, #13382, #46845, #11944, #42510, #34514, #48357, #41877, #41801, #28450, #45305, #35861, #16871, #7443, #20672, #15632, #19096, #33909, #31857, #28961, #17407, #5735, #46440, #23380, #18117, #31781, #14065, #23127, #39080, #28676, #8724, #17924, #26645, #16450, #43400, #2695, #17530, #8956, #16676, #559, #42808, #14891, #16581, #36272, #39545, #14708, #20615, #33621, #20311, #16172, #48143, #9264, #20267, #36661, #27263, #15718, #46977, #41974, #10252, #1647, #18044, #23212, #7048, #37664, #48401, #6831, #427, #27985, #5788, #4340, #17398, #24452, #35936, #14220, #43873, #11087, #8828, #12435, #21378, #46929, #22488, #11668, #1710, #27369, #22716, #4056, #40813, #31115, #17669, #26941, #39809, #37438, #19284, #14088, #21782, #3457, #27300, #39880, #19506, #16303, #5803, #3072, #11170, #36438, #27416, #15137, #16952, #31950, #19667, #47695, #2397, #20171, #16598, #21332, #42274, #8498, #46692, #37776, #20212, #26209, #27719, #5522, #32207, #7943, #34750, #18684, #10951, #36777, #13882, #11212, #2336, #32764, #18370, #34791, #1363, #9965 ) ) ;
#42766 = ORIENTED_EDGE ( 'NONE', *, *, #25564, .F. ) ;
#42767 = CIRCLE ( 'NONE', #36489, 82.00000000000000000 ) ;
#42768 = DIRECTION ( 'NONE',  ( 0.000000000000000000, 0.000000000000000000, 1.000000000000000000 ) ) ;
#42769 = VERTEX_POINT ( 'NONE', #45421 ) ;
#42770 = ORIENTED_EDGE ( 'NONE', *, *, #13370, .T. ) ;
#42771 = DIRECTION ( 'NONE',  ( -1.000000000000000000, -0.000000000000000000, 0.000000000000000000 ) ) ;
#42772 = FACE_OUTER_BOUND ( 'NONE', #15437, .T. ) ;
#42773 = EDGE_CURVE ( 'NONE', #10102, #20850, #18745, .T. ) ;
#42774 = VERTEX_POINT ( 'NONE', #22669 ) ;
#42775 = ORIENTED_EDGE ( 'NONE', *, *, #33801, .F. ) ;
#42776 = VERTEX_POINT ( 'NONE', #3587 ) ;
#42777 = EDGE_CURVE ( 'NONE', #2211, #41993, #41522, .T. ) ;
#42778 = DIRECTION ( 'NONE',  ( 0.000000000000000000, -0.07845909572783053842, -0.9969173337331290741 ) ) ;
#42780 = VERTEX_POINT ( 'NONE', #145 ) ;
#42779 = CARTESIAN_POINT ( 'NONE',  ( -3.000000000000000000, -22.32062822937469804, -14.36278369418829826 ) ) ;
#42781 = AXIS2_PLACEMENT_3D ( 'NONE', #15531, #30465, #11860 ) ;
#42782 = DIRECTION ( 'NONE',  ( -1.000000000000000000, -0.000000000000000000, -0.000000000000000000 ) ) ;
#42783 = EDGE_LOOP ( 'NONE', ( #10830, #26579, #44339, #16043 ) ) ;
#42784 = FACE_OUTER_BOUND ( 'NONE', #18572, .T. ) ;
#42785 = EDGE_CURVE ( 'NONE', #25865, #17779, #43235, .T. ) ;
#42786 = ORIENTED_EDGE ( 'NONE', *, *, #3136, .T. ) ;
#42787 = ORIENTED_EDGE ( 'NONE', *, *, #32023, .F. ) ;
#42788 = CYLINDRICAL_SURFACE ( 'NONE', #45474, 82.00000000000000000 ) ;
#42789 = CARTESIAN_POINT ( 'NONE',  ( -10.00000000000000000, 0.000000000000000000, 0.000000000000000000 ) ) ;
#42790 = ORIENTED_EDGE ( 'NONE', *, *, #7931, .F. ) ;
#42791 = CARTESIAN_POINT ( 'NONE',  ( 11.99999999999999822, 76.41127070299290835, -12.93880638057234123 ) ) ;
#42792 = CARTESIAN_POINT ( 'NONE',  ( 0.000000000000000000, 0.000000000000000000, 0.000000000000000000 ) ) ;
#42793 = CARTESIAN_POINT ( 'NONE',  ( 12.00000000000000000, 16.83928648764945635, 16.46020748918027010 ) ) ;
#42794 = ORIENTED_EDGE ( 'NONE', *, *, #47052, .T. ) ;
#42795 = EDGE_LOOP ( 'NONE', ( #33549, #22473, #3145, #24809 ) ) ;
#42796 = EDGE_CURVE ( 'NONE', #41264, #30621, #41764, .T. ) ;
#42797 = CARTESIAN_POINT ( 'NONE',  ( -11.59517495878806947, -96.12423995607481686, -5.500000000000000000 ) ) ;
#42798 = CARTESIAN_POINT ( 'NONE',  ( 10.00000000000000000, 33.17418723428333749, -17.67226234102790272 ) ) ;
#42799 = AXIS2_PLACEMENT_3D ( 'NONE', #20930, #5760, #39546 ) ;
#42800 = ORIENTED_EDGE ( 'NONE', *, *, #113, .F. ) ;
#42801 = ADVANCED_FACE ( 'NONE', ( #11181 ), #37602, .T. ) ;
#42802 = CARTESIAN_POINT ( 'NONE',  ( 10.00000000000000000, 51.29473840253223926, 63.97538442413446091 ) ) ;
#42803 = ORIENTED_EDGE ( 'NONE', *, *, #43324, .T. ) ;
#42804 = DIRECTION ( 'NONE',  ( -1.000000000000000000, 0.000000000000000000, 0.000000000000000000 ) ) ;
#42805 = CIRCLE ( 'NONE', #24038, 16.00000000000000000 ) ;
#42806 = DIRECTION ( 'NONE',  ( 0.000000000000000000, 0.000000000000000000, 1.000000000000000000 ) ) ;
#42807 = CARTESIAN_POINT ( 'NONE',  ( 15.00000000000000000, -11.95096189432345746, -23.69967320028757030 ) ) ;
#42808 = ORIENTED_EDGE ( 'NONE', *, *, #1153, .T. ) ;
#42809 = CARTESIAN_POINT ( 'NONE',  ( 5.000000000000000000, 51.29473840253317718, -63.97538442413369353 ) ) ;
#42810 = DIRECTION ( 'NONE',  ( 1.000000000000000000, 0.000000000000000000, 0.000000000000000000 ) ) ;
#42811 = DIRECTION ( 'NONE',  ( -1.000000000000000000, 0.000000000000000000, -0.000000000000000000 ) ) ;
#42812 = EDGE_CURVE ( 'NONE', #12381, #4718, #22909, .T. ) ;
#42813 = ORIENTED_EDGE ( 'NONE', *, *, #25354, .T. ) ;
#42814 = VECTOR ( 'NONE', #27215, 1000.000000000000000 ) ;
#42815 = DIRECTION ( 'NONE',  ( -1.000000000000000000, -0.000000000000000000, 0.000000000000000000 ) ) ;
#42816 = PLANE ( 'NONE',  #37819 ) ;
#42817 = DIRECTION ( 'NONE',  ( -1.000000000000000000, -0.000000000000000000, -0.000000000000000000 ) ) ;
#42818 = CARTESIAN_POINT ( 'NONE',  ( 10.00000000000000000, 33.00180498840046539, 17.80606268964551120 ) ) ;
#42819 = EDGE_LOOP ( 'NONE', ( #9181, #11186, #46122, #32983 ) ) ;
#42820 = ORIENTED_EDGE ( 'NONE', *, *, #20169, .F. ) ;
#42821 = CIRCLE ( 'NONE', #4519, 12.49999999999999645 ) ;
#42822 = ADVANCED_FACE ( 'NONE', ( #26828 ), #3335, .T. ) ;
#42823 = DIRECTION ( 'NONE',  ( 0.9997280174009349762, -0.02332147558787671729, 0.000000000000000000 ) ) ;
#42824 = DIRECTION ( 'NONE',  ( -0.9435911131814395114, 0.3311129884571304971, 0.000000000000000000 ) ) ;
#42825 = ORIENTED_EDGE ( 'NONE', *, *, #36889, .T. ) ;
#42826 = AXIS2_PLACEMENT_3D ( 'NONE', #48255, #14732, #7380 ) ;
#42827 = EDGE_CURVE ( 'NONE', #9644, #16667, #30275, .T. ) ;
#42828 = CYLINDRICAL_SURFACE ( 'NONE', #12466, 31.99999999999998579 ) ;
#42830 = EDGE_CURVE ( 'NONE', #35835, #30318, #44026, .T. ) ;
#42829 = AXIS2_PLACEMENT_3D ( 'NONE', #42986, #38844, #20220 ) ;
#42831 = ORIENTED_EDGE ( 'NONE', *, *, #664, .T. ) ;
#42832 = VERTEX_POINT ( 'NONE', #30022 ) ;
#42833 = ORIENTED_EDGE ( 'NONE', *, *, #11344, .F. ) ;
#42834 = ADVANCED_FACE ( 'NONE', ( #37362 ), #44953, .F. ) ;
#42835 = CARTESIAN_POINT ( 'NONE',  ( 6.000000000000000000, 71.87247863392413194, 39.47590169984871267 ) ) ;
#42836 = EDGE_CURVE ( 'NONE', #30446, #4822, #22441, .T. ) ;
#42837 = ORIENTED_EDGE ( 'NONE', *, *, #40056, .F. ) ;
#42838 = DIRECTION ( 'NONE',  ( -1.000000000000000000, 0.000000000000000000, 0.000000000000000000 ) ) ;
#42839 = EDGE_CURVE ( 'NONE', #18610, #20071, #6509, .T. ) ;
#42840 = ORIENTED_EDGE ( 'NONE', *, *, #45031, .T. ) ;
#42841 = DIRECTION ( 'NONE',  ( 0.000000000000000000, 0.8910065241883656784, 0.4539904997395510788 ) ) ;
#42842 = CARTESIAN_POINT ( 'NONE',  ( 10.00000000000000000, 0.000000000000000000, 0.000000000000000000 ) ) ;
#42843 = PRESENTATION_LAYER_ASSIGNMENT (  '', '', ( #15484 ) ) ;
#42844 = CYLINDRICAL_SURFACE ( 'NONE', #25956, 31.99999999999999289 ) ;
#42845 = ORIENTED_EDGE ( 'NONE', *, *, #42494, .F. ) ;
#42846 = CYLINDRICAL_SURFACE ( 'NONE', #38414, 32.00000000000000000 ) ;
#42847 = ORIENTED_EDGE ( 'NONE', *, *, #44657, .F. ) ;
#42848 = AXIS2_PLACEMENT_3D ( 'NONE', #36626, #14850, #25608 ) ;
#42849 = CARTESIAN_POINT ( 'NONE',  ( 5.000000000000002665, 2.543863470249527303, -81.96053171279901051 ) ) ;
#42850 = FACE_OUTER_BOUND ( 'NONE', #12117, .T. ) ;
#42851 = DIRECTION ( 'NONE',  ( -1.000000000000000000, 0.000000000000000000, 0.000000000000000000 ) ) ;
#42852 = EDGE_LOOP ( 'NONE', ( #30364, #41402, #36619, #3814 ) ) ;
#42853 = ORIENTED_EDGE ( 'NONE', *, *, #41708, .T. ) ;
#42854 = LINE ( 'NONE', #1985, #35397 ) ;
#42855 = CARTESIAN_POINT ( 'NONE',  ( -17.26469406256017791, -140.1601175325492648, 5.500000000000000000 ) ) ;
#42856 = ORIENTED_EDGE ( 'NONE', *, *, #318, .T. ) ;
#42857 = ORIENTED_EDGE ( 'NONE', *, *, #8871, .T. ) ;
#42858 = DIRECTION ( 'NONE',  ( 1.000000000000000000, 0.000000000000000000, 0.000000000000000000 ) ) ;
#42859 = DIRECTION ( 'NONE',  ( -1.000000000000000000, 0.000000000000000000, 0.000000000000000000 ) ) ;
#42860 = CARTESIAN_POINT ( 'NONE',  ( -11.99999999999999645, 0.000000000000000000, 0.000000000000000000 ) ) ;
#42861 = DIRECTION ( 'NONE',  ( -1.000000000000000000, -0.000000000000000000, -0.000000000000000000 ) ) ;
#42862 = CARTESIAN_POINT ( 'NONE',  ( 0.000000000000000000, 0.000000000000000000, 0.000000000000000000 ) ) ;
#42863 = DIRECTION ( 'NONE',  ( 0.000000000000000000, 0.000000000000000000, 1.000000000000000000 ) ) ;
#42864 = CIRCLE ( 'NONE', #10001, 77.49899999999999523 ) ;
#42865 = ADVANCED_FACE ( 'NONE', ( #37116 ), #48374, .T. ) ;
#42866 = DIRECTION ( 'NONE',  ( 0.000000000000000000, 0.8910065241883688980, -0.4539904997395445840 ) ) ;
#42867 = CARTESIAN_POINT ( 'NONE',  ( 7.543218489614351263, -11.91259227951415056, -1.199999999999999956 ) ) ;
#42868 = DIRECTION ( 'NONE',  ( 0.000000000000000000, 0.5877852522924743583, -0.8090169943749466741 ) ) ;
#42869 = VECTOR ( 'NONE', #12931, 1000.000000000000000 ) ;
#42870 = CARTESIAN_POINT ( 'NONE',  ( 10.00000000000000000, 3.925862922256769583, -41.81611651403858332 ) ) ;
#42871 = DIRECTION ( 'NONE',  ( 0.000000000000000000, 0.3090169943749482839, -0.9510565162951533091 ) ) ;
#42872 = EDGE_CURVE ( 'NONE', #38126, #46920, #26103, .T. ) ;
#42874 = AXIS2_PLACEMENT_3D ( 'NONE', #46195, #12919, #3078 ) ;
#42873 = DIRECTION ( 'NONE',  ( 0.000000000000000000, 0.000000000000000000, 1.000000000000000000 ) ) ;
#42875 = DIRECTION ( 'NONE',  ( -1.000000000000000000, -0.000000000000000000, 0.000000000000000000 ) ) ;
#42876 = ORIENTED_EDGE ( 'NONE', *, *, #10984, .T. ) ;
#42877 = ORIENTED_EDGE ( 'NONE', *, *, #47304, .T. ) ;
#42878 = EDGE_CURVE ( 'NONE', #747, #6258, #1611, .T. ) ;
#42879 = FACE_OUTER_BOUND ( 'NONE', #16345, .T. ) ;
#42880 = CARTESIAN_POINT ( 'NONE',  ( 11.99999999999999822, 0.000000000000000000, 0.000000000000000000 ) ) ;
#42881 = PRESENTATION_LAYER_ASSIGNMENT (  '', '', ( #47547 ) ) ;
#42882 = PLANE ( 'NONE',  #46394 ) ;
#42883 = ORIENTED_EDGE ( 'NONE', *, *, #5577, .F. ) ;
#42884 = AXIS2_PLACEMENT_3D ( 'NONE', #44845, #41195, #7648 ) ;
#42885 = EDGE_CURVE ( 'NONE', #35650, #46082, #233, .T. ) ;
#42886 = DIRECTION ( 'NONE',  ( 0.000000000000000000, -0.9945218953682730678, -0.1045284632676570929 ) ) ;
#42887 = EDGE_LOOP ( 'NONE', ( #7842, #45961, #28208, #27406 ) ) ;
#42888 = CARTESIAN_POINT ( 'NONE',  ( 11.99999999999999822, -2.946379043145784582, -75.11764819372150725 ) ) ;
#42889 = ORIENTED_EDGE ( 'NONE', *, *, #11104, .T. ) ;
#42891 = EDGE_CURVE ( 'NONE', #46797, #13463, #13539, .T. ) ;
#42890 = DIRECTION ( 'NONE',  ( -1.000000000000000000, 0.000000000000000000, -0.000000000000000000 ) ) ;
#42892 = CYLINDRICAL_SURFACE ( 'NONE', #17489, 37.49900000000000233 ) ;
#42893 = EDGE_CURVE ( 'NONE', #40712, #33189, #9192, .T. ) ;
#42894 = CARTESIAN_POINT ( 'NONE',  ( 15.00000000000000000, 6.762365576493647445, 25.66652317338391498 ) ) ;
#42895 = ORIENTED_EDGE ( 'NONE', *, *, #46743, .T. ) ;
#42896 = LINE ( 'NONE', #8864, #5906 ) ;
#42897 = ORIENTED_EDGE ( 'NONE', *, *, #22490, .T. ) ;
#42898 = AXIS2_PLACEMENT_3D ( 'NONE', #17543, #17296, #2602 ) ;
#42899 = EDGE_CURVE ( 'NONE', #29274, #828, #4173, .T. ) ;
#42900 = VECTOR ( 'NONE', #29055, 1000.000000000000000 ) ;
#42901 = DIRECTION ( 'NONE',  ( 1.000000000000000000, 0.000000000000000000, 0.000000000000000000 ) ) ;
#42902 = ORIENTED_EDGE ( 'NONE', *, *, #23600, .T. ) ;
#42903 = DIRECTION ( 'NONE',  ( -1.000000000000000000, 0.000000000000000000, 0.000000000000000000 ) ) ;
#42904 = LINE ( 'NONE', #42667, #45827 ) ;
#42905 = CARTESIAN_POINT ( 'NONE',  ( 0.000000000000000000, 21.53537804866081373, 30.80686688397018358 ) ) ;
#42906 = CARTESIAN_POINT ( 'NONE',  ( 10.00000000000000000, 0.000000000000000000, 0.000000000000000000 ) ) ;
#42907 = ORIENTED_EDGE ( 'NONE', *, *, #42872, .T. ) ;
#42908 = LINE ( 'NONE', #20368, #38134 ) ;
#42909 = ORIENTED_EDGE ( 'NONE', *, *, #12830, .T. ) ;
#42910 = ORIENTED_EDGE ( 'NONE', *, *, #34640, .T. ) ;
#42911 = DIRECTION ( 'NONE',  ( 0.000000000000000000, 0.000000000000000000, 1.000000000000000000 ) ) ;
#42912 = EDGE_LOOP ( 'NONE', ( #10523, #16824, #11404, #27941 ) ) ;
#42913 = FACE_OUTER_BOUND ( 'NONE', #8194, .T. ) ;
#42914 = DIRECTION ( 'NONE',  ( -1.000000000000000000, 0.000000000000000000, 0.000000000000000000 ) ) ;
#42915 = CARTESIAN_POINT ( 'NONE',  ( 0.000000000000000000, -1.278221433540502217, 26.51162292216071847 ) ) ;
#42916 = ORIENTED_EDGE ( 'NONE', *, *, #17712, .F. ) ;
#42917 = DIRECTION ( 'NONE',  ( -1.000000000000000000, 0.000000000000000000, -0.000000000000000000 ) ) ;
#42918 = PRODUCT ( 'small gear_ISO - Spur gear 2M 40T 20PA 10FW ---S40A75H50L20.0N', 'small gear_ISO - Spur gear 2M 40T 20PA 10FW ---S40A75H50L20.0N', '', ( #27472 ) ) ;
#42919 = LINE ( 'NONE', #2051, #27591 ) ;
#42920 = DIRECTION ( 'NONE',  ( 1.000000000000000000, 0.000000000000000000, 0.000000000000000000 ) ) ;
#42921 = STYLED_ITEM ( 'NONE', ( #18598 ), #1820 ) ;
#42922 = CARTESIAN_POINT ( 'NONE',  ( 10.00000000000000000, -22.64427369931148348, -30.00120703465229965 ) ) ;
#42923 = DIRECTION ( 'NONE',  ( 1.000000000000000000, 0.000000000000000000, 0.000000000000000000 ) ) ;
#42924 = LINE ( 'NONE', #35323, #39509 ) ;
#42925 = CARTESIAN_POINT ( 'NONE',  ( 0.000000000000000000, 0.000000000000000000, 0.000000000000000000 ) ) ;
#42926 = DIRECTION ( 'NONE',  ( 1.000000000000000000, -0.000000000000000000, -0.000000000000000000 ) ) ;
#42927 = FACE_OUTER_BOUND ( 'NONE', #46511, .T. ) ;
#42928 = CARTESIAN_POINT ( 'NONE',  ( 11.99999999999999822, 0.000000000000000000, 0.000000000000000000 ) ) ;
#42929 = ORIENTED_EDGE ( 'NONE', *, *, #41343, .F. ) ;
#42930 = CARTESIAN_POINT ( 'NONE',  ( 10.00000000000000000, 0.000000000000000000, 0.000000000000000000 ) ) ;
#42931 = AXIS2_PLACEMENT_3D ( 'NONE', #32526, #44264, #10740 ) ;
#42932 = ORIENTED_EDGE ( 'NONE', *, *, #16150, .F. ) ;
#42933 = CARTESIAN_POINT ( 'NONE',  ( 0.000000000000000000, 0.000000000000000000, 0.000000000000000000 ) ) ;
#42934 = EDGE_CURVE ( 'NONE', #36833, #7751, #38552, .T. ) ;
#42935 = AXIS2_PLACEMENT_3D ( 'NONE', #26388, #45227, #3863 ) ;
#42936 = AXIS2_PLACEMENT_3D ( 'NONE', #41566, #34206, #444 ) ;
#42937 = LINE ( 'NONE', #28238, #37758 ) ;
#42938 = ORIENTED_EDGE ( 'NONE', *, *, #18304, .T. ) ;
#42939 = CARTESIAN_POINT ( 'NONE',  ( 11.99999999999999822, -2.946379043145784582, -75.11764819372150725 ) ) ;
#42940 = ORIENTED_EDGE ( 'NONE', *, *, #17459, .T. ) ;
#42942 = EDGE_CURVE ( 'NONE', #27374, #28899, #23158, .T. ) ;
#42941 = EDGE_LOOP ( 'NONE', ( #17887, #5637, #2179, #625 ) ) ;
#42943 = ORIENTED_EDGE ( 'NONE', *, *, #45578, .F. ) ;
#42944 = EDGE_CURVE ( 'NONE', #26170, #3496, #1832, .T. ) ;
#42945 = EDGE_CURVE ( 'NONE', #34021, #1544, #8948, .T. ) ;
#42946 =( GEOMETRIC_REPRESENTATION_CONTEXT ( 3 ) GLOBAL_UNCERTAINTY_ASSIGNED_CONTEXT ( ( #26677 ) ) GLOBAL_UNIT_ASSIGNED_CONTEXT ( ( #2630, #36884, #3611 ) ) REPRESENTATION_CONTEXT ( 'NONE', 'WORKASPACE' ) );
#42947 = CARTESIAN_POINT ( 'NONE',  ( 11.99999999999999822, 16.65972982744933972, 80.28980883073764119 ) ) ;
#42948 = EDGE_CURVE ( 'NONE', #22205, #38319, #33051, .T. ) ;
#42949 = DIRECTION ( 'NONE',  ( -0.9966891607226786576, -0.08130631524009861166, 0.000000000000000000 ) ) ;
#42951 = VERTEX_POINT ( 'NONE', #20435 ) ;
#42950 = DIRECTION ( 'NONE',  ( -1.000000000000000000, 0.000000000000000000, 0.000000000000000000 ) ) ;
#42952 = EDGE_LOOP ( 'NONE', ( #40322, #895, #23025, #4888 ) ) ;
#42953 = DIRECTION ( 'NONE',  ( -0.000000000000000000, -0.000000000000000000, -1.000000000000000000 ) ) ;
#42954 = EDGE_CURVE ( 'NONE', #36873, #14595, #8846, .T. ) ;
#42955 = ORIENTED_EDGE ( 'NONE', *, *, #32793, .T. ) ;
#42956 = EDGE_LOOP ( 'NONE', ( #16293, #12102, #4201, #5704 ) ) ;
#42957 = FACE_OUTER_BOUND ( 'NONE', #39987, .T. ) ;
#42958 = CARTESIAN_POINT ( 'NONE',  ( 0.000000000000000000, 0.000000000000000000, 0.000000000000000000 ) ) ;
#42959 = CYLINDRICAL_SURFACE ( 'NONE', #37641, 77.49899999999999523 ) ;
#42960 = CIRCLE ( 'NONE', #48397, 77.49899999999999523 ) ;
#42961 = ORIENTED_EDGE ( 'NONE', *, *, #31945, .T. ) ;
#42962 = ORIENTED_EDGE ( 'NONE', *, *, #9724, .F. ) ;
#42963 = CIRCLE ( 'NONE', #39857, 77.49900000000000944 ) ;
#42964 = LINE ( 'NONE', #12866, #29444 ) ;
#42965 = ORIENTED_EDGE ( 'NONE', *, *, #20166, .T. ) ;
#42966 = FACE_BOUND ( 'NONE', #27547, .T. ) ;
#42967 = CIRCLE ( 'NONE', #14061, 31.99999999999999289 ) ;
#42968 = EDGE_CURVE ( 'NONE', #5995, #19357, #36198, .T. ) ;
#42969 = CARTESIAN_POINT ( 'NONE',  ( 0.000000000000000000, 54.21277698773752007, -55.38113227695726692 ) ) ;
#42970 = LINE ( 'NONE', #31732, #33822 ) ;
#42971 = PLANE ( 'NONE',  #20622 ) ;
#42972 = CYLINDRICAL_SURFACE ( 'NONE', #11754, 16.00000000000000000 ) ;
#42973 = DIRECTION ( 'NONE',  ( -1.000000000000000000, 0.000000000000000000, 0.000000000000000000 ) ) ;
#42974 = DIRECTION ( 'NONE',  ( -1.000000000000000000, 0.000000000000000000, 0.000000000000000000 ) ) ;
#42975 = DIRECTION ( 'NONE',  ( -1.000000000000000000, -0.000000000000000000, -0.000000000000000000 ) ) ;
#42976 = CARTESIAN_POINT ( 'NONE',  ( 10.00000000000000000, 68.55367621811204515, -44.99326035065983120 ) ) ;
#42977 = CARTESIAN_POINT ( 'NONE',  ( 11.99999999999999822, 77.19088730480532945, -6.903761155836932062 ) ) ;
#42978 = DIRECTION ( 'NONE',  ( 0.000000000000000000, 0.000000000000000000, 1.000000000000000000 ) ) ;
#42979 = ORIENTED_EDGE ( 'NONE', *, *, #2303, .T. ) ;
#42980 = AXIS2_PLACEMENT_3D ( 'NONE', #12326, #8624, #42415 ) ;
#42981 = CARTESIAN_POINT ( 'NONE',  ( 11.99999999999999822, -41.76937507738745836, -62.50329211542482710 ) ) ;
#42982 = LINE ( 'NONE', #42249, #35286 ) ;
#42983 = DIRECTION ( 'NONE',  ( 0.000000000000000000, 0.000000000000000000, 1.000000000000000000 ) ) ;
#42984 = ADVANCED_FACE ( 'NONE', ( #46161 ), #38829, .F. ) ;
#42985 = CARTESIAN_POINT ( 'NONE',  ( 10.00000000000000000, 12.26510123303259725, 35.53030884539089840 ) ) ;
#42986 = CARTESIAN_POINT ( 'NONE',  ( 10.00000000000000000, 5.202137450156389953, 37.22597642581160216 ) ) ;
#42987 = EDGE_CURVE ( 'NONE', #19565, #16881, #18199, .T. ) ;
#42988 = DIRECTION ( 'NONE',  ( -1.000000000000000000, 0.000000000000000000, 0.000000000000000000 ) ) ;
#42989 = CARTESIAN_POINT ( 'NONE',  ( 25.38712131070745315, -112.4010479962415872, -2.500000000000000000 ) ) ;
#42990 = ORIENTED_EDGE ( 'NONE', *, *, #17024, .T. ) ;
#42991 = DIRECTION ( 'NONE',  ( -0.000000000000000000, -0.6691306063588570163, 0.7431448254773953543 ) ) ;
#42992 = EDGE_CURVE ( 'NONE', #41344, #19426, #866, .T. ) ;
#42993 = ORIENTED_EDGE ( 'NONE', *, *, #33686, .F. ) ;
#42994 = EDGE_CURVE ( 'NONE', #46829, #19329, #35126, .T. ) ;
#42995 = CYLINDRICAL_SURFACE ( 'NONE', #42409, 82.00000000000000000 ) ;
#42996 = EDGE_LOOP ( 'NONE', ( #46499, #35003, #29257, #24645 ) ) ;
#42997 = ORIENTED_EDGE ( 'NONE', *, *, #34867, .T. ) ;
#42998 = AXIS2_PLACEMENT_3D ( 'NONE', #4778, #19679, #12371 ) ;
#42999 = VERTEX_POINT ( 'NONE', #4796 ) ;
#43000 = AXIS2_PLACEMENT_3D ( 'NONE', #12002, #15906, #18837 ) ;
#43001 = CARTESIAN_POINT ( 'NONE',  ( -0.2999999999999964362, 0.000000000000000000, 0.000000000000000000 ) ) ;
#43002 = ORIENTED_EDGE ( 'NONE', *, *, #44583, .T. ) ;
#43003 = CIRCLE ( 'NONE', #39888, 37.49900000000000233 ) ;
#43004 = EDGE_CURVE ( 'NONE', #994, #45324, #4219, .T. ) ;
#43005 = EDGE_CURVE ( 'NONE', #1874, #14593, #42012, .T. ) ;
#43006 = ORIENTED_EDGE ( 'NONE', *, *, #26562, .T. ) ;
#43007 = VECTOR ( 'NONE', #47522, 1000.000000000000000 ) ;
#43008 = CARTESIAN_POINT ( 'NONE',  ( -11.59999999999999787, 0.000000000000000000, 40.80000000000001847 ) ) ;
#43010 = EDGE_LOOP ( 'NONE', ( #32137, #20047, #20807, #898 ) ) ;
#43009 = CARTESIAN_POINT ( 'NONE',  ( 10.00000000000000000, -12.42422080174663712, 35.38097989696507994 ) ) ;
#43011 = ORIENTED_EDGE ( 'NONE', *, *, #30065, .T. ) ;
#43012 = ORIENTED_EDGE ( 'NONE', *, *, #31637, .T. ) ;
#43013 = LINE ( 'NONE', #1648, #24098 ) ;
#43014 = ADVANCED_FACE ( 'NONE', ( #45924 ), #8692, .T. ) ;
#43016 = EDGE_LOOP ( 'NONE', ( #2697, #23363, #42825, #804 ) ) ;
#43015 = DIRECTION ( 'NONE',  ( 0.000000000000000000, 0.8090169943749432324, 0.5877852522924789103 ) ) ;
#43017 = DIRECTION ( 'NONE',  ( 0.9227826878668550226, 0.3853207896976523772, -0.000000000000000000 ) ) ;
#43018 = VERTEX_POINT ( 'NONE', #17012 ) ;
#43019 = VERTEX_POINT ( 'NONE', #13350 ) ;
#43020 = DIRECTION ( 'NONE',  ( 0.000000000000000000, 0.3826834323650904479, -0.9238795325112865164 ) ) ;
#43021 = ORIENTED_EDGE ( 'NONE', *, *, #12594, .T. ) ;
#43022 = CARTESIAN_POINT ( 'NONE',  ( 10.00000000000000000, -5.202137450156655518, 37.22597642581156663 ) ) ;
#43023 = CARTESIAN_POINT ( 'NONE',  ( 10.00000000000000000, 0.000000000000000000, 2.500000000000000000 ) ) ;
#43024 = CARTESIAN_POINT ( 'NONE',  ( 0.000000000000000000, 71.87247863392471459, -39.47590169984771080 ) ) ;
#43025 = CARTESIAN_POINT ( 'NONE',  ( 50.00005079999999680, 1.530808498934191521E-15, -12.50000000000000000 ) ) ;
#43026 = DIRECTION ( 'NONE',  ( -1.000000000000000000, 0.000000000000000000, 0.000000000000000000 ) ) ;
#43027 = VERTEX_POINT ( 'NONE', #43685 ) ;
#43028 = ORIENTED_EDGE ( 'NONE', *, *, #14053, .F. ) ;
#43029 = CARTESIAN_POINT ( 'NONE',  ( 0.000000000000000000, 77.16300072079660310, 27.74655509720696500 ) ) ;
#43030 = VECTOR ( 'NONE', #623, 1000.000000000000000 ) ;
#43031 = DIRECTION ( 'NONE',  ( 0.000000000000000000, -0.8090169943749402348, -0.5877852522924830181 ) ) ;
#43032 = ORIENTED_EDGE ( 'NONE', *, *, #44548, .T. ) ;
#43033 = AXIS2_PLACEMENT_3D ( 'NONE', #27358, #34434, #30796 ) ;
#43034 = DIRECTION ( 'NONE',  ( 0.000000000000000000, 0.000000000000000000, 1.000000000000000000 ) ) ;
#43035 = ORIENTED_EDGE ( 'NONE', *, *, #15878, .F. ) ;
#43036 = AXIS2_PLACEMENT_3D ( 'NONE', #9057, #1713, #12981 ) ;
#43037 = CARTESIAN_POINT ( 'NONE',  ( 10.00000000000000000, 30.00120703465236716, -22.64427369931138756 ) ) ;
#43038 = PLANE ( 'NONE',  #44297 ) ;
#43039 = DIRECTION ( 'NONE',  ( 1.000000000000000000, 0.000000000000000000, 0.000000000000000000 ) ) ;
#43040 = CARTESIAN_POINT ( 'NONE',  ( 11.99999999999999822, 0.000000000000000000, 0.000000000000000000 ) ) ;
#43041 = VECTOR ( 'NONE', #19705, 999.9999999999998863 ) ;
#43042 = AXIS2_PLACEMENT_3D ( 'NONE', #29427, #17183, #25499 ) ;
#43043 = DIRECTION ( 'NONE',  ( 0.000000000000000000, 0.9969173337331281859, -0.07845909572784180719 ) ) ;
#43044 = ORIENTED_EDGE ( 'NONE', *, *, #33335, .T. ) ;
#43045 = ADVANCED_FACE ( 'NONE', ( #28269 ), #9665, .T. ) ;
#43046 = CARTESIAN_POINT ( 'NONE',  ( 15.00000000000000000, 16.83928648764945635, 16.46020748918027010 ) ) ;
#43047 = DIRECTION ( 'NONE',  ( -1.000000000000000000, -0.000000000000000000, 0.000000000000000000 ) ) ;
#43048 = DIRECTION ( 'NONE',  ( 0.000000000000000000, 0.000000000000000000, 1.000000000000000000 ) ) ;
#43049 = EDGE_CURVE ( 'NONE', #5583, #1751, #25074, .T. ) ;
#43050 = FACE_OUTER_BOUND ( 'NONE', #46564, .T. ) ;
#43051 = EDGE_CURVE ( 'NONE', #25561, #29936, #40020, .T. ) ;
#43052 = EDGE_LOOP ( 'NONE', ( #691, #17418, #21002, #6110 ) ) ;
#43053 = ORIENTED_EDGE ( 'NONE', *, *, #45919, .F. ) ;
#43054 = CARTESIAN_POINT ( 'NONE',  ( 0.000000000000000000, -44.88180994100421373, 63.18004540533011948 ) ) ;
#43055 = CARTESIAN_POINT ( 'NONE',  ( 10.00000000000000000, 2.956366410620650420, 75.11725578898469280 ) ) ;
#43056 = ORIENTED_EDGE ( 'NONE', *, *, #11218, .F. ) ;
#43057 = EDGE_CURVE ( 'NONE', #36518, #44612, #36339, .T. ) ;
#43058 = ADVANCED_FACE ( 'NONE', ( #28760 ), #32197, .T. ) ;
#43059 = ORIENTED_EDGE ( 'NONE', *, *, #27905, .F. ) ;
#43060 = VECTOR ( 'NONE', #18009, 999.9999999999998863 ) ;
#43061 = EDGE_CURVE ( 'NONE', #37949, #24526, #44065, .T. ) ;
#43062 = CARTESIAN_POINT ( 'NONE',  ( 0.000000000000000000, -41.91543099594819921, 2.663952781846001816 ) ) ;
#43063 = CIRCLE ( 'NONE', #7873, 37.49900000000001654 ) ;
#43065 = CIRCLE ( 'NONE', #46976, 16.00000000000000000 ) ;
#43064 = DIRECTION ( 'NONE',  ( 0.000000000000000000, 0.000000000000000000, -1.000000000000000000 ) ) ;
#43066 = ORIENTED_EDGE ( 'NONE', *, *, #23097, .F. ) ;
#43067 = ORIENTED_EDGE ( 'NONE', *, *, #20665, .F. ) ;
#43068 = ORIENTED_EDGE ( 'NONE', *, *, #43443, .F. ) ;
#43069 = CIRCLE ( 'NONE', #39928, 10.00000000000000178 ) ;
#43070 = AXIS2_PLACEMENT_3D ( 'NONE', #12752, #27685, #15943 ) ;
#43071 = EDGE_CURVE ( 'NONE', #43945, #29887, #28418, .T. ) ;
#43072 = CARTESIAN_POINT ( 'NONE',  ( 15.00000000000000000, -22.67460108101774452, 6.353146135318220367 ) ) ;
#43073 = AXIS2_PLACEMENT_3D ( 'NONE', #19514, #30086, #34454 ) ;
#43074 = VERTEX_POINT ( 'NONE', #14066 ) ;
#43075 = CARTESIAN_POINT ( 'NONE',  ( 0.000000000000000000, 81.50828551894227303, 8.966570791700986476 ) ) ;
#43076 = ORIENTED_EDGE ( 'NONE', *, *, #8611, .F. ) ;
#43077 = CARTESIAN_POINT ( 'NONE',  ( 0.000000000000000000, 0.000000000000000000, 0.000000000000000000 ) ) ;
#43078 = CARTESIAN_POINT ( 'NONE',  ( 3.250000000000000444, -13.95926121303099343, -1.199999999999999956 ) ) ;
#43079 = DIRECTION ( 'NONE',  ( 0.000000000000000000, 0.000000000000000000, 1.000000000000000000 ) ) ;
#43080 = ORIENTED_EDGE ( 'NONE', *, *, #39531, .F. ) ;
#43081 = DIRECTION ( 'NONE',  ( 0.9997280174009349762, -0.02332147558787674158, 0.000000000000000000 ) ) ;
#43082 = ORIENTED_EDGE ( 'NONE', *, *, #41549, .F. ) ;
#43083 = DIRECTION ( 'NONE',  ( -1.000000000000000000, -0.000000000000000000, -0.000000000000000000 ) ) ;
#43084 = CARTESIAN_POINT ( 'NONE',  ( 15.00000000000000000, -19.89357724624986545, 12.59942793731086219 ) ) ;
#43085 = CARTESIAN_POINT ( 'NONE',  ( 5.999999999999999112, -56.15606465355000410, 59.75363087400056372 ) ) ;
#43086 = ORIENTED_EDGE ( 'NONE', *, *, #43676, .F. ) ;
#43087 = ORIENTED_EDGE ( 'NONE', *, *, #45210, .T. ) ;
#43088 = DIRECTION ( 'NONE',  ( -1.000000000000000000, 0.000000000000000000, -0.000000000000000000 ) ) ;
#43089 = DIRECTION ( 'NONE',  ( 0.000000000000000000, 0.000000000000000000, 1.000000000000000000 ) ) ;
#43090 = VERTEX_POINT ( 'NONE', #28987 ) ;
#43091 = CARTESIAN_POINT ( 'NONE',  ( 10.00000000000000000, 0.000000000000000000, 0.000000000000000000 ) ) ;
#43092 = CARTESIAN_POINT ( 'NONE',  ( 12.50000000000000000, -107.5000000000000000, 2.500000000000000000 ) ) ;
#43093 = FACE_OUTER_BOUND ( 'NONE', #29891, .T. ) ;
#43094 = DIRECTION ( 'NONE',  ( -0.000000000000000000, -0.000000000000000000, -1.000000000000000000 ) ) ;
#43095 = FACE_OUTER_BOUND ( 'NONE', #35394, .T. ) ;
#43096 = CIRCLE ( 'NONE', #36827, 82.00000000000000000 ) ;
#43097 = DIRECTION ( 'NONE',  ( -1.000000000000000000, -0.000000000000000000, -0.000000000000000000 ) ) ;
#43098 = DIRECTION ( 'NONE',  ( 1.000000000000000000, 0.000000000000000000, 0.000000000000000000 ) ) ;
#43099 = CIRCLE ( 'NONE', #36063, 42.00000000000000000 ) ;
#43100 = AXIS2_PLACEMENT_3D ( 'NONE', #20975, #35897, #28803 ) ;
#43101 = EDGE_CURVE ( 'NONE', #48430, #34442, #1878, .T. ) ;
#43102 = PLANE ( 'NONE',  #47898 ) ;
#43103 = DIRECTION ( 'NONE',  ( 0.000000000000000000, 0.8660254037844421493, 0.4999999999999938938 ) ) ;
#43104 = ADVANCED_FACE ( 'NONE', ( #40271 ), #36577, .F. ) ;
#43105 = CARTESIAN_POINT ( 'NONE',  ( 0.000000000000000000, -3.948201729842037544, -23.21447184625298021 ) ) ;
#43106 = CYLINDRICAL_SURFACE ( 'NONE', #10769, 77.49899999999999523 ) ;
#43107 = ADVANCED_FACE ( 'NONE', ( #32898 ), #14308, .F. ) ;
#43108 = AXIS2_PLACEMENT_3D ( 'NONE', #32767, #2669, #17127 ) ;
#43109 = ORIENTED_EDGE ( 'NONE', *, *, #45225, .F. ) ;
#43110 = ORIENTED_EDGE ( 'NONE', *, *, #24973, .T. ) ;
#43111 = EDGE_CURVE ( 'NONE', #31962, #23138, #6250, .T. ) ;
#43112 = CARTESIAN_POINT ( 'NONE',  ( -35.50000000000000711, -120.0000000000000000, -2.500000000000000000 ) ) ;
#43113 = ADVANCED_FACE ( 'NONE', ( #5769 ), #43461, .T. ) ;
#43114 = DIRECTION ( 'NONE',  ( 0.000000000000000000, 0.000000000000000000, 1.000000000000000000 ) ) ;
#43115 = AXIS2_PLACEMENT_3D ( 'NONE', #9776, #42601, #27666 ) ;
#43116 = FACE_OUTER_BOUND ( 'NONE', #12009, .T. ) ;
#43117 = ORIENTED_EDGE ( 'NONE', *, *, #160, .T. ) ;
#43118 = EDGE_CURVE ( 'NONE', #4884, #39718, #2098, .T. ) ;
#43119 = ORIENTED_EDGE ( 'NONE', *, *, #34080, .F. ) ;
#43120 = ORIENTED_EDGE ( 'NONE', *, *, #45379, .F. ) ;
#43121 = EDGE_CURVE ( 'NONE', #30853, #21451, #32340, .T. ) ;
#43122 = CARTESIAN_POINT ( 'NONE',  ( 10.00000000000000000, -41.81611651403859042, -3.925862922256606602 ) ) ;
#43123 = ORIENTED_EDGE ( 'NONE', *, *, #36779, .F. ) ;
#43124 = FACE_OUTER_BOUND ( 'NONE', #42714, .T. ) ;
#43125 = ORIENTED_EDGE ( 'NONE', *, *, #9402, .F. ) ;
#43126 = DIRECTION ( 'NONE',  ( 0.000000000000000000, 0.000000000000000000, -1.000000000000000000 ) ) ;
#43127 = AXIS2_PLACEMENT_3D ( 'NONE', #30888, #45815, #6800 ) ;
#43128 = ADVANCED_FACE ( 'NONE', ( #36096 ), #9917, .F. ) ;
#43129 = CARTESIAN_POINT ( 'NONE',  ( 10.00000000000000000, -41.76937507738745836, -62.50329211542482710 ) ) ;
#43130 = VECTOR ( 'NONE', #33383, 1000.000000000000000 ) ;
#43131 = DIRECTION ( 'NONE',  ( 1.000000000000000000, 0.000000000000000000, -0.000000000000000000 ) ) ;
#43132 = ORIENTED_EDGE ( 'NONE', *, *, #34655, .T. ) ;
#43133 = DIRECTION ( 'NONE',  ( 0.000000000000000000, 0.000000000000000000, 1.000000000000000000 ) ) ;
#43134 = AXIS2_PLACEMENT_3D ( 'NONE', #1539, #16461, #27733 ) ;
#43135 = ORIENTED_EDGE ( 'NONE', *, *, #17548, .T. ) ;
#43136 = ORIENTED_EDGE ( 'NONE', *, *, #10552, .F. ) ;
#43137 = CYLINDRICAL_SURFACE ( 'NONE', #31446, 77.49899999999999523 ) ;
#43138 = VERTEX_POINT ( 'NONE', #17488 ) ;
#43139 = AXIS2_PLACEMENT_3D ( 'NONE', #41059, #15100, #11185 ) ;
#43140 = LINE ( 'NONE', #21584, #21427 ) ;
#43141 = CARTESIAN_POINT ( 'NONE',  ( 0.000000000000000000, 81.90746397400393164, -3.894527615416986333 ) ) ;
#43142 = EDGE_CURVE ( 'NONE', #45887, #45280, #44648, .T. ) ;
#43143 = DIRECTION ( 'NONE',  ( -1.000000000000000000, 0.000000000000000000, 0.000000000000000000 ) ) ;
#43144 = CARTESIAN_POINT ( 'NONE',  ( 10.00000000000000000, 10.30890764327382847, 81.34940948281339956 ) ) ;
#43145 = ORIENTED_EDGE ( 'NONE', *, *, #17987, .T. ) ;
#43146 = DIRECTION ( 'NONE',  ( -1.000000000000000000, 0.000000000000000000, 0.000000000000000000 ) ) ;
#43147 = ORIENTED_EDGE ( 'NONE', *, *, #33705, .T. ) ;
#43148 = CYLINDRICAL_SURFACE ( 'NONE', #33285, 31.99999999999999289 ) ;
#43149 = ORIENTED_EDGE ( 'NONE', *, *, #27640, .F. ) ;
#43150 = VECTOR ( 'NONE', #11710, 1000.000000000000000 ) ;
#43151 = DIRECTION ( 'NONE',  ( 0.000000000000000000, -0.5224985647159381408, -0.8526401643540988395 ) ) ;
#43152 = CARTESIAN_POINT ( 'NONE',  ( 5.000000000000000000, -50.23322058963393744, 64.81221759200325039 ) ) ;
#43153 = CARTESIAN_POINT ( 'NONE',  ( -10.90473778262209414, 0.000000000000000000, 0.000000000000000000 ) ) ;
#43154 = ORIENTED_EDGE ( 'NONE', *, *, #35601, .F. ) ;
#43155 = CARTESIAN_POINT ( 'NONE',  ( -15.44521549751111422, -137.7748507232956001, 5.500000000000000000 ) ) ;
#43156 = CARTESIAN_POINT ( 'NONE',  ( 15.00000000000000000, -26.23277895567251505, -4.042438405569750870 ) ) ;
#43157 = FACE_OUTER_BOUND ( 'NONE', #31201, .T. ) ;
#43158 = DIRECTION ( 'NONE',  ( 0.000000000000000000, 0.000000000000000000, 1.000000000000000000 ) ) ;
#43159 = ADVANCED_FACE ( 'NONE', ( #22614 ), #4022, .T. ) ;
#43160 = DIRECTION ( 'NONE',  ( 0.000000000000000000, 0.000000000000000000, 1.000000000000000000 ) ) ;
#43161 = DIRECTION ( 'NONE',  ( -1.000000000000000000, -0.000000000000000000, 0.000000000000000000 ) ) ;
#43162 = SURFACE_STYLE_FILL_AREA ( #46604 ) ;
#43163 = FACE_OUTER_BOUND ( 'NONE', #19432, .T. ) ;
#43164 = CARTESIAN_POINT ( 'NONE',  ( 10.00000000000000000, 36.72794159290241822, 65.59268652807223532 ) ) ;
#43165 = EDGE_CURVE ( 'NONE', #26395, #18356, #30768, .T. ) ;
#43166 = DIRECTION ( 'NONE',  ( -1.000000000000000000, -0.000000000000000000, 0.000000000000000000 ) ) ;
#43167 = CARTESIAN_POINT ( 'NONE',  ( 0.000000000000000000, 0.000000000000000000, 0.000000000000000000 ) ) ;
#43168 = ADVANCED_FACE ( 'NONE', ( #11607 ), #10648, .F. ) ;
#43169 = AXIS2_PLACEMENT_3D ( 'NONE', #48327, #30459, #38050 ) ;
#43170 = CARTESIAN_POINT ( 'NONE',  ( 10.00000000000000000, -8.840884882375609877, 74.65374052328647281 ) ) ;
#43171 = ORIENTED_EDGE ( 'NONE', *, *, #27014, .F. ) ;
#43172 = ADVANCED_FACE ( 'NONE', ( #18461 ), #48317, .T. ) ;
#43173 = CYLINDRICAL_SURFACE ( 'NONE', #43304, 82.00000000000000000 ) ;
#43174 = DIRECTION ( 'NONE',  ( -1.000000000000000000, -0.000000000000000000, -0.000000000000000000 ) ) ;
#43175 = AXIS2_PLACEMENT_3D ( 'NONE', #6732, #25559, #44415 ) ;
#43176 = VERTEX_POINT ( 'NONE', #40735 ) ;
#43177 = CIRCLE ( 'NONE', #951, 16.00000000000000000 ) ;
#43178 = DIRECTION ( 'NONE',  ( 0.000000000000000000, 0.000000000000000000, 1.000000000000000000 ) ) ;
#43179 = ORIENTED_EDGE ( 'NONE', *, *, #6528, .T. ) ;
#43180 = ORIENTED_EDGE ( 'NONE', *, *, #36586, .T. ) ;
#43181 = AXIS2_PLACEMENT_3D ( 'NONE', #17313, #16605, #12955 ) ;
#43182 = FACE_OUTER_BOUND ( 'NONE', #30200, .T. ) ;
#43183 = ORIENTED_EDGE ( 'NONE', *, *, #3002, .F. ) ;
#43184 = CARTESIAN_POINT ( 'NONE',  ( 0.000000000000000000, -18.89407956138310496, 75.16055320797023853 ) ) ;
#43185 = CARTESIAN_POINT ( 'NONE',  ( 11.99999999999999822, -49.70050353004932475, 59.46389618801947563 ) ) ;
#43186 = AXIS2_PLACEMENT_3D ( 'NONE', #7801, #45744, #12223 ) ;
#43187 = ORIENTED_EDGE ( 'NONE', *, *, #23640, .T. ) ;
#43188 = DIRECTION ( 'NONE',  ( 0.000000000000000000, 0.000000000000000000, 1.000000000000000000 ) ) ;
#43189 = ORIENTED_EDGE ( 'NONE', *, *, #30786, .F. ) ;
#43190 = DIRECTION ( 'NONE',  ( -1.000000000000000000, 0.000000000000000000, -0.000000000000000000 ) ) ;
#43191 = DIRECTION ( 'NONE',  ( -0.9580045777625456616, -0.2867529058022021404, 0.000000000000000000 ) ) ;
#43192 = DIRECTION ( 'NONE',  ( 0.000000000000000000, 0.000000000000000000, 1.000000000000000000 ) ) ;
#43193 = VECTOR ( 'NONE', #40223, 1000.000000000000114 ) ;
#43194 = ORIENTED_EDGE ( 'NONE', *, *, #19993, .F. ) ;
#43195 = AXIS2_PLACEMENT_3D ( 'NONE', #17671, #23879, #36273 ) ;
#43196 = ORIENTED_EDGE ( 'NONE', *, *, #32178, .F. ) ;
#43197 = ORIENTED_EDGE ( 'NONE', *, *, #38911, .T. ) ;
#43198 = DIRECTION ( 'NONE',  ( 0.7533909544171997208, 0.6575728627325955200, 0.000000000000000000 ) ) ;
#43199 = ORIENTED_EDGE ( 'NONE', *, *, #23038, .T. ) ;
#43200 = AXIS2_PLACEMENT_3D ( 'NONE', #34699, #38884, #35184 ) ;
#43201 = DIRECTION ( 'NONE',  ( -1.000000000000000000, 0.000000000000000000, 0.000000000000000000 ) ) ;
#43202 = CARTESIAN_POINT ( 'NONE',  ( 0.000000000000000000, -71.91182617369207719, 28.89263327155721228 ) ) ;
#43203 = DIRECTION ( 'NONE',  ( -1.000000000000000000, 0.000000000000000000, 0.000000000000000000 ) ) ;
#43204 = DIRECTION ( 'NONE',  ( 1.000000000000000000, -0.000000000000000000, -0.000000000000000000 ) ) ;
#43205 = DIRECTION ( 'NONE',  ( 0.000000000000000000, 0.000000000000000000, 1.000000000000000000 ) ) ;
#43206 = DIRECTION ( 'NONE',  ( 0.000000000000000000, -0.2079116908177664758, 0.9781476007338042455 ) ) ;
#43207 = DIRECTION ( 'NONE',  ( -1.000000000000000000, 0.000000000000000000, -0.000000000000000000 ) ) ;
#43208 = LINE ( 'NONE', #9669, #44928 ) ;
#43209 = LINE ( 'NONE', #5525, #147 ) ;
#43210 = ADVANCED_FACE ( 'NONE', ( #18924 ), #4274, .T. ) ;
#43211 = DIRECTION ( 'NONE',  ( 0.000000000000000000, 0.000000000000000000, 1.000000000000000000 ) ) ;
#43212 = ORIENTED_EDGE ( 'NONE', *, *, #16473, .F. ) ;
#43213 = AXIS2_PLACEMENT_3D ( 'NONE', #4331, #11905, #12393 ) ;
#43214 = CARTESIAN_POINT ( 'NONE',  ( 0.000000000000000000, 37.01155633439068282, -6.555932627142014191 ) ) ;
#43215 = EDGE_CURVE ( 'NONE', #17270, #13555, #14565, .T. ) ;
#43216 = AXIS2_PLACEMENT_3D ( 'NONE', #5730, #32163, #5487 ) ;
#43217 = DIRECTION ( 'NONE',  ( 0.000000000000000000, 0.000000000000000000, 1.000000000000000000 ) ) ;
#43218 = DIRECTION ( 'NONE',  ( 0.000000000000000000, 0.000000000000000000, 1.000000000000000000 ) ) ;
#43219 = EDGE_CURVE ( 'NONE', #48358, #37278, #20620, .T. ) ;
#43220 = CARTESIAN_POINT ( 'NONE',  ( 22.08297821871651934, -111.8242998470044540, 5.500000000000000000 ) ) ;
#43221 = DIRECTION ( 'NONE',  ( 0.7950889364178796992, -0.6064928550163510845, 0.000000000000000000 ) ) ;
#43222 = CARTESIAN_POINT ( 'NONE',  ( 5.999999999999999112, -46.11716303203136391, -67.80270845531939017 ) ) ;
#43223 = ORIENTED_EDGE ( 'NONE', *, *, #22179, .T. ) ;
#43224 = EDGE_CURVE ( 'NONE', #26631, #41727, #47971, .T. ) ;
#43225 = CARTESIAN_POINT ( 'NONE',  ( 0.000000000000000000, -18.13022148937243472, -15.02647892043568767 ) ) ;
#43226 = EDGE_CURVE ( 'NONE', #12437, #24420, #26533, .T. ) ;
#43227 = ORIENTED_EDGE ( 'NONE', *, *, #24145, .T. ) ;
#43228 = VECTOR ( 'NONE', #14763, 1000.000000000000000 ) ;
#43229 = DIRECTION ( 'NONE',  ( 0.000000000000000000, 0.9510565162951521989, 0.3090169943749515591 ) ) ;
#43230 = EDGE_LOOP ( 'NONE', ( #29292, #26410, #6605, #18239 ) ) ;
#43231 = ORIENTED_EDGE ( 'NONE', *, *, #31330, .T. ) ;
#43232 = AXIS2_PLACEMENT_3D ( 'NONE', #27457, #19370, #16204 ) ;
#43233 = CIRCLE ( 'NONE', #30721, 82.00000000000000000 ) ;
#43234 = ORIENTED_EDGE ( 'NONE', *, *, #35411, .F. ) ;
#43235 = CIRCLE ( 'NONE', #4940, 42.00000000000000000 ) ;
#43236 = AXIS2_PLACEMENT_3D ( 'NONE', #29466, #45122, #14551 ) ;
#43237 = AXIS2_PLACEMENT_3D ( 'NONE', #22438, #30019, #38092 ) ;
#43238 = CARTESIAN_POINT ( 'NONE',  ( 0.000000000000000000, 23.59884966291538433, -12.14883922797231719 ) ) ;
#43239 = ORIENTED_EDGE ( 'NONE', *, *, #24869, .T. ) ;
#43240 = VECTOR ( 'NONE', #14139, 1000.000000000000000 ) ;
#43241 = ADVANCED_FACE ( 'NONE', ( #15290 ), #10879, .T. ) ;
#43242 = EDGE_LOOP ( 'NONE', ( #4862, #27176, #24886, #18558 ) ) ;
#43243 = LINE ( 'NONE', #27592, #24198 ) ;
#43244 = AXIS2_PLACEMENT_3D ( 'NONE', #15006, #44857, #3241 ) ;
#43245 = DIRECTION ( 'NONE',  ( 0.000000000000000000, 0.000000000000000000, 1.000000000000000000 ) ) ;
#43246 = VERTEX_POINT ( 'NONE', #22384 ) ;
#43247 = ORIENTED_EDGE ( 'NONE', *, *, #13061, .F. ) ;
#43248 = VERTEX_POINT ( 'NONE', #22128 ) ;
#43249 = CIRCLE ( 'NONE', #46400, 37.49900000000000233 ) ;
#43250 = CARTESIAN_POINT ( 'NONE',  ( -22.67106064244953245, -113.6342314410295842, 5.500000000000000000 ) ) ;
#43252 = VERTEX_POINT ( 'NONE', #37308 ) ;
#43251 = DIRECTION ( 'NONE',  ( -1.000000000000000000, 0.000000000000000000, -0.000000000000000000 ) ) ;
#43253 = CARTESIAN_POINT ( 'NONE',  ( 10.00000000000000000, 0.8828120875900632436, 37.48860685352291000 ) ) ;
#43254 = ADVANCED_FACE ( 'NONE', ( #19184 ), #37786, .T. ) ;
#43255 = VERTEX_POINT ( 'NONE', #25556 ) ;
#43256 = EDGE_LOOP ( 'NONE', ( #1088, #14342, #24994, #27120 ) ) ;
#43257 = DIRECTION ( 'NONE',  ( 0.000000000000000000, 0.000000000000000000, -1.000000000000000000 ) ) ;
#43258 = ORIENTED_EDGE ( 'NONE', *, *, #22101, .T. ) ;
#43259 = DIRECTION ( 'NONE',  ( 0.000000000000000000, 0.000000000000000000, 1.000000000000000000 ) ) ;
#43260 = VERTEX_POINT ( 'NONE', #33622 ) ;
#43261 = FACE_OUTER_BOUND ( 'NONE', #4590, .T. ) ;
#43262 = EDGE_CURVE ( 'NONE', #25818, #1310, #41233, .T. ) ;
#43263 = CARTESIAN_POINT ( 'NONE',  ( 0.000000000000000000, 35.47612816024523852, 22.48208911017513145 ) ) ;
#43264 = DIRECTION ( 'NONE',  ( -1.000000000000000000, 0.000000000000000000, 0.000000000000000000 ) ) ;
#43265 = CIRCLE ( 'NONE', #15901, 15.99999999999999822 ) ;
#43266 = CARTESIAN_POINT ( 'NONE',  ( 0.000000000000000000, 50.23322058963348979, 64.81221759200361987 ) ) ;
#43267 = EDGE_CURVE ( 'NONE', #18503, #28263, #44171, .T. ) ;
#43268 = AXIS2_PLACEMENT_3D ( 'NONE', #9268, #46733, #31565 ) ;
#43269 = DIRECTION ( 'NONE',  ( -1.000000000000000000, -0.000000000000000000, 0.000000000000000000 ) ) ;
#43270 = DIRECTION ( 'NONE',  ( -1.000000000000000000, 0.000000000000000000, 0.000000000000000000 ) ) ;
#43271 = ORIENTED_EDGE ( 'NONE', *, *, #36365, .T. ) ;
#43272 = LINE ( 'NONE', #12946, #9273 ) ;
#43273 = ORIENTED_EDGE ( 'NONE', *, *, #21664, .F. ) ;
#43274 = VECTOR ( 'NONE', #27874, 1000.000000000000000 ) ;
#43275 = CARTESIAN_POINT ( 'NONE',  ( -10.00000000000000000, 0.000000000000000000, 0.000000000000000000 ) ) ;
#43276 = AXIS2_PLACEMENT_3D ( 'NONE', #10018, #36201, #24943 ) ;
#43277 = PLANE ( 'NONE',  #5213 ) ;
#43278 = CARTESIAN_POINT ( 'NONE',  ( 10.00000000000000000, 73.73191006444551476, 14.66109333815590254 ) ) ;
#43279 = CARTESIAN_POINT ( 'NONE',  ( 0.000000000000000000, -63.18004540532994184, -44.88180994100444821 ) ) ;
#43280 = EDGE_CURVE ( 'NONE', #22836, #44307, #6964, .T. ) ;
#43281 = AXIS2_PLACEMENT_3D ( 'NONE', #22680, #33695, #159 ) ;
#43282 = EDGE_CURVE ( 'NONE', #2837, #29636, #42507, .T. ) ;
#43283 = ADVANCED_FACE ( 'NONE', ( #8889 ), #27652, .F. ) ;
#43284 = DIRECTION ( 'NONE',  ( -1.000000000000000000, -0.000000000000000000, 0.000000000000000000 ) ) ;
#43285 = CARTESIAN_POINT ( 'NONE',  ( 10.00000000000000000, 40.68715046381928602, 10.41901085202092503 ) ) ;
#43286 = VERTEX_POINT ( 'NONE', #9139 ) ;
#43287 = CIRCLE ( 'NONE', #24512, 37.49900000000000944 ) ;
#43288 = AXIS2_PLACEMENT_3D ( 'NONE', #43472, #24136, #43218 ) ;
#43289 = DIRECTION ( 'NONE',  ( 0.000000000000000000, 0.000000000000000000, 1.000000000000000000 ) ) ;
#43290 = DIRECTION ( 'NONE',  ( -0.000000000000000000, -0.000000000000000000, -1.000000000000000000 ) ) ;
#43291 = CARTESIAN_POINT ( 'NONE',  ( 0.000000000000000000, -51.29473840253270112, 63.97538442413407012 ) ) ;
#43292 = ORIENTED_EDGE ( 'NONE', *, *, #39759, .F. ) ;
#43293 = CIRCLE ( 'NONE', #41745, 31.99999999999998934 ) ;
#43294 = DIRECTION ( 'NONE',  ( 0.000000000000000000, 0.000000000000000000, 1.000000000000000000 ) ) ;
#43295 = FILL_AREA_STYLE ('',( #34473 ) ) ;
#43296 = AXIS2_PLACEMENT_3D ( 'NONE', #32871, #40246, #40482 ) ;
#43297 = ORIENTED_EDGE ( 'NONE', *, *, #31750, .T. ) ;
#43298 = EDGE_CURVE ( 'NONE', #43965, #1594, #45871, .T. ) ;
#43299 = ORIENTED_EDGE ( 'NONE', *, *, #43439, .F. ) ;
#43300 = VERTEX_POINT ( 'NONE', #12572 ) ;
#43301 = CARTESIAN_POINT ( 'NONE',  ( 0.000000000000000000, -34.44570377933549565, -69.42325613327476219 ) ) ;
#43302 = CARTESIAN_POINT ( 'NONE',  ( -1.200000000000000030E-05, 16.95692799528845640, -2.500000000000000000 ) ) ;
#43303 = ORIENTED_EDGE ( 'NONE', *, *, #42441, .T. ) ;
#43304 = AXIS2_PLACEMENT_3D ( 'NONE', #22689, #4099, #425 ) ;
#43305 = VECTOR ( 'NONE', #44106, 1000.000000000000227 ) ;
#43306 = DIRECTION ( 'NONE',  ( 1.000000000000000000, 0.000000000000000000, 0.000000000000000000 ) ) ;
#43307 = VECTOR ( 'NONE', #45362, 1000.000000000000000 ) ;
#43308 = VECTOR ( 'NONE', #41051, 1000.000000000000114 ) ;
#43309 = AXIS2_PLACEMENT_3D ( 'NONE', #5308, #1876, #17506 ) ;
#43310 = EDGE_LOOP ( 'NONE', ( #39023, #30128, #24511, #18430 ) ) ;
#43311 = ORIENTED_EDGE ( 'NONE', *, *, #33981, .T. ) ;
#43312 = ORIENTED_EDGE ( 'NONE', *, *, #11111, .T. ) ;
#43313 = ORIENTED_EDGE ( 'NONE', *, *, #23288, .F. ) ;
#43314 = DIRECTION ( 'NONE',  ( -1.000000000000000000, 0.000000000000000000, -0.000000000000000000 ) ) ;
#43315 = EDGE_CURVE ( 'NONE', #39130, #25331, #42180, .T. ) ;
#43316 = AXIS2_PLACEMENT_3D ( 'NONE', #22533, #12424, #19739 ) ;
#43317 = CIRCLE ( 'NONE', #22213, 37.49900000000000233 ) ;
#43318 = ORIENTED_EDGE ( 'NONE', *, *, #1723, .T. ) ;
#43319 = DIRECTION ( 'NONE',  ( -1.000000000000000000, -0.000000000000000000, 0.000000000000000000 ) ) ;
#43320 = ORIENTED_EDGE ( 'NONE', *, *, #18537, .F. ) ;
#43321 = CIRCLE ( 'NONE', #5016, 82.00000000000000000 ) ;
#43322 = DIRECTION ( 'NONE',  ( -1.000000000000000000, -0.000000000000000000, 0.000000000000000000 ) ) ;
#43323 = VECTOR ( 'NONE', #29801, 1000.000000000000000 ) ;
#43324 = EDGE_CURVE ( 'NONE', #46585, #22321, #20379, .T. ) ;
#43325 = DIRECTION ( 'NONE',  ( -1.000000000000000000, 0.000000000000000000, 0.000000000000000000 ) ) ;
#43326 = CARTESIAN_POINT ( 'NONE',  ( 12.49999999999999645, 1.530808498934191127E-15, -44.99999999999998579 ) ) ;
#43327 = ADVANCED_FACE ( 'NONE', ( #31186 ), #23103, .T. ) ;
#43329 = ORIENTED_EDGE ( 'NONE', *, *, #3465, .F. ) ;
#43328 = AXIS2_PLACEMENT_3D ( 'NONE', #6707, #25532, #3254 ) ;
#43330 = LINE ( 'NONE', #21267, #18057 ) ;
#43331 = ORIENTED_EDGE ( 'NONE', *, *, #24323, .T. ) ;
#43332 = CARTESIAN_POINT ( 'NONE',  ( 11.99999999999999822, -75.16055320797016748, -18.89407956138335365 ) ) ;
#43333 = DIRECTION ( 'NONE',  ( -0.000000000000000000, -0.000000000000000000, 1.000000000000000000 ) ) ;
#43334 = VERTEX_POINT ( 'NONE', #45608 ) ;
#43335 = ORIENTED_EDGE ( 'NONE', *, *, #14816, .F. ) ;
#43336 = CARTESIAN_POINT ( 'NONE',  ( 10.00000000000000000, 0.000000000000000000, 0.000000000000000000 ) ) ;
#43337 = CARTESIAN_POINT ( 'NONE',  ( 10.00000000000000000, 16.45098606841126454, 33.79645857604518966 ) ) ;
#43338 = ORIENTED_EDGE ( 'NONE', *, *, #8425, .F. ) ;
#43339 = DIRECTION ( 'NONE',  ( 0.000000000000000000, 0.000000000000000000, 1.000000000000000000 ) ) ;
#43340 = CARTESIAN_POINT ( 'NONE',  ( 16.30584220631899228, -140.9432449716519784, 5.500000000000000000 ) ) ;
#43341 = DIRECTION ( 'NONE',  ( -1.000000000000000000, 0.000000000000000000, 0.000000000000000000 ) ) ;
#43342 = CIRCLE ( 'NONE', #1117, 37.49900000000000944 ) ;
#43343 = DIRECTION ( 'NONE',  ( -1.000000000000000000, -0.000000000000000000, -0.000000000000000000 ) ) ;
#43344 = EDGE_CURVE ( 'NONE', #30381, #4357, #12805, .T. ) ;
#43345 = EDGE_CURVE ( 'NONE', #22843, #29358, #27264, .T. ) ;
#43346 = LINE ( 'NONE', #21285, #43496 ) ;
#43347 = LINE ( 'NONE', #24023, #33265 ) ;
#43348 = CARTESIAN_POINT ( 'NONE',  ( 15.00000000000000000, 5.835314593368777558, 22.81335362449846471 ) ) ;
#43349 = AXIS2_PLACEMENT_3D ( 'NONE', #36093, #16533, #28757 ) ;
#43350 = CARTESIAN_POINT ( 'NONE',  ( 10.00000000000000000, 0.000000000000000000, 0.000000000000000000 ) ) ;
#43352 = AXIS2_PLACEMENT_3D ( 'NONE', #40718, #22599, #4254 ) ;
#43351 = DIRECTION ( 'NONE',  ( 0.000000000000000000, 0.7071067811865487940, -0.7071067811865462405 ) ) ;
#43353 = CARTESIAN_POINT ( 'NONE',  ( 11.41210121379328335, -99.40233154247455616, 5.500000000000000000 ) ) ;
#43354 = CARTESIAN_POINT ( 'NONE',  ( 11.99999999999999822, 2.956366410620650420, 75.11725578898469280 ) ) ;
#43355 = CARTESIAN_POINT ( 'NONE',  ( 0.000000000000000000, 0.000000000000000000, -125.0000000000000000 ) ) ;
#43356 = ORIENTED_EDGE ( 'NONE', *, *, #32178, .T. ) ;
#43357 = EDGE_CURVE ( 'NONE', #3234, #40846, #8638, .T. ) ;
#43358 = VERTEX_POINT ( 'NONE', #27028 ) ;
#43360 = DIRECTION ( 'NONE',  ( 0.000000000000000000, 0.000000000000000000, 1.000000000000000000 ) ) ;
#43359 = VECTOR ( 'NONE', #30480, 1000.000000000000000 ) ;
#43361 = CIRCLE ( 'NONE', #33939, 31.99999999999998579 ) ;
#43362 = CIRCLE ( 'NONE', #14417, 15.99999999999999467 ) ;
#43363 = DIRECTION ( 'NONE',  ( 0.000000000000000000, 0.000000000000000000, 1.000000000000000000 ) ) ;
#43364 = CIRCLE ( 'NONE', #2704, 31.99999999999998934 ) ;
#43365 = ITEM_DEFINED_TRANSFORMATION ( 'NONE', 'NONE', #10839,  #11636 ) ;
#43366 = DIRECTION ( 'NONE',  ( -1.000000000000000000, 0.000000000000000000, 0.000000000000000000 ) ) ;
#43367 = CIRCLE ( 'NONE', #38661, 31.99999999999998579 ) ;
#43368 = EDGE_LOOP ( 'NONE', ( #39154, #31082, #23661, #7189 ) ) ;
#43369 = EDGE_LOOP ( 'NONE', ( #46771, #21388, #17787, #32099 ) ) ;
#43370 = DIRECTION ( 'NONE',  ( -1.000000000000000000, 0.000000000000000000, -0.000000000000000000 ) ) ;
#43371 = ORIENTED_EDGE ( 'NONE', *, *, #41867, .T. ) ;
#43372 = CARTESIAN_POINT ( 'NONE',  ( 0.000000000000000000, 41.91543099594818500, -2.663952781846294915 ) ) ;
#43373 = ORIENTED_EDGE ( 'NONE', *, *, #38815, .F. ) ;
#43374 = DIRECTION ( 'NONE',  ( -1.000000000000000000, 0.000000000000000000, 0.000000000000000000 ) ) ;
#43375 = AXIS2_PLACEMENT_3D ( 'NONE', #43275, #32260, #15044 ) ;
#43376 = DIRECTION ( 'NONE',  ( -1.000000000000000000, -0.000000000000000000, 0.000000000000000000 ) ) ;
#43377 = VERTEX_POINT ( 'NONE', #31431 ) ;
#43378 = DIRECTION ( 'NONE',  ( 0.000000000000000000, 0.9510565162951521989, 0.3090169943749515591 ) ) ;
#43379 = DIRECTION ( 'NONE',  ( 0.000000000000000000, 0.000000000000000000, 1.000000000000000000 ) ) ;
#43380 = ORIENTED_EDGE ( 'NONE', *, *, #2335, .F. ) ;
#43381 = EDGE_CURVE ( 'NONE', #38831, #25953, #3421, .T. ) ;
#43382 = ORIENTED_EDGE ( 'NONE', *, *, #16983, .F. ) ;
#43383 = DIRECTION ( 'NONE',  ( 9.814797785686868941E-17, 1.000000000000000000, 0.000000000000000000 ) ) ;
#43384 = EDGE_CURVE ( 'NONE', #33558, #960, #9683, .T. ) ;
#43385 = DIRECTION ( 'NONE',  ( -1.000000000000000000, 0.000000000000000000, 0.000000000000000000 ) ) ;
#43386 = CARTESIAN_POINT ( 'NONE',  ( 0.000000000000000000, 50.95692526931328104, 58.39081064771769292 ) ) ;
#43387 = DIRECTION ( 'NONE',  ( -1.000000000000000000, -0.000000000000000000, -0.000000000000000000 ) ) ;
#43388 = DIRECTION ( 'NONE',  ( -0.000000000000000000, -0.000000000000000000, -1.000000000000000000 ) ) ;
#43389 = AXIS2_PLACEMENT_3D ( 'NONE', #47566, #14046, #10368 ) ;
#43390 = VERTEX_POINT ( 'NONE', #24075 ) ;
#43391 = CARTESIAN_POINT ( 'NONE',  ( -10.00000000000000000, 0.000000000000000000, 0.000000000000000000 ) ) ;
#43392 = ORIENTED_EDGE ( 'NONE', *, *, #22820, .T. ) ;
#43393 = ORIENTED_EDGE ( 'NONE', *, *, #38645, .T. ) ;
#43394 = EDGE_CURVE ( 'NONE', #14647, #1729, #8411, .T. ) ;
#43395 = CARTESIAN_POINT ( 'NONE',  ( 0.000000000000000000, 0.000000000000000000, 0.000000000000000000 ) ) ;
#43396 = CARTESIAN_POINT ( 'NONE',  ( 11.99999999999999822, 73.72996012237440766, 14.67089635893739619 ) ) ;
#43397 = AXIS2_PLACEMENT_3D ( 'NONE', #20559, #5645, #39425 ) ;
#43398 = DIRECTION ( 'NONE',  ( -1.000000000000000000, 0.000000000000000000, 0.000000000000000000 ) ) ;
#43399 = DIRECTION ( 'NONE',  ( 0.000000000000000000, -0.5877852522924801315, 0.8090169943749421222 ) ) ;
#43400 = ORIENTED_EDGE ( 'NONE', *, *, #35915, .T. ) ;
#43401 = CYLINDRICAL_SURFACE ( 'NONE', #40967, 77.49899999999999523 ) ;
#43402 = VECTOR ( 'NONE', #9920, 1000.000000000000000 ) ;
#43403 = CARTESIAN_POINT ( 'NONE',  ( 0.000000000000000000, 0.000000000000000000, 0.000000000000000000 ) ) ;
#43404 = VECTOR ( 'NONE', #10308, 1000.000000000000000 ) ;
#43405 = CARTESIAN_POINT ( 'NONE',  ( 0.000000000000000000, 26.08949754953024325, 27.05870788708241648 ) ) ;
#43406 = EDGE_CURVE ( 'NONE', #9901, #14655, #20651, .T. ) ;
#43407 = DIRECTION ( 'NONE',  ( -1.000000000000000000, 0.000000000000000000, 0.000000000000000000 ) ) ;
#43408 = DIRECTION ( 'NONE',  ( -1.000000000000000000, 0.000000000000000000, 0.000000000000000000 ) ) ;
#43409 = DIRECTION ( 'NONE',  ( 0.000000000000000000, 0.9510565162951544194, -0.3090169943749448422 ) ) ;
#43410 = EDGE_CURVE ( 'NONE', #15076, #11714, #42680, .T. ) ;
#43411 = DIRECTION ( 'NONE',  ( -1.000000000000000000, 0.000000000000000000, 0.000000000000000000 ) ) ;
#43412 = CARTESIAN_POINT ( 'NONE',  ( 0.000000000000000000, -71.87247863392443037, 39.47590169984818687 ) ) ;
#43413 = DIRECTION ( 'NONE',  ( 0.000000000000000000, 0.000000000000000000, 1.000000000000000000 ) ) ;
#43414 = CIRCLE ( 'NONE', #25419, 31.99999999999998579 ) ;
#43415 = CARTESIAN_POINT ( 'NONE',  ( -3.000000000000000000, -10.45096189432344147, 21.10159698893426494 ) ) ;
#43416 = DIRECTION ( 'NONE',  ( -1.000000000000000000, 0.000000000000000000, 0.000000000000000000 ) ) ;
#43417 = ORIENTED_EDGE ( 'NONE', *, *, #29253, .F. ) ;
#43418 = EDGE_CURVE ( 'NONE', #35093, #42101, #35317, .T. ) ;
#43419 = ORIENTED_EDGE ( 'NONE', *, *, #43345, .T. ) ;
#43420 = VECTOR ( 'NONE', #4746, 1000.000000000000000 ) ;
#43421 = CARTESIAN_POINT ( 'NONE',  ( -3.000000000000000000, 22.07842321921481243, 8.187992925817422218 ) ) ;
#43422 = EDGE_LOOP ( 'NONE', ( #30531, #3267, #4711, #46204 ) ) ;
#43423 = CARTESIAN_POINT ( 'NONE',  ( 10.00000000000000000, 10.96151621346540317, -35.95386929396244113 ) ) ;
#43424 = VECTOR ( 'NONE', #4679, 1000.000000000000000 ) ;
#43425 = CARTESIAN_POINT ( 'NONE',  ( 10.00000000000000000, -35.91791733033426226, -68.67312586195033930 ) ) ;
#43426 = ORIENTED_EDGE ( 'NONE', *, *, #27156, .T. ) ;
#43427 = EDGE_CURVE ( 'NONE', #6120, #4472, #12841, .T. ) ;
#43428 = AXIS2_PLACEMENT_3D ( 'NONE', #40429, #17654, #48243 ) ;
#43429 = VECTOR ( 'NONE', #36022, 1000.000000000000000 ) ;
#43430 = DIRECTION ( 'NONE',  ( 1.000000000000000000, 0.000000000000000000, -0.000000000000000000 ) ) ;
#43431 = CIRCLE ( 'NONE', #25445, 77.49900000000000944 ) ;
#43432 = ORIENTED_EDGE ( 'NONE', *, *, #22995, .F. ) ;
#43433 = VERTEX_POINT ( 'NONE', #16005 ) ;
#43434 = CIRCLE ( 'NONE', #16845, 77.49900000000000944 ) ;
#43435 = AXIS2_PLACEMENT_3D ( 'NONE', #25653, #28631, #44510 ) ;
#43436 = CIRCLE ( 'NONE', #27786, 15.99999999999999822 ) ;
#43437 = DIRECTION ( 'NONE',  ( -1.000000000000000000, -0.000000000000000000, -0.000000000000000000 ) ) ;
#43438 = ORIENTED_EDGE ( 'NONE', *, *, #14320, .T. ) ;
#43439 = EDGE_CURVE ( 'NONE', #12057, #12729, #8171, .T. ) ;
#43440 = DIRECTION ( 'NONE',  ( -1.000000000000000000, -0.000000000000000000, -0.000000000000000000 ) ) ;
#43441 = DIRECTION ( 'NONE',  ( 0.000000000000000000, -0.1564344650402381687, 0.9876883405951365491 ) ) ;
#43442 = VERTEX_POINT ( 'NONE', #4737 ) ;
#43443 = EDGE_CURVE ( 'NONE', #8637, #30376, #14408, .T. ) ;
#43444 = DIRECTION ( 'NONE',  ( 0.000000000000000000, 0.000000000000000000, 1.000000000000000000 ) ) ;
#43445 = VECTOR ( 'NONE', #39378, 1000.000000000000000 ) ;
#43446 = ORIENTED_EDGE ( 'NONE', *, *, #44687, .T. ) ;
#43447 = ORIENTED_EDGE ( 'NONE', *, *, #19696, .F. ) ;
#43448 = EDGE_CURVE ( 'NONE', #1286, #6051, #28452, .T. ) ;
#43449 = DIRECTION ( 'NONE',  ( -1.000000000000000000, 0.000000000000000000, 0.000000000000000000 ) ) ;
#43450 = FACE_OUTER_BOUND ( 'NONE', #2626, .T. ) ;
#43451 = CARTESIAN_POINT ( 'NONE',  ( -10.00000000000000000, 0.000000000000000000, 0.000000000000000000 ) ) ;
#43452 = AXIS2_PLACEMENT_3D ( 'NONE', #1267, #41909, #30403 ) ;
#43453 = ORIENTED_EDGE ( 'NONE', *, *, #6354, .F. ) ;
#43454 = CARTESIAN_POINT ( 'NONE',  ( 11.99999999999999822, -73.95703589263958122, -23.16143007188505010 ) ) ;
#43455 = ORIENTED_EDGE ( 'NONE', *, *, #9037, .T. ) ;
#43456 = EDGE_CURVE ( 'NONE', #9518, #4524, #35512, .T. ) ;
#43457 = DIRECTION ( 'NONE',  ( -0.000000000000000000, -0.000000000000000000, -1.000000000000000000 ) ) ;
#43458 = FACE_OUTER_BOUND ( 'NONE', #32057, .T. ) ;
#43459 = DIRECTION ( 'NONE',  ( -1.000000000000000000, -0.000000000000000000, 0.000000000000000000 ) ) ;
#43460 = CARTESIAN_POINT ( 'NONE',  ( 11.99999999999999822, 56.15606465354957777, 59.75363087400094031 ) ) ;
#43461 = CYLINDRICAL_SURFACE ( 'NONE', #19039, 77.49899999999999523 ) ;
#43462 = DIRECTION ( 'NONE',  ( -1.000000000000000000, -0.000000000000000000, 0.000000000000000000 ) ) ;
#43463 = CARTESIAN_POINT ( 'NONE',  ( 10.00000000000000000, -46.53671651293907274, -59.03961581697448935 ) ) ;
#43464 = DIRECTION ( 'NONE',  ( 0.000000000000000000, 0.000000000000000000, 1.000000000000000000 ) ) ;
#43465 = CARTESIAN_POINT ( 'NONE',  ( 25.81725066941077529, -113.8380548628854854, 5.500000000000000000 ) ) ;
#43466 = LINE ( 'NONE', #36102, #45769 ) ;
#43467 = ORIENTED_EDGE ( 'NONE', *, *, #30008, .T. ) ;
#43468 = VERTEX_POINT ( 'NONE', #29595 ) ;
#43469 = CARTESIAN_POINT ( 'NONE',  ( 12.00000000000000000, 6.762365576493649222, 25.66652317338391853 ) ) ;
#43470 = AXIS2_PLACEMENT_3D ( 'NONE', #26484, #22567, #33574 ) ;
#43471 = DIRECTION ( 'NONE',  ( 0.000000000000000000, 0.000000000000000000, 1.000000000000000000 ) ) ;
#43472 = CARTESIAN_POINT ( 'NONE',  ( -10.00000000000000000, 0.000000000000000000, 0.000000000000000000 ) ) ;
#43473 = AXIS2_PLACEMENT_3D ( 'NONE', #19892, #4972, #41695 ) ;
#43474 = CARTESIAN_POINT ( 'NONE',  ( 0.000000000000000000, 8.840884882376133902, -74.65374052328640175 ) ) ;
#43475 = ADVANCED_FACE ( 'NONE', ( #31917 ), #13527, .T. ) ;
#43476 = CYLINDRICAL_SURFACE ( 'NONE', #3671, 82.00000000000000000 ) ;
#43477 = CARTESIAN_POINT ( 'NONE',  ( 0.000000000000000000, -59.03342792756297541, 46.54456581323783126 ) ) ;
#43478 = ORIENTED_EDGE ( 'NONE', *, *, #44319, .F. ) ;
#43479 = LINE ( 'NONE', #43225, #33216 ) ;
#43480 = ORIENTED_EDGE ( 'NONE', *, *, #40677, .F. ) ;
#43481 = CIRCLE ( 'NONE', #30979, 16.00000000000000355 ) ;
#43482 = LINE ( 'NONE', #39577, #15825 ) ;
#43483 = VERTEX_POINT ( 'NONE', #25017 ) ;
#43484 = VERTEX_POINT ( 'NONE', #16962 ) ;
#43485 = CIRCLE ( 'NONE', #28625, 15.99999999999999645 ) ;
#43486 = VERTEX_POINT ( 'NONE', #6431 ) ;
#43487 = VERTEX_POINT ( 'NONE', #32383 ) ;
#43488 = DIRECTION ( 'NONE',  ( -0.5200609990132993854, -0.8541291221503275466, 0.000000000000000000 ) ) ;
#43489 = AXIS2_PLACEMENT_3D ( 'NONE', #31744, #20698, #35633 ) ;
#43490 = ORIENTED_EDGE ( 'NONE', *, *, #12544, .T. ) ;
#43491 = EDGE_LOOP ( 'NONE', ( #22430, #39919, #8940, #43505 ) ) ;
#43492 = EDGE_CURVE ( 'NONE', #21764, #28312, #4247, .T. ) ;
#43493 = CARTESIAN_POINT ( 'NONE',  ( 10.00000000000000000, -62.50884508063453637, 41.76106447765467777 ) ) ;
#43494 = CARTESIAN_POINT ( 'NONE',  ( 0.000000000000000000, 39.47590169984846398, 71.87247863392428826 ) ) ;
#43495 = VERTEX_POINT ( 'NONE', #9367 ) ;
#43496 = VECTOR ( 'NONE', #24739, 1000.000000000000000 ) ;
#43497 = ORIENTED_EDGE ( 'NONE', *, *, #5826, .F. ) ;
#43498 = EDGE_CURVE ( 'NONE', #35718, #18061, #44524, .T. ) ;
#43499 = ORIENTED_EDGE ( 'NONE', *, *, #39518, .T. ) ;
#43500 = CARTESIAN_POINT ( 'NONE',  ( 0.000000000000000000, 0.000000000000000000, 0.000000000000000000 ) ) ;
#43501 = DIRECTION ( 'NONE',  ( -1.000000000000000000, -0.000000000000000000, -0.000000000000000000 ) ) ;
#43502 = DIRECTION ( 'NONE',  ( 0.000000000000000000, 0.1564344650402244852, 0.9876883405951387696 ) ) ;
#43503 = ORIENTED_EDGE ( 'NONE', *, *, #6311, .F. ) ;
#43504 = AXIS2_PLACEMENT_3D ( 'NONE', #47185, #13415, #20507 ) ;
#43505 = ORIENTED_EDGE ( 'NONE', *, *, #24528, .F. ) ;
#43506 = CARTESIAN_POINT ( 'NONE',  ( 0.000000000000000000, 20.40083707022987625, -72.35432306680462489 ) ) ;
#43507 = VERTEX_POINT ( 'NONE', #10096 ) ;
#43508 = EDGE_CURVE ( 'NONE', #32773, #41443, #19844, .T. ) ;
#43509 = CARTESIAN_POINT ( 'NONE',  ( 10.00000000000000000, 22.74946021919175720, -29.81001611430984255 ) ) ;
#43510 = DIRECTION ( 'NONE',  ( -0.000000000000000000, -0.000000000000000000, -1.000000000000000000 ) ) ;
#43511 = ADVANCED_FACE ( 'NONE', ( #2049 ), #43401, .T. ) ;
#43512 = CARTESIAN_POINT ( 'NONE',  ( 0.000000000000000000, 28.89263327155848415, -71.91182617369156560 ) ) ;
#43513 = DIRECTION ( 'NONE',  ( 0.000000000000000000, 0.000000000000000000, 1.000000000000000000 ) ) ;
#43514 = DIRECTION ( 'NONE',  ( 0.000000000000000000, 0.000000000000000000, 1.000000000000000000 ) ) ;
#43515 = AXIS2_PLACEMENT_3D ( 'NONE', #12268, #31110, #8339 ) ;
#43516 = DIRECTION ( 'NONE',  ( 0.000000000000000000, 0.3826834323650841752, 0.9238795325112891810 ) ) ;
#43517 = DIRECTION ( 'NONE',  ( -1.000000000000000000, 0.000000000000000000, 0.000000000000000000 ) ) ;
#43518 = ORIENTED_EDGE ( 'NONE', *, *, #1224, .F. ) ;
#43519 = DIRECTION ( 'NONE',  ( -1.000000000000000000, -0.000000000000000000, -0.000000000000000000 ) ) ;
#43520 = VERTEX_POINT ( 'NONE', #40858 ) ;
#43521 = LINE ( 'NONE', #21226, #11346 ) ;
#43522 = LINE ( 'NONE', #22137, #24740 ) ;
#43523 = CARTESIAN_POINT ( 'NONE',  ( -3.000000000000000000, -22.67460108101783334, 6.353146135317912169 ) ) ;
#43524 = VERTEX_POINT ( 'NONE', #43155 ) ;
#43525 = DIRECTION ( 'NONE',  ( -1.000000000000000000, -0.000000000000000000, 0.000000000000000000 ) ) ;
#43526 = EDGE_CURVE ( 'NONE', #42271, #11749, #7321, .T. ) ;
#43527 = CARTESIAN_POINT ( 'NONE',  ( 10.00000000000000000, 0.000000000000000000, 0.000000000000000000 ) ) ;
#43528 = CIRCLE ( 'NONE', #20065, 82.00000000000000000 ) ;
#43529 = ORIENTED_EDGE ( 'NONE', *, *, #1153, .F. ) ;
#43530 = CARTESIAN_POINT ( 'NONE',  ( -9.332068499558246799, 6.890028847512375876, 42.00000000000001421 ) ) ;
#43531 = CARTESIAN_POINT ( 'NONE',  ( 2.874421927457452952, -143.3717286177755739, 5.500000000000000000 ) ) ;
#43532 = CARTESIAN_POINT ( 'NONE',  ( 25.81725066941077529, -113.8380548628854854, 5.500000000000000000 ) ) ;
#43533 =( REPRESENTATION_RELATIONSHIP ('NONE','NONE', #5957, #45973 ) REPRESENTATION_RELATIONSHIP_WITH_TRANSFORMATION ( #2705 )SHAPE_REPRESENTATION_RELATIONSHIP( ) );
#43534 = CIRCLE ( 'NONE', #4475, 16.00000000000000000 ) ;
#43535 = DIRECTION ( 'NONE',  ( 1.000000000000000000, -0.000000000000000000, -0.000000000000000000 ) ) ;
#43536 = VERTEX_POINT ( 'NONE', #9857 ) ;
#43537 = ORIENTED_EDGE ( 'NONE', *, *, #11412, .T. ) ;
#43538 = ORIENTED_EDGE ( 'NONE', *, *, #1704, .T. ) ;
#43539 = ADVANCED_FACE ( 'NONE', ( #22261 ), #46595, .F. ) ;
#43540 = PLANE ( 'NONE',  #18667 ) ;
#43541 = CIRCLE ( 'NONE', #21633, 37.49900000000000944 ) ;
#43542 = CARTESIAN_POINT ( 'NONE',  ( 11.99999999999999822, 0.000000000000000000, 0.000000000000000000 ) ) ;
#43543 = EDGE_CURVE ( 'NONE', #26599, #39866, #2265, .T. ) ;
#43544 = VERTEX_POINT ( 'NONE', #36282 ) ;
#43545 = AXIS2_PLACEMENT_3D ( 'NONE', #21670, #36357, #33168 ) ;
#43546 = LINE ( 'NONE', #2896, #38244 ) ;
#43547 = ORIENTED_EDGE ( 'NONE', *, *, #13995, .F. ) ;
#43548 = VERTEX_POINT ( 'NONE', #17679 ) ;
#43549 = EDGE_LOOP ( 'NONE', ( #42619, #20816, #9621, #30320 ) ) ;
#43550 = EDGE_CURVE ( 'NONE', #22912, #41381, #32610, .T. ) ;
#43551 = EDGE_CURVE ( 'NONE', #38691, #19053, #47063, .T. ) ;
#43552 = EDGE_CURVE ( 'NONE', #33236, #32480, #39238, .T. ) ;
#43553 = AXIS2_PLACEMENT_3D ( 'NONE', #327, #45130, #38503 ) ;
#43554 = CARTESIAN_POINT ( 'NONE',  ( 8.700667342345820288, -98.11853780484867116, 2.500000000000000000 ) ) ;
#43555 = ORIENTED_EDGE ( 'NONE', *, *, #32459, .F. ) ;
#43556 = DIRECTION ( 'NONE',  ( -1.000000000000000000, 0.000000000000000000, 0.000000000000000000 ) ) ;
#43557 = ORIENTED_EDGE ( 'NONE', *, *, #45655, .F. ) ;
#43558 = CARTESIAN_POINT ( 'NONE',  ( 10.00000000000000000, -41.19522573413780009, 65.64334221924896440 ) ) ;
#43559 = AXIS2_PLACEMENT_3D ( 'NONE', #43754, #3605, #14869 ) ;
#43560 = EDGE_CURVE ( 'NONE', #1910, #39296, #30806, .T. ) ;
#43561 = CARTESIAN_POINT ( 'NONE',  ( 0.000000000000000000, -30.00120703465189465, -22.64427369931201639 ) ) ;
#43562 = CARTESIAN_POINT ( 'NONE',  ( 5.000000000000000000, 39.04073710021344112, 15.48615015657596850 ) ) ;
#43563 = ORIENTED_EDGE ( 'NONE', *, *, #23862, .T. ) ;
#43564 = CARTESIAN_POINT ( 'NONE',  ( 11.99999999999999822, -65.59268652807237743, 36.72794159290217664 ) ) ;
#43565 = ORIENTED_EDGE ( 'NONE', *, *, #13214, .F. ) ;
#43566 = FACE_OUTER_BOUND ( 'NONE', #12865, .T. ) ;
#43567 = FACE_OUTER_BOUND ( 'NONE', #33886, .T. ) ;
#43568 = CIRCLE ( 'NONE', #9951, 77.49899999999999523 ) ;
#43569 = ORIENTED_EDGE ( 'NONE', *, *, #664, .F. ) ;
#43570 = ORIENTED_EDGE ( 'NONE', *, *, #22195, .F. ) ;
#43571 = CARTESIAN_POINT ( 'NONE',  ( -0.8815729230226008184, -93.47222532549339746, 5.500000000000000000 ) ) ;
#43572 = CARTESIAN_POINT ( 'NONE',  ( 0.000000000000000000, 0.000000000000000000, 0.000000000000000000 ) ) ;
#43573 = ORIENTED_EDGE ( 'NONE', *, *, #21833, .F. ) ;
#43574 = CARTESIAN_POINT ( 'NONE',  ( 10.00000000000000000, 33.79645857604513992, -16.45098606841138178 ) ) ;
#43575 = CARTESIAN_POINT ( 'NONE',  ( 10.00000000000000000, -30.00120703465189465, -22.64427369931201639 ) ) ;
#43576 = DIRECTION ( 'NONE',  ( -0.4796670183876317051, 0.8774505977381971134, 0.000000000000000000 ) ) ;
#43577 = CARTESIAN_POINT ( 'NONE',  ( 0.000000000000000000, 10.74501242461333028, -35.92658777277499382 ) ) ;
#43578 = AXIS2_PLACEMENT_3D ( 'NONE', #22143, #37560, #18479 ) ;
#43579 = CARTESIAN_POINT ( 'NONE',  ( -10.00000000000000000, 0.000000000000000000, 0.000000000000000000 ) ) ;
#43580 = DIRECTION ( 'NONE',  ( 0.000000000000000000, 0.000000000000000000, -1.000000000000000000 ) ) ;
#43581 = LINE ( 'NONE', #5909, #7449 ) ;
#43582 = DIRECTION ( 'NONE',  ( 0.000000000000000000, 0.000000000000000000, 1.000000000000000000 ) ) ;
#43583 = DIRECTION ( 'NONE',  ( 0.000000000000000000, 0.5877852522924744694, -0.8090169943749465631 ) ) ;
#43584 = DIRECTION ( 'NONE',  ( -0.000000000000000000, -0.000000000000000000, -1.000000000000000000 ) ) ;
#43585 = LINE ( 'NONE', #17147, #16327 ) ;
#43586 = CYLINDRICAL_SURFACE ( 'NONE', #30310, 82.00000000000000000 ) ;
#43587 = ORIENTED_EDGE ( 'NONE', *, *, #40729, .F. ) ;
#43588 = ORIENTED_EDGE ( 'NONE', *, *, #30985, .T. ) ;
#43589 = CIRCLE ( 'NONE', #22482, 32.00000000000000000 ) ;
#43590 = EDGE_CURVE ( 'NONE', #25422, #18426, #20882, .T. ) ;
#43591 = CARTESIAN_POINT ( 'NONE',  ( 15.00000000000000000, 14.60985201121729737, 18.46759930825687235 ) ) ;
#43592 = EDGE_CURVE ( 'NONE', #41683, #34932, #36038, .T. ) ;
#43593 = ITEM_DEFINED_TRANSFORMATION ( 'NONE', 'NONE', #24110,  #11636 ) ;
#43594 = VECTOR ( 'NONE', #48153, 1000.000000000000000 ) ;
#43595 = DIRECTION ( 'NONE',  ( -1.000000000000000000, 0.000000000000000000, 0.000000000000000000 ) ) ;
#43596 = ADVANCED_FACE ( 'NONE', ( #4143 ), #11268, .F. ) ;
#43597 = ORIENTED_EDGE ( 'NONE', *, *, #45219, .F. ) ;
#43598 = AXIS2_PLACEMENT_3D ( 'NONE', #19720, #42504, #38114 ) ;
#43599 = DIRECTION ( 'NONE',  ( 0.000000000000000000, 0.000000000000000000, -1.000000000000000000 ) ) ;
#43600 = ORIENTED_EDGE ( 'NONE', *, *, #12280, .T. ) ;
#43601 = CYLINDRICAL_SURFACE ( 'NONE', #8895, 16.00000000000000000 ) ;
#43602 = ORIENTED_EDGE ( 'NONE', *, *, #32751, .F. ) ;
#43603 = FACE_OUTER_BOUND ( 'NONE', #39444, .T. ) ;
#43604 = EDGE_CURVE ( 'NONE', #3463, #40000, #40203, .T. ) ;
#43605 = EDGE_CURVE ( 'NONE', #40065, #7437, #19079, .T. ) ;
#43606 = AXIS2_PLACEMENT_3D ( 'NONE', #25369, #14364, #21705 ) ;
#43607 = ORIENTED_EDGE ( 'NONE', *, *, #41146, .F. ) ;
#43608 = CARTESIAN_POINT ( 'NONE',  ( 10.00000000000000000, 4.992566952385523393, -37.16516213103272293 ) ) ;
#43609 = DIRECTION ( 'NONE',  ( 0.000000000000000000, 0.000000000000000000, 1.000000000000000000 ) ) ;
#43610 = ORIENTED_EDGE ( 'NONE', *, *, #9390, .T. ) ;
#43611 = CYLINDRICAL_SURFACE ( 'NONE', #13726, 31.99999999999998579 ) ;
#43612 = VERTEX_POINT ( 'NONE', #45020 ) ;
#43613 = ORIENTED_EDGE ( 'NONE', *, *, #47840, .F. ) ;
#43614 = DIRECTION ( 'NONE',  ( -0.000000000000000000, -0.000000000000000000, -1.000000000000000000 ) ) ;
#43615 = PLANE ( 'NONE',  #20584 ) ;
#43616 = CARTESIAN_POINT ( 'NONE',  ( 4.999999999999999112, 41.81611651403868990, -3.925862922255709542 ) ) ;
#43617 = EDGE_CURVE ( 'NONE', #27937, #46875, #30032, .T. ) ;
#43619 = FACE_OUTER_BOUND ( 'NONE', #25082, .T. ) ;
#43618 = VECTOR ( 'NONE', #30153, 1000.000000000000227 ) ;
#43620 = CARTESIAN_POINT ( 'NONE',  ( 10.00000000000000000, 0.000000000000000000, 0.000000000000000000 ) ) ;
#43621 = ORIENTED_EDGE ( 'NONE', *, *, #46112, .F. ) ;
#43622 = LINE ( 'NONE', #10086, #9206 ) ;
#43623 = ORIENTED_EDGE ( 'NONE', *, *, #17683, .F. ) ;
#43624 = ORIENTED_EDGE ( 'NONE', *, *, #36527, .F. ) ;
#43625 = DIRECTION ( 'NONE',  ( 0.000000000000000000, 0.4067366430757887730, 0.9135454576426059736 ) ) ;
#43626 = ORIENTED_EDGE ( 'NONE', *, *, #27757, .T. ) ;
#43627 = AXIS2_PLACEMENT_3D ( 'NONE', #37263, #19138, #11801 ) ;
#43628 = DIRECTION ( 'NONE',  ( -1.000000000000000000, -0.000000000000000000, 0.000000000000000000 ) ) ;
#43629 = LINE ( 'NONE', #47533, #37579 ) ;
#43630 = DIRECTION ( 'NONE',  ( 0.000000000000000000, 0.000000000000000000, 1.000000000000000000 ) ) ;
#43631 = ORIENTED_EDGE ( 'NONE', *, *, #17674, .F. ) ;
#43632 = DIRECTION ( 'NONE',  ( -1.000000000000000000, -0.000000000000000000, 0.000000000000000000 ) ) ;
#43633 = CIRCLE ( 'NONE', #21741, 31.99999999999998224 ) ;
#43634 = CARTESIAN_POINT ( 'NONE',  ( 10.00000000000000000, 0.000000000000000000, 0.000000000000000000 ) ) ;
#43635 = LINE ( 'NONE', #35808, #25884 ) ;
#43636 = DIRECTION ( 'NONE',  ( -0.000000000000000000, -0.000000000000000000, 1.000000000000000000 ) ) ;
#43637 = ORIENTED_EDGE ( 'NONE', *, *, #11406, .F. ) ;
#43638 = DIRECTION ( 'NONE',  ( 0.000000000000000000, -0.9876883405951393247, 0.1564344650402207382 ) ) ;
#43639 = DIRECTION ( 'NONE',  ( 1.000000000000000000, 0.000000000000000000, 0.000000000000000000 ) ) ;
#43640 = CARTESIAN_POINT ( 'NONE',  ( 0.000000000000000000, 0.000000000000000000, 0.000000000000000000 ) ) ;
#43641 = FACE_OUTER_BOUND ( 'NONE', #42279, .T. ) ;
#43642 = ORIENTED_EDGE ( 'NONE', *, *, #18152, .F. ) ;
#43643 = DIRECTION ( 'NONE',  ( 1.000000000000000000, 0.000000000000000000, 0.000000000000000000 ) ) ;
#43644 = DIRECTION ( 'NONE',  ( -1.000000000000000000, -0.000000000000000000, -0.000000000000000000 ) ) ;
#43645 = AXIS2_PLACEMENT_3D ( 'NONE', #15005, #11342, #26501 ) ;
#43646 = ORIENTED_EDGE ( 'NONE', *, *, #25614, .F. ) ;
#43647 = VECTOR ( 'NONE', #45191, 1000.000000000000227 ) ;
#43648 = VERTEX_POINT ( 'NONE', #19058 ) ;
#43649 = EDGE_CURVE ( 'NONE', #41886, #45830, #48005, .T. ) ;
#43650 = DIRECTION ( 'NONE',  ( 0.000000000000000000, 0.000000000000000000, 1.000000000000000000 ) ) ;
#43651 = EDGE_LOOP ( 'NONE', ( #29649, #4004, #22633, #17517 ) ) ;
#43652 = DIRECTION ( 'NONE',  ( -1.000000000000000000, 0.000000000000000000, 0.000000000000000000 ) ) ;
#43653 = EDGE_CURVE ( 'NONE', #40145, #11579, #46455, .T. ) ;
#43654 = CARTESIAN_POINT ( 'NONE',  ( 11.99999999999999822, -76.66974797899844418, 11.30684508768314522 ) ) ;
#43655 = EDGE_CURVE ( 'NONE', #10143, #270, #21423, .T. ) ;
#43656 = VERTEX_POINT ( 'NONE', #34226 ) ;
#43657 = VERTEX_POINT ( 'NONE', #4399 ) ;
#43658 = CARTESIAN_POINT ( 'NONE',  ( 0.000000000000000000, 41.81611651403861885, 3.925862922256313503 ) ) ;
#43659 = ORIENTED_EDGE ( 'NONE', *, *, #32978, .F. ) ;
#43660 = ORIENTED_EDGE ( 'NONE', *, *, #31435, .T. ) ;
#43661 = AXIS2_PLACEMENT_3D ( 'NONE', #15079, #26339, #41272 ) ;
#43662 = ORIENTED_EDGE ( 'NONE', *, *, #629, .T. ) ;
#43663 = EDGE_CURVE ( 'NONE', #28709, #39014, #11248, .T. ) ;
#43664 = ADVANCED_FACE ( 'NONE', ( #208 ), #45255, .T. ) ;
#43665 = CARTESIAN_POINT ( 'NONE',  ( 10.00000000000000000, 56.15606465355042332, -59.75363087400016582 ) ) ;
#43666 = ORIENTED_EDGE ( 'NONE', *, *, #26749, .T. ) ;
#43667 = EDGE_CURVE ( 'NONE', #44212, #47865, #29258, .T. ) ;
#43668 = DIRECTION ( 'NONE',  ( 0.000000000000000000, 0.000000000000000000, -1.000000000000000000 ) ) ;
#43669 = DIRECTION ( 'NONE',  ( 0.000000000000000000, 0.9876883405951371042, 0.1564344650402346437 ) ) ;
#43670 = ORIENTED_EDGE ( 'NONE', *, *, #37714, .T. ) ;
#43671 = DIRECTION ( 'NONE',  ( 0.000000000000000000, 0.3090169943749412340, 0.9510565162951556406 ) ) ;
#43672 = CARTESIAN_POINT ( 'NONE',  ( 0.000000000000000000, 8.830959090343430518, -74.65491531819107252 ) ) ;
#43673 = CARTESIAN_POINT ( 'NONE',  ( 22.94323693612312809, -114.6983135802921083, 5.500000000000000000 ) ) ;
#43674 = CARTESIAN_POINT ( 'NONE',  ( 0.000000000000000000, 0.000000000000000000, 0.000000000000000000 ) ) ;
#43675 = DIRECTION ( 'NONE',  ( 0.000000000000000000, 0.000000000000000000, 1.000000000000000000 ) ) ;
#43676 = EDGE_CURVE ( 'NONE', #13460, #1544, #33171, .T. ) ;
#43677 = ORIENTED_EDGE ( 'NONE', *, *, #2526, .F. ) ;
#43678 = CARTESIAN_POINT ( 'NONE',  ( -6.880223345695647197, -142.5202692415819854, -2.500000000000000000 ) ) ;
#43679 = ORIENTED_EDGE ( 'NONE', *, *, #46356, .T. ) ;
#43680 = VERTEX_POINT ( 'NONE', #11971 ) ;
#43681 = CARTESIAN_POINT ( 'NONE',  ( 11.99999999999999822, 77.49459641780886443, -0.8261519478433960728 ) ) ;
#43682 = CARTESIAN_POINT ( 'NONE',  ( 12.00000000000000000, 26.50000000000000355, -1.500000000000000000 ) ) ;
#43683 = CARTESIAN_POINT ( 'NONE',  ( 0.000000000000000000, 0.000000000000000000, 52.00000000000002132 ) ) ;
#43684 = CARTESIAN_POINT ( 'NONE',  ( 11.99999999999999822, 46.53671651293948486, 59.03961581697416250 ) ) ;
#43685 = CARTESIAN_POINT ( 'NONE',  ( 0.000000000000000000, -4.992566952385247170, 37.16516213103275845 ) ) ;
#43686 = CARTESIAN_POINT ( 'NONE',  ( 0.000000000000000000, -29.81001611431024045, 22.74946021919122430 ) ) ;
#43687 = DIRECTION ( 'NONE',  ( 1.000000000000000000, 0.000000000000000000, 0.000000000000000000 ) ) ;
#43688 = DIRECTION ( 'NONE',  ( -1.000000000000000000, -0.000000000000000000, 0.000000000000000000 ) ) ;
#43689 = LINE ( 'NONE', #9670, #16575 ) ;
#43690 = CARTESIAN_POINT ( 'NONE',  ( 15.00000000000000000, 0.000000000000000000, 0.000000000000000000 ) ) ;
#43691 = VERTEX_POINT ( 'NONE', #26903 ) ;
#43692 = VECTOR ( 'NONE', #45230, 1000.000000000000000 ) ;
#43693 = DIRECTION ( 'NONE',  ( -1.000000000000000000, 0.000000000000000000, 0.000000000000000000 ) ) ;
#43694 = AXIS2_PLACEMENT_3D ( 'NONE', #34732, #16155, #13913 ) ;
#43695 = DIRECTION ( 'NONE',  ( -1.000000000000000000, -0.000000000000000000, -0.000000000000000000 ) ) ;
#43696 = DIRECTION ( 'NONE',  ( -1.000000000000000000, -0.000000000000000000, -0.000000000000000000 ) ) ;
#43697 = AXIS2_PLACEMENT_3D ( 'NONE', #47101, #14051, #21642 ) ;
#43698 = DIRECTION ( 'NONE',  ( 0.000000000000000000, 0.000000000000000000, 1.000000000000000000 ) ) ;
#43699 = CARTESIAN_POINT ( 'NONE',  ( 0.000000000000000000, 0.000000000000000000, 0.000000000000000000 ) ) ;
#43700 = CARTESIAN_POINT ( 'NONE',  ( 0.000000000000000000, 35.38097989696528600, -12.42422080174602605 ) ) ;
#43701 = ORIENTED_EDGE ( 'NONE', *, *, #22873, .F. ) ;
#43702 = EDGE_CURVE ( 'NONE', #26319, #14647, #39436, .T. ) ;
#43703 = CARTESIAN_POINT ( 'NONE',  ( -10.00000000000000000, 0.000000000000000000, 0.000000000000000000 ) ) ;
#43704 =( GEOMETRIC_REPRESENTATION_CONTEXT ( 3 ) GLOBAL_UNCERTAINTY_ASSIGNED_CONTEXT ( ( #11514 ) ) GLOBAL_UNIT_ASSIGNED_CONTEXT ( ( #31811, #5358, #20767 ) ) REPRESENTATION_CONTEXT ( 'NONE', 'WORKASPACE' ) );
#43705 = ADVANCED_FACE ( 'NONE', ( #7803 ), #18584, .T. ) ;
#43706 = PRODUCT_DEFINITION_SHAPE ( 'NONE', 'NONE',  #1121 ) ;
#43707 = EDGE_CURVE ( 'NONE', #32864, #3407, #18275, .T. ) ;
#43708 = DIRECTION ( 'NONE',  ( 0.000000000000000000, 0.000000000000000000, 1.000000000000000000 ) ) ;
#43709 = EDGE_CURVE ( 'NONE', #21451, #30509, #34728, .T. ) ;
#43710 = EDGE_LOOP ( 'NONE', ( #31599, #37661 ) ) ;
#43711 = ORIENTED_EDGE ( 'NONE', *, *, #2987, .T. ) ;
#43712 = PRESENTATION_LAYER_ASSIGNMENT (  '', '', ( #16359 ) ) ;
#43713 = EDGE_CURVE ( 'NONE', #11050, #45431, #19116, .T. ) ;
#43714 = ADVANCED_FACE ( 'NONE', ( #10426 ), #6764, .F. ) ;
#43715 = ORIENTED_EDGE ( 'NONE', *, *, #42204, .T. ) ;
#43716 = ORIENTED_EDGE ( 'NONE', *, *, #38304, .F. ) ;
#43717 = DIRECTION ( 'NONE',  ( -1.000000000000000000, -0.000000000000000000, -0.000000000000000000 ) ) ;
#43718 = ORIENTED_EDGE ( 'NONE', *, *, #8552, .T. ) ;
#43719 = ORIENTED_EDGE ( 'NONE', *, *, #31077, .T. ) ;
#43720 = AXIS2_PLACEMENT_3D ( 'NONE', #42624, #47006, #31612 ) ;
#43721 = AXIS2_PLACEMENT_3D ( 'NONE', #40053, #3311, #40533 ) ;
#43722 = ADVANCED_FACE ( 'NONE', ( #39394 ), #44677, .F. ) ;
#43723 = DIRECTION ( 'NONE',  ( -1.000000000000000000, -0.000000000000000000, -0.000000000000000000 ) ) ;
#43725 = ORIENTED_EDGE ( 'NONE', *, *, #1233, .T. ) ;
#43724 = DIRECTION ( 'NONE',  ( -1.000000000000000000, 0.000000000000000000, 0.000000000000000000 ) ) ;
#43726 = AXIS2_PLACEMENT_3D ( 'NONE', #9697, #36600, #21188 ) ;
#43727 = ORIENTED_EDGE ( 'NONE', *, *, #35148, .T. ) ;
#43728 = CARTESIAN_POINT ( 'NONE',  ( 5.000000000000002665, -81.90746397400393164, 3.894527615417586741 ) ) ;
#43729 = VERTEX_POINT ( 'NONE', #48349 ) ;
#43730 = ORIENTED_EDGE ( 'NONE', *, *, #38676, .T. ) ;
#43731 = CYLINDRICAL_SURFACE ( 'NONE', #22526, 82.00000000000000000 ) ;
#43732 = DIRECTION ( 'NONE',  ( 0.000000000000000000, 0.000000000000000000, 1.000000000000000000 ) ) ;
#43733 = EDGE_CURVE ( 'NONE', #41791, #40361, #18496, .T. ) ;
#43734 = DIRECTION ( 'NONE',  ( 0.000000000000000000, 0.000000000000000000, 1.000000000000000000 ) ) ;
#43735 = ORIENTED_EDGE ( 'NONE', *, *, #15923, .T. ) ;
#43736 = ORIENTED_EDGE ( 'NONE', *, *, #16923, .F. ) ;
#43737 = CIRCLE ( 'NONE', #10124, 42.00000000000000000 ) ;
#43738 = PLANE ( 'NONE',  #9875 ) ;
#43739 = ORIENTED_EDGE ( 'NONE', *, *, #9219, .F. ) ;
#43740 = CARTESIAN_POINT ( 'NONE',  ( 0.000000000000000000, -74.65491531819124305, 8.830959090342128448 ) ) ;
#43741 = LINE ( 'NONE', #10933, #15882 ) ;
#43742 = DIRECTION ( 'NONE',  ( 0.000000000000000000, 0.8910065241883656784, 0.4539904997395510788 ) ) ;
#43743 = DIRECTION ( 'NONE',  ( 0.000000000000000000, 0.000000000000000000, 1.000000000000000000 ) ) ;
#43744 = SURFACE_SIDE_STYLE ('',( #47419 ) ) ;
#43745 = ADVANCED_FACE ( 'NONE', ( #24450 ), #6518, .T. ) ;
#43746 = CYLINDRICAL_SURFACE ( 'NONE', #23557, 16.00000000000000000 ) ;
#43747 = ORIENTED_EDGE ( 'NONE', *, *, #22697, .T. ) ;
#43748 = FACE_OUTER_BOUND ( 'NONE', #37877, .T. ) ;
#43749 = ORIENTED_EDGE ( 'NONE', *, *, #24386, .T. ) ;
#43750 = DIRECTION ( 'NONE',  ( 0.000000000000000000, 0.7604059656000277112, 0.6494480483301875440 ) ) ;
#43751 = CARTESIAN_POINT ( 'NONE',  ( 10.00000000000000000, -50.95692526931372157, 58.39081064771733054 ) ) ;
#43752 = FACE_OUTER_BOUND ( 'NONE', #29454, .T. ) ;
#43753 = CYLINDRICAL_SURFACE ( 'NONE', #44302, 77.49899999999999523 ) ;
#43754 = CARTESIAN_POINT ( 'NONE',  ( 10.00000000000000000, 65.58780272294076497, 36.73666225445916211 ) ) ;
#43755 = EDGE_CURVE ( 'NONE', #15196, #13603, #25346, .T. ) ;
#43756 = AXIS2_PLACEMENT_3D ( 'NONE', #11734, #22739, #30342 ) ;
#43757 = ORIENTED_EDGE ( 'NONE', *, *, #2133, .T. ) ;
#43758 = DIRECTION ( 'NONE',  ( 0.000000000000000000, -0.7604059656000369261, 0.6494480483301766638 ) ) ;
#43759 = LINE ( 'NONE', #21005, #12183 ) ;
#43760 = ADVANCED_FACE ( 'NONE', ( #22417 ), #13204, .T. ) ;
#43761 = AXIS2_PLACEMENT_3D ( 'NONE', #32468, #47396, #29271 ) ;
#43762 = DIRECTION ( 'NONE',  ( 0.000000000000000000, -0.7604059656000228262, -0.6494480483301932061 ) ) ;
#43763 = EDGE_CURVE ( 'NONE', #47615, #8515, #2839, .T. ) ;
#43764 = ADVANCED_FACE ( 'NONE', ( #3066 ), #32932, .T. ) ;
#43765 = ORIENTED_EDGE ( 'NONE', *, *, #170, .T. ) ;
#43766 = ORIENTED_EDGE ( 'NONE', *, *, #24042, .T. ) ;
#43767 = ORIENTED_EDGE ( 'NONE', *, *, #43508, .F. ) ;
#43768 = CIRCLE ( 'NONE', #1574, 31.99999999999998579 ) ;
#43769 = EDGE_CURVE ( 'NONE', #11292, #20770, #26963, .T. ) ;
#43770 = FACE_OUTER_BOUND ( 'NONE', #12778, .T. ) ;
#43771 = CARTESIAN_POINT ( 'NONE',  ( 15.00000000000000000, 24.81905959214260804, -9.408202855044828894 ) ) ;
#43772 = ORIENTED_EDGE ( 'NONE', *, *, #38071, .F. ) ;
#43773 = DIRECTION ( 'NONE',  ( 1.000000000000000000, -0.000000000000000000, -0.000000000000000000 ) ) ;
#43774 = ORIENTED_EDGE ( 'NONE', *, *, #12280, .F. ) ;
#43775 = EDGE_LOOP ( 'NONE', ( #40920, #40338, #45524, #89 ) ) ;
#43776 = ORIENTED_EDGE ( 'NONE', *, *, #9125, .T. ) ;
#43777 = VERTEX_POINT ( 'NONE', #21444 ) ;
#43778 = AXIS2_PLACEMENT_3D ( 'NONE', #4057, #30255, #30483 ) ;
#43779 = DIRECTION ( 'NONE',  ( -1.000000000000000000, 0.000000000000000000, 0.000000000000000000 ) ) ;
#43780 = ORIENTED_EDGE ( 'NONE', *, *, #29700, .F. ) ;
#43782 = ORIENTED_EDGE ( 'NONE', *, *, #9945, .T. ) ;
#43781 = AXIS2_PLACEMENT_3D ( 'NONE', #25475, #36009, #43378 ) ;
#43783 = FACE_OUTER_BOUND ( 'NONE', #45585, .T. ) ;
#43784 = ORIENTED_EDGE ( 'NONE', *, *, #44263, .F. ) ;
#43785 = CARTESIAN_POINT ( 'NONE',  ( 11.99999999999999822, -59.03961581697367933, -46.53671651294010303 ) ) ;
#43786 = AXIS2_PLACEMENT_3D ( 'NONE', #18205, #33151, #39784 ) ;
#43787 = CIRCLE ( 'NONE', #22688, 77.49899999999999523 ) ;
#43788 = CARTESIAN_POINT ( 'NONE',  ( 11.99999999999999822, 59.75363087400075557, 56.15606465354979093 ) ) ;
#43789 = CARTESIAN_POINT ( 'NONE',  ( 0.000000000000000000, -22.90783923731575911, -78.73519480814978522 ) ) ;
#43790 = VERTEX_POINT ( 'NONE', #36378 ) ;
#43791 = CIRCLE ( 'NONE', #41467, 12.49999999999999822 ) ;
#43792 = CYLINDRICAL_SURFACE ( 'NONE', #7901, 31.99999999999998579 ) ;
#43793 = ORIENTED_EDGE ( 'NONE', *, *, #39997, .T. ) ;
#43794 = AXIS2_PLACEMENT_3D ( 'NONE', #29237, #32436, #22125 ) ;
#43795 = CARTESIAN_POINT ( 'NONE',  ( -12.49999999999999645, 0.000000000000000000, 40.80000000000001847 ) ) ;
#43796 = CARTESIAN_POINT ( 'NONE',  ( -20.30386590532152979, -102.9045904027214959, 5.500000000000000000 ) ) ;
#43797 = ORIENTED_EDGE ( 'NONE', *, *, #1264, .F. ) ;
#43798 = CIRCLE ( 'NONE', #21914, 11.59999999999999787 ) ;
#43799 = ORIENTED_EDGE ( 'NONE', *, *, #44924, .F. ) ;
#43800 = DIRECTION ( 'NONE',  ( 1.000000000000000000, 0.000000000000000000, -0.000000000000000000 ) ) ;
#43801 = CARTESIAN_POINT ( 'NONE',  ( 0.000000000000000000, -71.91182617369207719, 28.89263327155721228 ) ) ;
#43802 = VERTEX_POINT ( 'NONE', #32694 ) ;
#43803 = VERTEX_POINT ( 'NONE', #3308 ) ;
#43804 = CARTESIAN_POINT ( 'NONE',  ( 18.80329974962065265, -105.8248132807389084, -5.500000000000000000 ) ) ;
#43805 = CARTESIAN_POINT ( 'NONE',  ( 0.000000000000000000, -27.74655509720617275, -77.16300072079690153 ) ) ;
#43806 = PLANE ( 'NONE',  #39379 ) ;
#43807 = CARTESIAN_POINT ( 'NONE',  ( 11.99999999999999822, 2.543863470249544623, -81.96053171279901051 ) ) ;
#43808 = DIRECTION ( 'NONE',  ( 1.000000000000000000, 0.000000000000000000, 0.000000000000000000 ) ) ;
#43809 = CARTESIAN_POINT ( 'NONE',  ( 10.00000000000000178, 0.000000000000000000, 0.000000000000000000 ) ) ;
#43810 = DIRECTION ( 'NONE',  ( -1.000000000000000000, 0.000000000000000000, 0.000000000000000000 ) ) ;
#43811 = EDGE_CURVE ( 'NONE', #25213, #22663, #29276, .T. ) ;
#43812 = CARTESIAN_POINT ( 'NONE',  ( 15.00000000000000000, -26.23277895567245466, 4.042438405570107918 ) ) ;
#43813 = CARTESIAN_POINT ( 'NONE',  ( -11.99999999999999645, 0.000000000000000000, -13.90444123027096879 ) ) ;
#43814 = DIRECTION ( 'NONE',  ( 0.000000000000000000, 0.9969173337331281859, -0.07845909572784168229 ) ) ;
#43815 = ADVANCED_FACE ( 'NONE', ( #29516 ), #44206, .F. ) ;
#43816 = DIRECTION ( 'NONE',  ( 0.000000000000000000, 0.000000000000000000, -1.000000000000000000 ) ) ;
#43817 = ORIENTED_EDGE ( 'NONE', *, *, #9626, .T. ) ;
#43818 = EDGE_CURVE ( 'NONE', #28645, #38352, #25590, .T. ) ;
#43819 = VERTEX_POINT ( 'NONE', #33186 ) ;
#43820 = CIRCLE ( 'NONE', #24288, 82.00000000000000000 ) ;
#43821 = CIRCLE ( 'NONE', #39955, 31.99999999999998579 ) ;
#43822 = FACE_OUTER_BOUND ( 'NONE', #28734, .T. ) ;
#43823 = EDGE_CURVE ( 'NONE', #24762, #923, #48113, .T. ) ;
#43824 = VECTOR ( 'NONE', #29428, 1000.000000000000000 ) ;
#43825 = VECTOR ( 'NONE', #44020, 1000.000000000000000 ) ;
#43826 = EDGE_CURVE ( 'NONE', #41225, #14780, #33956, .T. ) ;
#43827 = CARTESIAN_POINT ( 'NONE',  ( 5.000000000000000000, 22.48208911017500355, 35.47612816024530957 ) ) ;
#43828 = ORIENTED_EDGE ( 'NONE', *, *, #23601, .F. ) ;
#43829 = VECTOR ( 'NONE', #14249, 1000.000000000000000 ) ;
#43830 = ORIENTED_EDGE ( 'NONE', *, *, #40716, .T. ) ;
#43831 = PRESENTATION_LAYER_ASSIGNMENT (  '', '', ( #25064 ) ) ;
#43832 = DIRECTION ( 'NONE',  ( 0.000000000000000000, 0.9876883405951383255, -0.1564344650402276216 ) ) ;
#43833 = VERTEX_POINT ( 'NONE', #15791 ) ;
#43834 = LINE ( 'NONE', #29623, #29994 ) ;
#43835 = ORIENTED_EDGE ( 'NONE', *, *, #19197, .F. ) ;
#43836 = DIRECTION ( 'NONE',  ( 0.000000000000000000, 0.000000000000000000, 1.000000000000000000 ) ) ;
#43837 = EDGE_CURVE ( 'NONE', #14170, #43657, #2686, .T. ) ;
#43838 = ORIENTED_EDGE ( 'NONE', *, *, #22823, .F. ) ;
#43839 = FACE_OUTER_BOUND ( 'NONE', #22288, .T. ) ;
#43840 = DIRECTION ( 'NONE',  ( 0.000000000000000000, -0.000000000000000000, 1.000000000000000000 ) ) ;
#43841 = CARTESIAN_POINT ( 'NONE',  ( -22.53294031248081808, -134.0273518838794757, -2.500000000000000000 ) ) ;
#43842 = ORIENTED_EDGE ( 'NONE', *, *, #3235, .T. ) ;
#43843 = LINE ( 'NONE', #36258, #44970 ) ;
#43844 = VERTEX_POINT ( 'NONE', #27060 ) ;
#43845 = FACE_OUTER_BOUND ( 'NONE', #1978, .T. ) ;
#43846 = DIRECTION ( 'NONE',  ( -1.000000000000000000, 0.000000000000000000, -0.000000000000000000 ) ) ;
#43847 = DIRECTION ( 'NONE',  ( -0.4999999999999919509, -0.8660254037844432595, 0.000000000000000000 ) ) ;
#43848 = ADVANCED_FACE ( 'NONE', ( #19678 ), #16040, .T. ) ;
#43849 = VECTOR ( 'NONE', #42133, 1000.000000000000000 ) ;
#43850 = DIRECTION ( 'NONE',  ( 0.000000000000000000, 0.000000000000000000, 1.000000000000000000 ) ) ;
#43851 = EDGE_CURVE ( 'NONE', #9070, #1962, #10530, .T. ) ;
#43852 = CARTESIAN_POINT ( 'NONE',  ( 10.00000000000000000, 35.95386929396241271, 10.96151621346552751 ) ) ;
#43853 = VERTEX_POINT ( 'NONE', #847 ) ;
#43854 = AXIS2_PLACEMENT_3D ( 'NONE', #25114, #28567, #40064 ) ;
#43855 = CARTESIAN_POINT ( 'NONE',  ( 0.000000000000000000, -16.65972982744876774, -80.28980883073775487 ) ) ;
#43856 = ORIENTED_EDGE ( 'NONE', *, *, #18687, .F. ) ;
#43857 = ORIENTED_EDGE ( 'NONE', *, *, #2245, .F. ) ;
#43858 = CARTESIAN_POINT ( 'NONE',  ( 0.000000000000000000, 0.000000000000000000, 0.000000000000000000 ) ) ;
#43859 = CARTESIAN_POINT ( 'NONE',  ( 15.00000000000000000, 8.688484142254226938, 21.88630264137359305 ) ) ;
#43860 = AXIS2_PLACEMENT_3D ( 'NONE', #44701, #400, #18984 ) ;
#43861 = ORIENTED_EDGE ( 'NONE', *, *, #12945, .F. ) ;
#43862 = AXIS2_PLACEMENT_3D ( 'NONE', #22483, #11479, #15392 ) ;
#43863 = EDGE_CURVE ( 'NONE', #9209, #29936, #8441, .T. ) ;
#43864 = DIRECTION ( 'NONE',  ( 0.000000000000000000, -0.9238795325112906243, 0.3826834323650805669 ) ) ;
#43865 = CYLINDRICAL_SURFACE ( 'NONE', #43042, 10.00000000000000178 ) ;
#43866 = CARTESIAN_POINT ( 'NONE',  ( -17.09243336300205129, -103.8724235629982502, -2.500000000000000000 ) ) ;
#43867 = VERTEX_POINT ( 'NONE', #12140 ) ;
#43868 = ADVANCED_FACE ( 'NONE', ( #23367 ), #38302, .T. ) ;
#43869 = DIRECTION ( 'NONE',  ( 0.000000000000000000, 0.000000000000000000, -1.000000000000000000 ) ) ;
#43870 = CARTESIAN_POINT ( 'NONE',  ( 14.09999999999999964, 0.000000000000000000, -1.199999999999999956 ) ) ;
#43871 = AXIS2_PLACEMENT_3D ( 'NONE', #29656, #40925, #22328 ) ;
#43872 = DIRECTION ( 'NONE',  ( 0.000000000000000000, 0.9876883405951372152, 0.1564344650402347547 ) ) ;
#43873 = ORIENTED_EDGE ( 'NONE', *, *, #11174, .T. ) ;
#43874 = VECTOR ( 'NONE', #38581, 1000.000000000000000 ) ;
#43875 = CARTESIAN_POINT ( 'NONE',  ( 10.00000000000000000, 0.000000000000000000, 0.000000000000000000 ) ) ;
#43876 = DIRECTION ( 'NONE',  ( 0.000000000000000000, 0.000000000000000000, 1.000000000000000000 ) ) ;
#43877 = DIRECTION ( 'NONE',  ( -0.000000000000000000, -0.000000000000000000, -1.000000000000000000 ) ) ;
#43878 = CARTESIAN_POINT ( 'NONE',  ( -3.000000000000000000, -22.32062822937469804, -14.36278369418829826 ) ) ;
#43879 = DIRECTION ( 'NONE',  ( -1.000000000000000000, 0.000000000000000000, 0.000000000000000000 ) ) ;
#43880 = DIRECTION ( 'NONE',  ( 1.000000000000000000, -0.000000000000000000, 0.000000000000000000 ) ) ;
#43881 = EDGE_CURVE ( 'NONE', #11259, #17933, #45647, .T. ) ;
#43882 = DIRECTION ( 'NONE',  ( -1.000000000000000000, -0.000000000000000000, 0.000000000000000000 ) ) ;
#43883 = EDGE_CURVE ( 'NONE', #13636, #45738, #11637, .T. ) ;
#43884 = ORIENTED_EDGE ( 'NONE', *, *, #16223, .F. ) ;
#43885 = EDGE_CURVE ( 'NONE', #34724, #37662, #15547, .T. ) ;
#43886 = VERTEX_POINT ( 'NONE', #34144 ) ;
#43887 = DIRECTION ( 'NONE',  ( 0.000000000000000000, 0.000000000000000000, 1.000000000000000000 ) ) ;
#43888 = VERTEX_POINT ( 'NONE', #33655 ) ;
#43889 = FACE_OUTER_BOUND ( 'NONE', #35534, .T. ) ;
#43890 = FILL_AREA_STYLE_COLOUR ( '', #37386 ) ;
#43891 = ORIENTED_EDGE ( 'NONE', *, *, #35294, .F. ) ;
#43892 = DIRECTION ( 'NONE',  ( -1.000000000000000000, -0.000000000000000000, -0.000000000000000000 ) ) ;
#43893 = ORIENTED_EDGE ( 'NONE', *, *, #20894, .F. ) ;
#43894 = EDGE_CURVE ( 'NONE', #10618, #11777, #45901, .T. ) ;
#43895 = AXIS2_PLACEMENT_3D ( 'NONE', #4807, #12405, #27825 ) ;
#43896 = VECTOR ( 'NONE', #20192, 1000.000000000000000 ) ;
#43897 = CIRCLE ( 'NONE', #6382, 12.49999999999999822 ) ;
#43898 = CARTESIAN_POINT ( 'NONE',  ( 11.99999999999999822, -2.956366410620109519, -75.11725578898472122 ) ) ;
#43899 = VERTEX_POINT ( 'NONE', #122 ) ;
#43900 = CIRCLE ( 'NONE', #28284, 12.49999999999999645 ) ;
#43901 = CYLINDRICAL_SURFACE ( 'NONE', #36222, 31.99999999999999289 ) ;
#43902 = ORIENTED_EDGE ( 'NONE', *, *, #48330, .F. ) ;
#43903 = DIRECTION ( 'NONE',  ( -1.000000000000000000, 0.000000000000000000, 0.000000000000000000 ) ) ;
#43904 = CARTESIAN_POINT ( 'NONE',  ( -11.59517495878806947, -96.12423995607481686, 5.500000000000000000 ) ) ;
#43905 = VECTOR ( 'NONE', #15674, 1000.000000000000000 ) ;
#43906 = ORIENTED_EDGE ( 'NONE', *, *, #29111, .T. ) ;
#43907 = CARTESIAN_POINT ( 'NONE',  ( 11.99999999999999822, 0.000000000000000000, 0.000000000000000000 ) ) ;
#43908 = ORIENTED_EDGE ( 'NONE', *, *, #38296, .F. ) ;
#43909 = CARTESIAN_POINT ( 'NONE',  ( 0.000000000000000000, -22.67460108101782978, 6.353146135317912169 ) ) ;
#43910 = LINE ( 'NONE', #32428, #12429 ) ;
#43911 = DIRECTION ( 'NONE',  ( 1.000000000000000000, 0.000000000000000000, 0.000000000000000000 ) ) ;
#43912 = ADVANCED_FACE ( 'NONE', ( #4536 ), #42210, .F. ) ;
#43913 = ORIENTED_EDGE ( 'NONE', *, *, #9674, .T. ) ;
#43914 = DIRECTION ( 'NONE',  ( 0.000000000000000000, 0.000000000000000000, -1.000000000000000000 ) ) ;
#43915 = ORIENTED_EDGE ( 'NONE', *, *, #22024, .T. ) ;
#43916 = EDGE_LOOP ( 'NONE', ( #21190, #40201, #7542, #12975 ) ) ;
#43917 = FACE_OUTER_BOUND ( 'NONE', #1617, .T. ) ;
#43918 = ADVANCED_FACE ( 'NONE', ( #15067 ), #26563, .T. ) ;
#43919 = CYLINDRICAL_SURFACE ( 'NONE', #27775, 82.00000000000000000 ) ;
#43920 = CARTESIAN_POINT ( 'NONE',  ( 23.41451323550362318, -132.5004227906269989, -2.500000000000000000 ) ) ;
#43921 = DIRECTION ( 'NONE',  ( 0.000000000000000000, 0.000000000000000000, 1.000000000000000000 ) ) ;
#43922 = ORIENTED_EDGE ( 'NONE', *, *, #31801, .F. ) ;
#43923 = DIRECTION ( 'NONE',  ( -1.000000000000000000, 0.000000000000000000, 0.000000000000000000 ) ) ;
#43924 = EDGE_CURVE ( 'NONE', #20356, #36250, #44138, .T. ) ;
#43925 = DIRECTION ( 'NONE',  ( 0.000000000000000000, -0.7604059656000368150, 0.6494480483301767748 ) ) ;
#43926 = DIRECTION ( 'NONE',  ( 0.000000000000000000, 0.000000000000000000, 1.000000000000000000 ) ) ;
#43927 = AXIS2_PLACEMENT_3D ( 'NONE', #4516, #41716, #15300 ) ;
#43928 = DIRECTION ( 'NONE',  ( -1.000000000000000000, 0.000000000000000000, 0.000000000000000000 ) ) ;
#43929 = CARTESIAN_POINT ( 'NONE',  ( 0.000000000000000000, 51.29473840253317007, -63.97538442413369353 ) ) ;
#43930 = EDGE_LOOP ( 'NONE', ( #29833, #6366, #3469, #6057 ) ) ;
#43931 = DIRECTION ( 'NONE',  ( 0.000000000000000000, 0.9876883405951371042, 0.1564344650402346715 ) ) ;
#43932 = FACE_OUTER_BOUND ( 'NONE', #29755, .T. ) ;
#43933 = CARTESIAN_POINT ( 'NONE',  ( 10.00000000000000000, -24.73286445877757345, 73.44644590900053061 ) ) ;
#43934 = AXIS2_PLACEMENT_3D ( 'NONE', #2807, #47590, #28991 ) ;
#43935 = ADVANCED_FACE ( 'NONE', ( #30477 ), #7950, .T. ) ;
#43936 = ADVANCED_FACE ( 'NONE', ( #8205 ), #7717, .F. ) ;
#43937 = DIRECTION ( 'NONE',  ( 0.000000000000000000, 0.000000000000000000, 1.000000000000000000 ) ) ;
#43938 = VERTEX_POINT ( 'NONE', #9188 ) ;
#43939 = DIRECTION ( 'NONE',  ( -1.000000000000000000, 0.000000000000000000, 0.000000000000000000 ) ) ;
#43940 = DIRECTION ( 'NONE',  ( 0.000000000000000000, -0.9723699203976789995, 0.2334453638558957045 ) ) ;
#43941 = ORIENTED_EDGE ( 'NONE', *, *, #39582, .F. ) ;
#43942 = CARTESIAN_POINT ( 'NONE',  ( 10.00000000000000000, 36.73666225445988687, -65.58780272294035285 ) ) ;
#43943 = AXIS2_PLACEMENT_3D ( 'NONE', #30547, #15396, #11483 ) ;
#43944 = CARTESIAN_POINT ( 'NONE',  ( 0.000000000000000000, -107.5000000000000000, 40.00000000000000711 ) ) ;
#43945 = VERTEX_POINT ( 'NONE', #28521 ) ;
#43946 = ORIENTED_EDGE ( 'NONE', *, *, #3992, .T. ) ;
#43947 = EDGE_CURVE ( 'NONE', #8149, #46255, #1853, .T. ) ;
#43948 = ORIENTED_EDGE ( 'NONE', *, *, #17092, .T. ) ;
#43949 = ORIENTED_EDGE ( 'NONE', *, *, #16829, .F. ) ;
#43950 = AXIS2_PLACEMENT_3D ( 'NONE', #15164, #18806, #26656 ) ;
#43951 = CARTESIAN_POINT ( 'NONE',  ( 6.000000000000000000, -68.55367621811173251, 44.99326035066031437 ) ) ;
#43952 = VERTEX_POINT ( 'NONE', #1606 ) ;
#43953 = ORIENTED_EDGE ( 'NONE', *, *, #29796, .T. ) ;
#43954 = AXIS2_PLACEMENT_3D ( 'NONE', #28479, #46840, #2762 ) ;
#43955 = CIRCLE ( 'NONE', #35359, 82.00000000000000000 ) ;
#43956 = CARTESIAN_POINT ( 'NONE',  ( -3.000000000000000000, 22.07842321921492612, -8.187992925817130896 ) ) ;
#43957 = DIRECTION ( 'NONE',  ( 0.000000000000000000, 0.000000000000000000, 1.000000000000000000 ) ) ;
#43958 = CIRCLE ( 'NONE', #19694, 12.50000000000000000 ) ;
#43959 = CARTESIAN_POINT ( 'NONE',  ( 0.000000000000000000, -56.15606465355000410, 59.75363087400056372 ) ) ;
#43960 = ORIENTED_EDGE ( 'NONE', *, *, #9905, .F. ) ;
#43961 = LINE ( 'NONE', #18004, #24260 ) ;
#43962 = ORIENTED_EDGE ( 'NONE', *, *, #44215, .T. ) ;
#43963 = ORIENTED_EDGE ( 'NONE', *, *, #12620, .T. ) ;
#43964 = AXIS2_PLACEMENT_3D ( 'NONE', #26663, #22507, #41591 ) ;
#43965 = VERTEX_POINT ( 'NONE', #32435 ) ;
#43966 = DIRECTION ( 'NONE',  ( 0.000000000000000000, 0.000000000000000000, 1.000000000000000000 ) ) ;
#43967 = DIRECTION ( 'NONE',  ( -1.000000000000000000, -0.000000000000000000, -0.000000000000000000 ) ) ;
#43968 = CARTESIAN_POINT ( 'NONE',  ( -12.00000000000000000, 2.119128821244579932E-15, 17.30399999999999849 ) ) ;
#43969 = VERTEX_POINT ( 'NONE', #47367 ) ;
#43970 = CIRCLE ( 'NONE', #5682, 77.49899999999999523 ) ;
#43971 = EDGE_LOOP ( 'NONE', ( #22892, #33850, #23531, #17200 ) ) ;
#43972 = EDGE_LOOP ( 'NONE', ( #29412, #19089, #7947, #22434 ) ) ;
#43973 = CARTESIAN_POINT ( 'NONE',  ( 5.999999999999999112, 74.74816331893430288, 33.71516098798768724 ) ) ;
#43974 = VERTEX_POINT ( 'NONE', #20933 ) ;
#43975 = CARTESIAN_POINT ( 'NONE',  ( 15.00000000000000000, -4.261787119645322974, -26.19803753235774835 ) ) ;
#43976 = EDGE_CURVE ( 'NONE', #38352, #23166, #41008, .T. ) ;
#43977 = DIRECTION ( 'NONE',  ( 0.000000000000000000, 0.000000000000000000, 1.000000000000000000 ) ) ;
#43978 = FACE_BOUND ( 'NONE', #24517, .T. ) ;
#43979 = ORIENTED_EDGE ( 'NONE', *, *, #19768, .F. ) ;
#43980 = CARTESIAN_POINT ( 'NONE',  ( 10.00000000000000000, 35.95386929396256903, -10.96151621346501237 ) ) ;
#43981 = DIRECTION ( 'NONE',  ( 0.000000000000000000, 0.000000000000000000, -1.000000000000000000 ) ) ;
#43982 = EDGE_CURVE ( 'NONE', #16743, #4190, #2318, .T. ) ;
#43983 = ADVANCED_FACE ( 'NONE', ( #43458 ), #24839, .F. ) ;
#43984 = DIRECTION ( 'NONE',  ( -1.000000000000000000, 0.000000000000000000, -0.000000000000000000 ) ) ;
#43985 = DIRECTION ( 'NONE',  ( 0.000000000000000000, 0.000000000000000000, -1.000000000000000000 ) ) ;
#43986 = CARTESIAN_POINT ( 'NONE',  ( 15.00000000000000000, 16.61724383029361718, -20.69703378468926402 ) ) ;
#43987 = EDGE_LOOP ( 'NONE', ( #6928, #22898, #2244, #23996 ) ) ;
#43988 = EDGE_CURVE ( 'NONE', #9394, #19028, #13108, .T. ) ;
#43989 = CYLINDRICAL_SURFACE ( 'NONE', #13197, 31.99999999999998579 ) ;
#43990 = VERTEX_POINT ( 'NONE', #17009 ) ;
#43991 = CARTESIAN_POINT ( 'NONE',  ( 11.99999999999999822, 62.50329211542494789, -41.76937507738723099 ) ) ;
#43992 = DIRECTION ( 'NONE',  ( 0.000000000000000000, -0.8910065241883627918, -0.4539904997395567965 ) ) ;
#43993 = AXIS2_PLACEMENT_3D ( 'NONE', #46301, #5198, #20112 ) ;
#43994 = DIRECTION ( 'NONE',  ( -0.6575728627325957421, 0.7533909544171993877, 1.230411769795008318E-16 ) ) ;
#43995 = ADVANCED_FACE ( 'NONE', ( #24350 ), #27808, .T. ) ;
#43996 = DIRECTION ( 'NONE',  ( -0.9580045777625456616, -0.2867529058022021404, 0.000000000000000000 ) ) ;
#43997 = DIRECTION ( 'NONE',  ( 0.000000000000000000, -0.9876883405951361050, -0.1564344650402419989 ) ) ;
#43998 = CIRCLE ( 'NONE', #20538, 82.00000000000000000 ) ;
#43999 = CARTESIAN_POINT ( 'NONE',  ( 0.000000000000000000, 29.81001611431041098, -22.74946021919100403 ) ) ;
#44000 = DIRECTION ( 'NONE',  ( -1.000000000000000000, 0.000000000000000000, 0.000000000000000000 ) ) ;
#44001 = EDGE_CURVE ( 'NONE', #30621, #30136, #13347, .T. ) ;
#44002 = CIRCLE ( 'NONE', #33827, 31.99999999999998579 ) ;
#44003 = CARTESIAN_POINT ( 'NONE',  ( 0.000000000000000000, 0.000000000000000000, 0.000000000000000000 ) ) ;
#44004 = CIRCLE ( 'NONE', #1809, 32.00000000000000000 ) ;
#44005 = EDGE_LOOP ( 'NONE', ( #16617, #21532, #35776, #26711 ) ) ;
#44006 = ORIENTED_EDGE ( 'NONE', *, *, #39186, .T. ) ;
#44007 = VERTEX_POINT ( 'NONE', #43202 ) ;
#44008 = EDGE_CURVE ( 'NONE', #28263, #38490, #24579, .T. ) ;
#44009 = AXIS2_PLACEMENT_3D ( 'NONE', #11847, #19903, #8173 ) ;
#44010 = AXIS2_PLACEMENT_3D ( 'NONE', #34599, #19670, #7941 ) ;
#44011 = DIRECTION ( 'NONE',  ( -1.000000000000000000, 0.000000000000000000, -0.000000000000000000 ) ) ;
#44012 = FACE_OUTER_BOUND ( 'NONE', #46088, .T. ) ;
#44013 = ORIENTED_EDGE ( 'NONE', *, *, #12719, .T. ) ;
#44014 = ORIENTED_EDGE ( 'NONE', *, *, #20898, .T. ) ;
#44015 = EDGE_CURVE ( 'NONE', #45284, #8653, #6615, .T. ) ;
#44016 = CARTESIAN_POINT ( 'NONE',  ( -6.509281303079589520, -14.89695620656361008, -1.199999999999999956 ) ) ;
#44017 = VERTEX_POINT ( 'NONE', #47110 ) ;
#44018 = CIRCLE ( 'NONE', #8835, 82.00000000000000000 ) ;
#44019 = AXIS2_PLACEMENT_3D ( 'NONE', #28350, #39861, #21236 ) ;
#44020 = DIRECTION ( 'NONE',  ( -0.000000000000000000, -0.000000000000000000, -1.000000000000000000 ) ) ;
#44021 = ORIENTED_EDGE ( 'NONE', *, *, #10889, .F. ) ;
#44022 = CARTESIAN_POINT ( 'NONE',  ( 0.000000000000000000, 2.543863470248389103, 81.96053171279903893 ) ) ;
#44023 = VERTEX_POINT ( 'NONE', #42969 ) ;
#44024 = EDGE_CURVE ( 'NONE', #6313, #18399, #6247, .T. ) ;
#44025 = CARTESIAN_POINT ( 'NONE',  ( -1.233757462863590115, -120.8531368722710795, 2.500000000000000000 ) ) ;
#44026 = CIRCLE ( 'NONE', #28376, 0.2999999999999999334 ) ;
#44027 = AXIS2_PLACEMENT_3D ( 'NONE', #38883, #28325, #46460 ) ;
#44028 = ADVANCED_FACE ( 'NONE', ( #17485 ), #5516, .T. ) ;
#44029 = CYLINDRICAL_SURFACE ( 'NONE', #28421, 31.99999999999998579 ) ;
#44030 = DIRECTION ( 'NONE',  ( 8.090853898039828715E-17, -9.269810975720166919E-17, 1.000000000000000000 ) ) ;
#44031 = CIRCLE ( 'NONE', #33104, 31.99999999999998579 ) ;
#44032 = ORIENTED_EDGE ( 'NONE', *, *, #24717, .T. ) ;
#44033 = EDGE_CURVE ( 'NONE', #36090, #20737, #48045, .T. ) ;
#44034 = EDGE_LOOP ( 'NONE', ( #2869, #15399, #29522, #39017 ) ) ;
#44035 = DIRECTION ( 'NONE',  ( 0.000000000000000000, -0.8526401643540860720, -0.5224985647159590130 ) ) ;
#44036 = DIRECTION ( 'NONE',  ( 0.000000000000000000, 0.000000000000000000, 1.000000000000000000 ) ) ;
#44037 = VECTOR ( 'NONE', #39856, 1000.000000000000114 ) ;
#44038 = CIRCLE ( 'NONE', #33110, 82.00000000000000000 ) ;
#44039 = ORIENTED_EDGE ( 'NONE', *, *, #29221, .F. ) ;
#44040 = ORIENTED_EDGE ( 'NONE', *, *, #11954, .F. ) ;
#44041 = EDGE_CURVE ( 'NONE', #6044, #5383, #28491, .T. ) ;
#44042 = AXIS2_PLACEMENT_3D ( 'NONE', #20564, #35017, #27944 ) ;
#44043 = CARTESIAN_POINT ( 'NONE',  ( 0.000000000000000000, -56.15606465354916566, -59.75363087400133111 ) ) ;
#44044 = CARTESIAN_POINT ( 'NONE',  ( 10.00000000000000000, -25.88420570971381807, -27.13269053701123212 ) ) ;
#44045 = ORIENTED_EDGE ( 'NONE', *, *, #23150, .T. ) ;
#44046 = EDGE_LOOP ( 'NONE', ( #34866, #25237, #43419, #31885 ) ) ;
#44047 = AXIS2_PLACEMENT_3D ( 'NONE', #24757, #16444, #2463 ) ;
#44048 = DIRECTION ( 'NONE',  ( 0.000000000000000000, -0.9781476007338043566, 0.2079116908177651712 ) ) ;
#44049 = CARTESIAN_POINT ( 'NONE',  ( 10.00000000000000000, 35.53030884539084866, 12.26510123303271982 ) ) ;
#44050 = CARTESIAN_POINT ( 'NONE',  ( 10.00000000000000000, 71.21200624218852226, -40.65526001592539984 ) ) ;
#44051 = CYLINDRICAL_SURFACE ( 'NONE', #10139, 16.00000000000000000 ) ;
#44052 = AXIS2_PLACEMENT_3D ( 'NONE', #35345, #16512, #32176 ) ;
#44053 = CARTESIAN_POINT ( 'NONE',  ( -12.50000000000000000, -132.5000000000000000, 2.500000000000000000 ) ) ;
#44054 = DIRECTION ( 'NONE',  ( 1.000000000000000000, 0.000000000000000000, 0.000000000000000000 ) ) ;
#44055 = CYLINDRICAL_SURFACE ( 'NONE', #31719, 16.00000000000000000 ) ;
#44056 = FACE_OUTER_BOUND ( 'NONE', #5229, .T. ) ;
#44057 = DIRECTION ( 'NONE',  ( 0.9227826878668540234, 0.3853207896976547087, -0.000000000000000000 ) ) ;
#44058 = DIRECTION ( 'NONE',  ( 0.000000000000000000, -0.9135454576426015327, 0.4067366430757989315 ) ) ;
#44059 = VERTEX_POINT ( 'NONE', #43682 ) ;
#44060 = VERTEX_POINT ( 'NONE', #23878 ) ;
#44061 = AXIS2_PLACEMENT_3D ( 'NONE', #30967, #8909, #38539 ) ;
#44062 = VERTEX_POINT ( 'NONE', #38825 ) ;
#44063 = EDGE_LOOP ( 'NONE', ( #20794, #5297, #17557, #29212 ) ) ;
#44064 = DIRECTION ( 'NONE',  ( 0.000000000000000000, 0.1045284632676459491, -0.9945218953682741780 ) ) ;
#44065 = CIRCLE ( 'NONE', #22961, 82.00000000000000000 ) ;
#44066 = VECTOR ( 'NONE', #30747, 1000.000000000000114 ) ;
#44067 = AXIS2_PLACEMENT_3D ( 'NONE', #32912, #40039, #43940 ) ;
#44068 = CARTESIAN_POINT ( 'NONE',  ( 21.07894319797337701, -103.8699611390234878, 5.500000000000000000 ) ) ;
#44069 = VERTEX_POINT ( 'NONE', #20199 ) ;
#44070 = ORIENTED_EDGE ( 'NONE', *, *, #2529, .T. ) ;
#44071 = CIRCLE ( 'NONE', #3388, 31.99999999999998934 ) ;
#44072 = AXIS2_PLACEMENT_3D ( 'NONE', #5978, #31690, #46841 ) ;
#44073 = VECTOR ( 'NONE', #25671, 1000.000000000000000 ) ;
#44074 = DIRECTION ( 'NONE',  ( -1.000000000000000000, -0.000000000000000000, -0.000000000000000000 ) ) ;
#44075 = CIRCLE ( 'NONE', #16620, 82.00000000000000000 ) ;
#44076 = EDGE_LOOP ( 'NONE', ( #42034, #4541, #838, #13030 ) ) ;
#44077 = DIRECTION ( 'NONE',  ( -1.000000000000000000, -0.000000000000000000, -0.000000000000000000 ) ) ;
#44078 = ORIENTED_EDGE ( 'NONE', *, *, #1759, .F. ) ;
#44079 = DIRECTION ( 'NONE',  ( -0.000000000000000000, -0.000000000000000000, 1.000000000000000000 ) ) ;
#44080 = VECTOR ( 'NONE', #27481, 1000.000000000000000 ) ;
#44081 = DIRECTION ( 'NONE',  ( 0.000000000000000000, 0.000000000000000000, -1.000000000000000000 ) ) ;
#44082 = CARTESIAN_POINT ( 'NONE',  ( 11.99999999999999822, 65.59268652807263322, -36.72794159290169347 ) ) ;
#44083 = ORIENTED_EDGE ( 'NONE', *, *, #12546, .F. ) ;
#44084 = EDGE_CURVE ( 'NONE', #2861, #11520, #12156, .T. ) ;
#44085 = CARTESIAN_POINT ( 'NONE',  ( -3.000000000000002665, 0.000000000000000000, 0.000000000000000000 ) ) ;
#44086 = VERTEX_POINT ( 'NONE', #9418 ) ;
#44087 = DIRECTION ( 'NONE',  ( -0.000000000000000000, -0.000000000000000000, 1.000000000000000000 ) ) ;
#44088 = EDGE_CURVE ( 'NONE', #18357, #25916, #39550, .T. ) ;
#44089 = CARTESIAN_POINT ( 'NONE',  ( 0.000000000000000000, 51.03279382321166224, -55.19960302592011914 ) ) ;
#44090 = ORIENTED_EDGE ( 'NONE', *, *, #33230, .F. ) ;
#44091 = PLANE ( 'NONE',  #45684 ) ;
#44092 = DIRECTION ( 'NONE',  ( 1.000000000000000000, -0.000000000000000000, 0.000000000000000000 ) ) ;
#44093 = DIRECTION ( 'NONE',  ( 0.000000000000000000, 0.000000000000000000, 1.000000000000000000 ) ) ;
#44094 = AXIS2_PLACEMENT_3D ( 'NONE', #16192, #46282, #31122 ) ;
#44095 = DIRECTION ( 'NONE',  ( 0.000000000000000000, 0.6494480483301848794, -0.7604059656000299317 ) ) ;
#44096 = ORIENTED_EDGE ( 'NONE', *, *, #47846, .T. ) ;
#44097 = FACE_OUTER_BOUND ( 'NONE', #31267, .T. ) ;
#44098 = ORIENTED_EDGE ( 'NONE', *, *, #13923, .F. ) ;
#44099 = EDGE_LOOP ( 'NONE', ( #42955, #33612, #3132, #6767 ) ) ;
#44100 = EDGE_CURVE ( 'NONE', #31098, #32136, #41047, .T. ) ;
#44101 = LINE ( 'NONE', #26234, #24433 ) ;
#44102 = AXIS2_PLACEMENT_3D ( 'NONE', #30447, #11846, #41703 ) ;
#44103 = CYLINDRICAL_SURFACE ( 'NONE', #33975, 31.99999999999998579 ) ;
#44104 = ORIENTED_EDGE ( 'NONE', *, *, #6599, .T. ) ;
#44105 = AXIS2_PLACEMENT_3D ( 'NONE', #2338, #31988, #46899 ) ;
#44106 = DIRECTION ( 'NONE',  ( 0.9966891607226786576, 0.08130631524009862554, 0.000000000000000000 ) ) ;
#44107 = ADVANCED_FACE ( 'NONE', ( #29709 ), #3525, .T. ) ;
#44108 = FACE_OUTER_BOUND ( 'NONE', #36850, .T. ) ;
#44109 = CARTESIAN_POINT ( 'NONE',  ( 10.00000000000000000, -69.42325613327415113, -34.44570377933673910 ) ) ;
#44110 = ORIENTED_EDGE ( 'NONE', *, *, #22478, .T. ) ;
#44111 = VECTOR ( 'NONE', #8869, 1000.000000000000000 ) ;
#44112 = FACE_OUTER_BOUND ( 'NONE', #33261, .T. ) ;
#44113 = DIRECTION ( 'NONE',  ( 0.000000000000000000, -1.000000000000000000, -1.301042606982602560E-15 ) ) ;
#44114 = DIRECTION ( 'NONE',  ( 0.3090169943749448977, 0.9510565162951543083, 0.000000000000000000 ) ) ;
#44115 = ORIENTED_EDGE ( 'NONE', *, *, #14519, .F. ) ;
#44116 = VECTOR ( 'NONE', #22300, 1000.000000000000000 ) ;
#44117 = VECTOR ( 'NONE', #10533, 1000.000000000000000 ) ;
#44118 = DIRECTION ( 'NONE',  ( -1.000000000000000000, -0.000000000000000000, 0.000000000000000000 ) ) ;
#44119 = DIRECTION ( 'NONE',  ( -1.000000000000000000, 0.000000000000000000, 0.000000000000000000 ) ) ;
#44121 = AXIS2_PLACEMENT_3D ( 'NONE', #18279, #18032, #41066 ) ;
#44120 = CARTESIAN_POINT ( 'NONE',  ( 11.99999999999999822, -2.946379043146863719, 75.11764819372146462 ) ) ;
#44122 = VECTOR ( 'NONE', #21737, 1000.000000000000000 ) ;
#44123 = EDGE_CURVE ( 'NONE', #27602, #26319, #9757, .T. ) ;
#44124 = ORIENTED_EDGE ( 'NONE', *, *, #42066, .T. ) ;
#44125 = CARTESIAN_POINT ( 'NONE',  ( 0.000000000000000000, 0.000000000000000000, 0.000000000000000000 ) ) ;
#44126 = CARTESIAN_POINT ( 'NONE',  ( -3.000000000000000000, -11.95096189432312350, -23.69967320028773372 ) ) ;
#44127 = CARTESIAN_POINT ( 'NONE',  ( 0.000000000000000000, -73.72996012237429397, -14.67089635893794508 ) ) ;
#44128 = DIRECTION ( 'NONE',  ( 0.000000000000000000, 0.000000000000000000, 1.000000000000000000 ) ) ;
#44129 = VECTOR ( 'NONE', #18749, 1000.000000000000000 ) ;
#44130 = ORIENTED_EDGE ( 'NONE', *, *, #34367, .F. ) ;
#44131 = DIRECTION ( 'NONE',  ( 0.000000000000000000, 0.000000000000000000, 1.000000000000000000 ) ) ;
#44132 = ORIENTED_EDGE ( 'NONE', *, *, #3255, .T. ) ;
#44133 = DIRECTION ( 'NONE',  ( 0.8225049752423776450, 0.5687579148473765889, -0.000000000000000000 ) ) ;
#44134 = PLANE ( 'NONE',  #8856 ) ;
#44135 = EDGE_LOOP ( 'NONE', ( #9705, #15736, #45909, #7989 ) ) ;
#44136 = VECTOR ( 'NONE', #33402, 1000.000000000000000 ) ;
#44137 = EDGE_CURVE ( 'NONE', #1537, #17280, #31697, .T. ) ;
#44138 = CIRCLE ( 'NONE', #23036, 31.99999999999998934 ) ;
#44139 = AXIS2_PLACEMENT_3D ( 'NONE', #29445, #22084, #47550 ) ;
#44140 = ADVANCED_FACE ( 'NONE', ( #7195 ), #43919, .T. ) ;
#44141 = CARTESIAN_POINT ( 'NONE',  ( 10.00000000000000000, -51.02545421589285723, -55.20638768913812555 ) ) ;
#44142 = ORIENTED_EDGE ( 'NONE', *, *, #45302, .F. ) ;
#44143 = EDGE_CURVE ( 'NONE', #13979, #16986, #37304, .T. ) ;
#44144 = AXIS2_PLACEMENT_3D ( 'NONE', #30252, #30984, #19936 ) ;
#44145 = CIRCLE ( 'NONE', #23048, 30.50000000000000000 ) ;
#44146 = DIRECTION ( 'NONE',  ( 0.000000000000000000, -0.2334453638558922628, -0.9723699203976798877 ) ) ;
#44147 = ORIENTED_EDGE ( 'NONE', *, *, #5534, .F. ) ;
#44148 = VECTOR ( 'NONE', #39502, 999.9999999999998863 ) ;
#44149 = DIRECTION ( 'NONE',  ( 0.000000000000000000, 0.8660254037844363761, -0.5000000000000039968 ) ) ;
#44150 = DIRECTION ( 'NONE',  ( -1.000000000000000000, 0.000000000000000000, 0.000000000000000000 ) ) ;
#44151 = EDGE_LOOP ( 'NONE', ( #33386, #46151, #25063, #47558 ) ) ;
#44152 = DIRECTION ( 'NONE',  ( -1.000000000000000000, 0.000000000000000000, -0.000000000000000000 ) ) ;
#44153 = AXIS2_PLACEMENT_3D ( 'NONE', #38449, #45807, #8578 ) ;
#44154 = EDGE_CURVE ( 'NONE', #13155, #17581, #41848, .T. ) ;
#44155 = ORIENTED_EDGE ( 'NONE', *, *, #12143, .T. ) ;
#44156 = EDGE_CURVE ( 'NONE', #31426, #33111, #39513, .T. ) ;
#44157 = ADVANCED_FACE ( 'NONE', ( #44167 ), #33391, .T. ) ;
#44158 = CARTESIAN_POINT ( 'NONE',  ( 10.00000000000000000, -40.65526001592565564, -71.21200624218839437 ) ) ;
#44159 = CARTESIAN_POINT ( 'NONE',  ( 5.000000000000002665, 39.47590169984846398, 71.87247863392428826 ) ) ;
#44160 = FACE_OUTER_BOUND ( 'NONE', #28262, .T. ) ;
#44161 = ORIENTED_EDGE ( 'NONE', *, *, #22149, .T. ) ;
#44162 = CARTESIAN_POINT ( 'NONE',  ( 0.000000000000000000, -0.8828120875898013420, -37.48860685352291711 ) ) ;
#44163 = ORIENTED_EDGE ( 'NONE', *, *, #47137, .F. ) ;
#44164 = ORIENTED_EDGE ( 'NONE', *, *, #4685, .F. ) ;
#44165 =( REPRESENTATION_RELATIONSHIP ('NONE','NONE', #5957, #9091 ) REPRESENTATION_RELATIONSHIP_WITH_TRANSFORMATION ( #43593 )SHAPE_REPRESENTATION_RELATIONSHIP( ) );
#44166 = DIRECTION ( 'NONE',  ( -1.000000000000000000, -0.000000000000000000, -0.000000000000000000 ) ) ;
#44167 = FACE_OUTER_BOUND ( 'NONE', #910, .T. ) ;
#44168 = DIRECTION ( 'NONE',  ( -1.000000000000000000, 0.000000000000000000, 0.000000000000000000 ) ) ;
#44169 = FACE_OUTER_BOUND ( 'NONE', #47464, .T. ) ;
#44170 = VERTEX_POINT ( 'NONE', #6480 ) ;
#44171 = LINE ( 'NONE', #15037, #34660 ) ;
#44172 = DIRECTION ( 'NONE',  ( 0.000000000000000000, 0.000000000000000000, -1.000000000000000000 ) ) ;
#44173 = DIRECTION ( 'NONE',  ( -1.000000000000000000, -0.000000000000000000, 0.000000000000000000 ) ) ;
#44174 = CARTESIAN_POINT ( 'NONE',  ( 0.000000000000000000, -55.20638768913797634, 51.02545421589302777 ) ) ;
#44175 = CIRCLE ( 'NONE', #27771, 37.49900000000000944 ) ;
#44176 = CARTESIAN_POINT ( 'NONE',  ( 15.00000000000000000, 20.85821328998756385, 10.92862929874494249 ) ) ;
#44177 = ORIENTED_EDGE ( 'NONE', *, *, #35320, .T. ) ;
#44178 = CARTESIAN_POINT ( 'NONE',  ( -4.250000000000000000, -13.95926121303099343, -1.199999999999999956 ) ) ;
#44179 = AXIS2_PLACEMENT_3D ( 'NONE', #24607, #5285, #20430 ) ;
#44180 = DIRECTION ( 'NONE',  ( 0.000000000000000000, -0.9723699203976740035, -0.2334453638559160216 ) ) ;
#44181 = CARTESIAN_POINT ( 'NONE',  ( 10.00000000000000178, 1.530808498934191521E-15, -12.50000000000000000 ) ) ;
#44182 = DIRECTION ( 'NONE',  ( 0.000000000000000000, 0.000000000000000000, 1.000000000000000000 ) ) ;
#44183 = CIRCLE ( 'NONE', #1996, 31.99999999999999645 ) ;
#44184 = CIRCLE ( 'NONE', #32482, 32.00000000000000000 ) ;
#44185 = CARTESIAN_POINT ( 'NONE',  ( 12.00000000000000000, 9.615535125378766423, -24.73947219025917121 ) ) ;
#44186 = DIRECTION ( 'NONE',  ( -1.000000000000000000, 0.000000000000000000, -0.000000000000000000 ) ) ;
#44187 = ORIENTED_EDGE ( 'NONE', *, *, #442, .T. ) ;
#44188 = LINE ( 'NONE', #41251, #8997 ) ;
#44189 = AXIS2_PLACEMENT_3D ( 'NONE', #46280, #35741, #43089 ) ;
#44190 = DIRECTION ( 'NONE',  ( -1.000000000000000000, -0.000000000000000000, -0.000000000000000000 ) ) ;
#44191 = CIRCLE ( 'NONE', #9838, 15.39727592608509177 ) ;
#44192 = CIRCLE ( 'NONE', #17630, 16.00000000000000000 ) ;
#44193 = ORIENTED_EDGE ( 'NONE', *, *, #25890, .T. ) ;
#44194 = ORIENTED_EDGE ( 'NONE', *, *, #1148, .T. ) ;
#44195 = EDGE_CURVE ( 'NONE', #48169, #37035, #40017, .T. ) ;
#44197 = ADVANCED_FACE ( 'NONE', ( #3272 ), #29236, .T. ) ;
#44196 = AXIS2_PLACEMENT_3D ( 'NONE', #16142, #14748, #45998 ) ;
#44198 = ORIENTED_EDGE ( 'NONE', *, *, #15266, .T. ) ;
#44199 = EDGE_CURVE ( 'NONE', #1910, #27382, #14476, .T. ) ;
#44200 = AXIS2_PLACEMENT_3D ( 'NONE', #32324, #21053, #10529 ) ;
#44201 = CARTESIAN_POINT ( 'NONE',  ( 0.000000000000000000, 41.76106447765489094, 62.50884508063442269 ) ) ;
#44202 = VERTEX_POINT ( 'NONE', #15033 ) ;
#44203 = EDGE_CURVE ( 'NONE', #15440, #7146, #36808, .T. ) ;
#44204 = ORIENTED_EDGE ( 'NONE', *, *, #9339, .F. ) ;
#44205 = VECTOR ( 'NONE', #34585, 1000.000000000000000 ) ;
#44206 = PLANE ( 'NONE',  #11312 ) ;
#44207 = FACE_OUTER_BOUND ( 'NONE', #23719, .T. ) ;
#44209 = ORIENTED_EDGE ( 'NONE', *, *, #4204, .T. ) ;
#44208 = CARTESIAN_POINT ( 'NONE',  ( 10.00000000000000000, -76.69515212746036070, 29.01471420065537643 ) ) ;
#44210 = EDGE_LOOP ( 'NONE', ( #12721, #38371, #30639, #18545 ) ) ;
#44211 = DIRECTION ( 'NONE',  ( -1.000000000000000000, 0.000000000000000000, 0.000000000000000000 ) ) ;
#44212 = VERTEX_POINT ( 'NONE', #3037 ) ;
#44213 = ORIENTED_EDGE ( 'NONE', *, *, #19375, .F. ) ;
#44214 = VERTEX_POINT ( 'NONE', #18202 ) ;
#44215 = EDGE_CURVE ( 'NONE', #28409, #29152, #33149, .T. ) ;
#44216 = EDGE_CURVE ( 'NONE', #16811, #9223, #44406, .T. ) ;
#44217 = DIRECTION ( 'NONE',  ( 0.9580045777625456616, 0.2867529058022021404, 0.000000000000000000 ) ) ;
#44218 = CARTESIAN_POINT ( 'NONE',  ( 11.99999999999999822, -55.38113227695820484, 54.21277698773656084 ) ) ;
#44219 = DIRECTION ( 'NONE',  ( -1.000000000000000000, -0.000000000000000000, -0.000000000000000000 ) ) ;
#44220 = ORIENTED_EDGE ( 'NONE', *, *, #14369, .F. ) ;
#44221 = EDGE_LOOP ( 'NONE', ( #48450, #31991, #28644, #7652 ) ) ;
#44222 = VERTEX_POINT ( 'NONE', #37056 ) ;
#44223 = CARTESIAN_POINT ( 'NONE',  ( 15.00000000000000000, -20.55727247249748402, -16.78983467731284307 ) ) ;
#44224 = ORIENTED_EDGE ( 'NONE', *, *, #18817, .T. ) ;
#44225 = CARTESIAN_POINT ( 'NONE',  ( -8.637688417678548447, 13.69818742750669749, -55.00000000000000000 ) ) ;
#44226 = CIRCLE ( 'NONE', #23121, 31.99999999999999645 ) ;
#44227 = DIRECTION ( 'NONE',  ( -1.000000000000000000, -0.000000000000000000, 0.000000000000000000 ) ) ;
#44228 = FACE_OUTER_BOUND ( 'NONE', #35200, .T. ) ;
#44229 = ORIENTED_EDGE ( 'NONE', *, *, #47314, .F. ) ;
#44230 = LINE ( 'NONE', #48134, #4174 ) ;
#44231 = LINE ( 'NONE', #10706, #19008 ) ;
#44232 = CIRCLE ( 'NONE', #37199, 82.00000000000000000 ) ;
#44233 = CARTESIAN_POINT ( 'NONE',  ( 11.99999999999999822, 41.19522573413826194, -65.64334221924865176 ) ) ;
#44234 = DIRECTION ( 'NONE',  ( 1.000000000000000000, 0.000000000000000000, 0.000000000000000000 ) ) ;
#44235 = EDGE_CURVE ( 'NONE', #37423, #36132, #48312, .T. ) ;
#44236 = CARTESIAN_POINT ( 'NONE',  ( 0.000000000000000000, 24.81905959214261514, 9.408202855044827118 ) ) ;
#44237 = VERTEX_POINT ( 'NONE', #2798 ) ;
#44238 = CIRCLE ( 'NONE', #24701, 37.49900000000000944 ) ;
#44239 = CARTESIAN_POINT ( 'NONE',  ( -3.000000000000000000, -3.948201729842038432, -23.21447184625298021 ) ) ;
#44240 = CARTESIAN_POINT ( 'NONE',  ( 0.000000000000000000, 0.000000000000000000, 0.000000000000000000 ) ) ;
#44241 = VECTOR ( 'NONE', #47809, 1000.000000000000000 ) ;
#44242 = DIRECTION ( 'NONE',  ( 0.000000000000000000, 0.000000000000000000, 1.000000000000000000 ) ) ;
#44243 = DIRECTION ( 'NONE',  ( 0.000000000000000000, 0.000000000000000000, 1.000000000000000000 ) ) ;
#44244 = CIRCLE ( 'NONE', #26256, 31.99999999999999289 ) ;
#44245 = DIRECTION ( 'NONE',  ( 0.000000000000000000, 0.000000000000000000, 1.000000000000000000 ) ) ;
#44246 = CARTESIAN_POINT ( 'NONE',  ( 10.00000000000000000, 0.000000000000000000, 0.000000000000000000 ) ) ;
#44247 = VECTOR ( 'NONE', #37255, 1000.000000000000000 ) ;
#44248 = DIRECTION ( 'NONE',  ( 0.000000000000000000, 0.000000000000000000, 1.000000000000000000 ) ) ;
#44249 = FACE_OUTER_BOUND ( 'NONE', #40014, .T. ) ;
#44250 = DIRECTION ( 'NONE',  ( -1.000000000000000000, 0.000000000000000000, -0.000000000000000000 ) ) ;
#44251 =( NAMED_UNIT ( * ) SI_UNIT ( $, .STERADIAN. ) SOLID_ANGLE_UNIT ( ) );
#44252 = FACE_OUTER_BOUND ( 'NONE', #41376, .T. ) ;
#44253 = ORIENTED_EDGE ( 'NONE', *, *, #10552, .T. ) ;
#44254 = VERTEX_POINT ( 'NONE', #45867 ) ;
#44255 = CIRCLE ( 'NONE', #30994, 32.00000000000000000 ) ;
#44256 = ORIENTED_EDGE ( 'NONE', *, *, #25125, .T. ) ;
#44257 = ADVANCED_FACE ( 'NONE', ( #26292 ), #45135, .T. ) ;
#44258 = AXIS2_PLACEMENT_3D ( 'NONE', #20634, #43408, #43872 ) ;
#44259 = DIRECTION ( 'NONE',  ( 1.000000000000000000, 0.000000000000000000, 0.000000000000000000 ) ) ;
#44260 = DIRECTION ( 'NONE',  ( 1.000000000000000000, 0.000000000000000000, 0.000000000000000000 ) ) ;
#44261 = ORIENTED_EDGE ( 'NONE', *, *, #1604, .F. ) ;
#44262 = EDGE_CURVE ( 'NONE', #32517, #7731, #12335, .T. ) ;
#44263 = EDGE_CURVE ( 'NONE', #2304, #8879, #34571, .T. ) ;
#44264 = DIRECTION ( 'NONE',  ( -1.000000000000000000, -0.000000000000000000, -0.000000000000000000 ) ) ;
#44265 = ORIENTED_EDGE ( 'NONE', *, *, #43448, .F. ) ;
#44266 = VECTOR ( 'NONE', #33579, 1000.000000000000000 ) ;
#44267 = AXIS2_PLACEMENT_3D ( 'NONE', #44817, #11772, #26703 ) ;
#44268 = ADVANCED_FACE ( 'NONE', ( #41229 ), #809, .T. ) ;
#44269 = CIRCLE ( 'NONE', #15367, 31.99999999999999289 ) ;
#44270 = DIRECTION ( 'NONE',  ( 1.000000000000000000, 0.000000000000000000, 0.000000000000000000 ) ) ;
#44271 = VERTEX_POINT ( 'NONE', #42176 ) ;
#44272 = DIRECTION ( 'NONE',  ( 0.000000000000000000, 0.000000000000000000, 1.000000000000000000 ) ) ;
#44273 = EDGE_CURVE ( 'NONE', #6623, #5626, #1053, .T. ) ;
#44274 = ORIENTED_EDGE ( 'NONE', *, *, #21102, .T. ) ;
#44275 = DIRECTION ( 'NONE',  ( 0.000000000000000000, -0.2334453638559128297, 0.9723699203976748917 ) ) ;
#44276 = CARTESIAN_POINT ( 'NONE',  ( 11.99999999999999822, -73.72996012237449293, 14.67089635893687571 ) ) ;
#44277 = DIRECTION ( 'NONE',  ( -1.000000000000000000, -0.000000000000000000, -0.000000000000000000 ) ) ;
#44278 = ORIENTED_EDGE ( 'NONE', *, *, #28410, .F. ) ;
#44279 = ORIENTED_EDGE ( 'NONE', *, *, #24588, .F. ) ;
#44280 = DIRECTION ( 'NONE',  ( 0.7585478161175716050, 0.6516173805718067369, 0.000000000000000000 ) ) ;
#44281 = EDGE_CURVE ( 'NONE', #10873, #2830, #15751, .T. ) ;
#44282 = DIRECTION ( 'NONE',  ( -1.000000000000000000, -0.000000000000000000, 0.000000000000000000 ) ) ;
#44283 = AXIS2_PLACEMENT_3D ( 'NONE', #14119, #29041, #7734 ) ;
#44284 = ORIENTED_EDGE ( 'NONE', *, *, #38190, .F. ) ;
#44285 = ORIENTED_EDGE ( 'NONE', *, *, #40787, .F. ) ;
#44286 = CARTESIAN_POINT ( 'NONE',  ( 5.000000000000000000, 31.52238457039599595, 27.75498641678753842 ) ) ;
#44287 = DIRECTION ( 'NONE',  ( 0.000000000000000000, 0.07845909572784512398, -0.9969173337331279638 ) ) ;
#44288 = ORIENTED_EDGE ( 'NONE', *, *, #15088, .F. ) ;
#44289 = ORIENTED_EDGE ( 'NONE', *, *, #16677, .F. ) ;
#44290 = LINE ( 'NONE', #3397, #8954 ) ;
#44291 = CIRCLE ( 'NONE', #33358, 31.99999999999999645 ) ;
#44292 = DIRECTION ( 'NONE',  ( 0.000000000000000000, 0.000000000000000000, 1.000000000000000000 ) ) ;
#44293 = CYLINDRICAL_SURFACE ( 'NONE', #38653, 0.5000000000000004441 ) ;
#44294 = DIRECTION ( 'NONE',  ( -0.9580045777625456616, -0.2867529058022021404, 0.000000000000000000 ) ) ;
#44295 = DIRECTION ( 'NONE',  ( 0.000000000000000000, -0.9876883405951393247, 0.1564344650402207104 ) ) ;
#44296 = FACE_OUTER_BOUND ( 'NONE', #44513, .T. ) ;
#44297 = AXIS2_PLACEMENT_3D ( 'NONE', #35919, #9492, #39366 ) ;
#44298 = FACE_OUTER_BOUND ( 'NONE', #20248, .T. ) ;
#44299 = LINE ( 'NONE', #10772, #3526 ) ;
#44300 = CYLINDRICAL_SURFACE ( 'NONE', #5710, 16.00000000000000000 ) ;
#44301 = CARTESIAN_POINT ( 'NONE',  ( 5.000000000000000000, -59.75363087400113926, 56.15606465354937882 ) ) ;
#44302 = AXIS2_PLACEMENT_3D ( 'NONE', #13902, #36414, #6554 ) ;
#44303 = DIRECTION ( 'NONE',  ( 1.000000000000000000, 0.000000000000000000, 0.000000000000000000 ) ) ;
#44304 = LINE ( 'NONE', #40627, #38125 ) ;
#44305 = ORIENTED_EDGE ( 'NONE', *, *, #15905, .T. ) ;
#44306 = ORIENTED_EDGE ( 'NONE', *, *, #42022, .F. ) ;
#44307 = VERTEX_POINT ( 'NONE', #45603 ) ;
#44308 = ORIENTED_EDGE ( 'NONE', *, *, #8671, .T. ) ;
#44309 = CIRCLE ( 'NONE', #12288, 42.00000000000000000 ) ;
#44310 = EDGE_CURVE ( 'NONE', #13250, #27191, #34769, .T. ) ;
#44311 = FACE_OUTER_BOUND ( 'NONE', #6014, .T. ) ;
#44312 = EDGE_CURVE ( 'NONE', #27800, #28663, #30680, .T. ) ;
#44313 = DIRECTION ( 'NONE',  ( 0.000000000000000000, 0.000000000000000000, 1.000000000000000000 ) ) ;
#44314 = ORIENTED_EDGE ( 'NONE', *, *, #6629, .F. ) ;
#44315 = EDGE_CURVE ( 'NONE', #18326, #22246, #44947, .T. ) ;
#44316 = VECTOR ( 'NONE', #14076, 1000.000000000000000 ) ;
#44317 = ORIENTED_EDGE ( 'NONE', *, *, #35238, .T. ) ;
#44318 = CIRCLE ( 'NONE', #27146, 31.99999999999998579 ) ;
#44319 = EDGE_CURVE ( 'NONE', #8938, #29208, #19895, .T. ) ;
#44320 = EDGE_CURVE ( 'NONE', #11204, #14124, #334, .T. ) ;
#44321 = DIRECTION ( 'NONE',  ( -1.000000000000000000, 0.000000000000000000, 0.000000000000000000 ) ) ;
#44322 = EDGE_LOOP ( 'NONE', ( #7108, #28154, #43145, #482 ) ) ;
#44323 = CARTESIAN_POINT ( 'NONE',  ( 0.000000000000000000, -120.0000000000000000, -2.500000000000000000 ) ) ;
#44324 = AXIS2_PLACEMENT_3D ( 'NONE', #478, #38663, #33996 ) ;
#44325 = ORIENTED_EDGE ( 'NONE', *, *, #31749, .T. ) ;
#44326 = FILL_AREA_STYLE_COLOUR ( '', #23490 ) ;
#44327 = DIRECTION ( 'NONE',  ( 0.000000000000000000, 0.000000000000000000, 1.000000000000000000 ) ) ;
#44328 = AXIS2_PLACEMENT_3D ( 'NONE', #34845, #35085, #5472 ) ;
#44329 = ORIENTED_EDGE ( 'NONE', *, *, #21984, .F. ) ;
#44330 = CARTESIAN_POINT ( 'NONE',  ( 0.000000000000000000, 9.188173127307290855, 40.98264845739752360 ) ) ;
#44331 = VERTEX_POINT ( 'NONE', #34106 ) ;
#44332 = LINE ( 'NONE', #3447, #18365 ) ;
#44333 = LINE ( 'NONE', #6888, #33752 ) ;
#44334 = ORIENTED_EDGE ( 'NONE', *, *, #12286, .T. ) ;
#44335 = DIRECTION ( 'NONE',  ( -1.000000000000000000, 0.000000000000000000, -0.000000000000000000 ) ) ;
#44336 = LINE ( 'NONE', #41396, #2828 ) ;
#44337 = AXIS2_PLACEMENT_3D ( 'NONE', #23118, #38054, #18706 ) ;
#44339 = ORIENTED_EDGE ( 'NONE', *, *, #27577, .T. ) ;
#44338 = CARTESIAN_POINT ( 'NONE',  ( 11.99999999999999822, 0.000000000000000000, 0.000000000000000000 ) ) ;
#44340 = EDGE_CURVE ( 'NONE', #7999, #12683, #17577, .T. ) ;
#44341 = DIRECTION ( 'NONE',  ( -1.000000000000000000, 0.000000000000000000, 0.000000000000000000 ) ) ;
#44342 = ORIENTED_EDGE ( 'NONE', *, *, #25455, .F. ) ;
#44343 = CARTESIAN_POINT ( 'NONE',  ( -23.54415474984308787, -120.4156646670583086, 5.500000000000000000 ) ) ;
#44344 = EDGE_LOOP ( 'NONE', ( #35437, #48435, #7396, #29889 ) ) ;
#44345 = ORIENTED_EDGE ( 'NONE', *, *, #35353, .T. ) ;
#44346 = DIRECTION ( 'NONE',  ( 0.000000000000000000, 0.9510565162951521989, 0.3090169943749515591 ) ) ;
#44347 = DIRECTION ( 'NONE',  ( 0.000000000000000000, 0.000000000000000000, -1.000000000000000000 ) ) ;
#44348 = ORIENTED_EDGE ( 'NONE', *, *, #22147, .T. ) ;
#44349 = DIRECTION ( 'NONE',  ( -1.000000000000000000, 0.000000000000000000, -0.000000000000000000 ) ) ;
#44350 = DIRECTION ( 'NONE',  ( -1.000000000000000000, -0.000000000000000000, -0.000000000000000000 ) ) ;
#44351 = CARTESIAN_POINT ( 'NONE',  ( -19.90058851926621131, -132.5883508287165853, -5.500000000000000000 ) ) ;
#44352 = ORIENTED_EDGE ( 'NONE', *, *, #25464, .T. ) ;
#44353 = EDGE_CURVE ( 'NONE', #4138, #2489, #8219, .T. ) ;
#44354 = CARTESIAN_POINT ( 'NONE',  ( -3.000000000000002665, 0.000000000000000000, 0.000000000000000000 ) ) ;
#44355 = LINE ( 'NONE', #21827, #46198 ) ;
#44356 = LINE ( 'NONE', #33342, #42699 ) ;
#44357 = EDGE_CURVE ( 'NONE', #4532, #12258, #18920, .T. ) ;
#44358 = AXIS2_PLACEMENT_3D ( 'NONE', #46095, #27743, #8877 ) ;
#44359 = ORIENTED_EDGE ( 'NONE', *, *, #5652, .T. ) ;
#44360 = DIRECTION ( 'NONE',  ( 0.000000000000000000, 0.000000000000000000, 1.000000000000000000 ) ) ;
#44361 = CARTESIAN_POINT ( 'NONE',  ( 10.00000000000000000, -37.01155633439053361, -6.555932627142825986 ) ) ;
#44362 = CARTESIAN_POINT ( 'NONE',  ( 0.000000000000000000, 40.98264845739763018, -9.188173127306864529 ) ) ;
#44363 = LINE ( 'NONE', #36761, #14584 ) ;
#44364 = VECTOR ( 'NONE', #10223, 1000.000000000000114 ) ;
#44365 = ORIENTED_EDGE ( 'NONE', *, *, #22872, .F. ) ;
#44366 = DIRECTION ( 'NONE',  ( 1.000000000000000000, 0.000000000000000000, 0.000000000000000000 ) ) ;
#44367 = CARTESIAN_POINT ( 'NONE',  ( 10.00000000000000000, -36.72794159290197769, -65.59268652807249111 ) ) ;
#44368 = CARTESIAN_POINT ( 'NONE',  ( 11.99999999999999822, -77.19088730480528682, 6.903761155837505825 ) ) ;
#44369 = FACE_OUTER_BOUND ( 'NONE', #31061, .T. ) ;
#44370 = ORIENTED_EDGE ( 'NONE', *, *, #36639, .F. ) ;
#44371 = ORIENTED_EDGE ( 'NONE', *, *, #28363, .T. ) ;
#44372 = DIRECTION ( 'NONE',  ( 0.000000000000000000, 0.8526401643540935105, -0.5224985647159468005 ) ) ;
#44373 = VECTOR ( 'NONE', #23767, 1000.000000000000000 ) ;
#44374 = ORIENTED_EDGE ( 'NONE', *, *, #800, .T. ) ;
#44375 = ADVANCED_FACE ( 'NONE', ( #37540 ), #8167, .T. ) ;
#44376 = LINE ( 'NONE', #26500, #30716 ) ;
#44377 = CARTESIAN_POINT ( 'NONE',  ( -0.6292498812908471351, 0.7209408956789961076, -45.00000000000000000 ) ) ;
#44378 = EDGE_CURVE ( 'NONE', #25935, #27340, #48090, .T. ) ;
#44379 = CARTESIAN_POINT ( 'NONE',  ( 10.00000000000000000, -12.93880638057369659, 76.41127070299266677 ) ) ;
#44380 = VERTEX_POINT ( 'NONE', #45358 ) ;
#44381 = VECTOR ( 'NONE', #31874, 1000.000000000000000 ) ;
#44382 = EDGE_CURVE ( 'NONE', #45431, #40832, #11841, .T. ) ;
#44383 = CARTESIAN_POINT ( 'NONE',  ( 10.00000000000000000, 16.00000000000000000, -2.500000000000000000 ) ) ;
#44385 = EDGE_CURVE ( 'NONE', #3134, #41559, #38035, .T. ) ;
#44384 = ORIENTED_EDGE ( 'NONE', *, *, #19755, .F. ) ;
#44386 = AXIS2_PLACEMENT_3D ( 'NONE', #29419, #2737, #14491 ) ;
#44387 = CARTESIAN_POINT ( 'NONE',  ( 11.99999999999999822, 50.23322058963442061, -64.81221759200288091 ) ) ;
#44388 = CARTESIAN_POINT ( 'NONE',  ( 10.00000000000000000, 33.80338159004307386, -16.23288003029461279 ) ) ;
#44389 = LINE ( 'NONE', #22106, #22280 ) ;
#44390 = ORIENTED_EDGE ( 'NONE', *, *, #15375, .T. ) ;
#44391 = AXIS2_PLACEMENT_3D ( 'NONE', #7647, #22574, #7877 ) ;
#44392 = CARTESIAN_POINT ( 'NONE',  ( 0.000000000000000000, 55.20638768913760686, 51.02545421589343988 ) ) ;
#44393 = VECTOR ( 'NONE', #29032, 1000.000000000000000 ) ;
#44394 = ORIENTED_EDGE ( 'NONE', *, *, #11718, .F. ) ;
#44395 = ADVANCED_FACE ( 'NONE', ( #12810 ), #2261, .T. ) ;
#44396 = LINE ( 'NONE', #19166, #32413 ) ;
#44397 = FACE_OUTER_BOUND ( 'NONE', #36526, .T. ) ;
#44398 = CYLINDRICAL_SURFACE ( 'NONE', #25886, 16.00000000000000000 ) ;
#44400 = ORIENTED_EDGE ( 'NONE', *, *, #38543, .T. ) ;
#44399 = DIRECTION ( 'NONE',  ( 0.000000000000000000, 0.000000000000000000, 1.000000000000000000 ) ) ;
#44401 = ORIENTED_EDGE ( 'NONE', *, *, #22937, .F. ) ;
#44402 = DIRECTION ( 'NONE',  ( -0.000000000000000000, -0.000000000000000000, -1.000000000000000000 ) ) ;
#44403 = VERTEX_POINT ( 'NONE', #5233 ) ;
#44404 = ORIENTED_EDGE ( 'NONE', *, *, #16774, .F. ) ;
#44405 = CARTESIAN_POINT ( 'NONE',  ( 0.000000000000000000, -30.41916302227164337, 71.27951684758015460 ) ) ;
#44406 = LINE ( 'NONE', #40731, #10566 ) ;
#44407 = CARTESIAN_POINT ( 'NONE',  ( 5.000000000000000000, -38.55633173626998911, -16.65560815589452304 ) ) ;
#44408 = CYLINDRICAL_SURFACE ( 'NONE', #9400, 31.99999999999999289 ) ;
#44409 = ORIENTED_EDGE ( 'NONE', *, *, #44033, .F. ) ;
#44411 = CARTESIAN_POINT ( 'NONE',  ( 10.00000000000000000, 0.000000000000000000, 0.000000000000000000 ) ) ;
#44410 = AXIS2_PLACEMENT_3D ( 'NONE', #10849, #7165, #6931 ) ;
#44412 = DIRECTION ( 'NONE',  ( -1.000000000000000000, -0.000000000000000000, 0.000000000000000000 ) ) ;
#44413 = DIRECTION ( 'NONE',  ( 0.4796670183876317051, -0.8774505977381972244, 0.000000000000000000 ) ) ;
#44414 = CIRCLE ( 'NONE', #29563, 31.99999999999998934 ) ;
#44415 = DIRECTION ( 'NONE',  ( -0.8225049752423776450, -0.5687579148473765889, 0.000000000000000000 ) ) ;
#44416 = CARTESIAN_POINT ( 'NONE',  ( -3.000000000000000000, -3.948201729842348850, 23.21447184625293048 ) ) ;
#44417 = VERTEX_POINT ( 'NONE', #35564 ) ;
#44418 = CARTESIAN_POINT ( 'NONE',  ( 10.00000000000000000, 73.73191006444572793, -14.66109333815486515 ) ) ;
#44419 = CARTESIAN_POINT ( 'NONE',  ( 0.000000000000000000, 0.000000000000000000, 42.00000000000001421 ) ) ;
#44420 = LINE ( 'NONE', #28593, #36468 ) ;
#44421 = ADVANCED_FACE ( 'NONE', ( #12568 ), #2044, .T. ) ;
#44422 = DIRECTION ( 'NONE',  ( -1.000000000000000000, -0.000000000000000000, -0.000000000000000000 ) ) ;
#44423 = FACE_OUTER_BOUND ( 'NONE', #21876, .T. ) ;
#44424 = DIRECTION ( 'NONE',  ( -1.000000000000000000, 0.000000000000000000, 0.000000000000000000 ) ) ;
#44425 = CARTESIAN_POINT ( 'NONE',  ( -42.50000000000000000, 0.000000000000000000, 0.000000000000000000 ) ) ;
#44426 = CARTESIAN_POINT ( 'NONE',  ( 4.999999999999999112, 41.81611651403861885, 3.925862922256313503 ) ) ;
#44427 = DIRECTION ( 'NONE',  ( 1.000000000000000000, -0.000000000000000000, -0.000000000000000000 ) ) ;
#44428 = CARTESIAN_POINT ( 'NONE',  ( 0.000000000000000000, 75.54627589209970040, -17.28742895386005785 ) ) ;
#44429 = AXIS2_PLACEMENT_3D ( 'NONE', #6298, #21210, #21703 ) ;
#44430 = EDGE_CURVE ( 'NONE', #24067, #44556, #36349, .T. ) ;
#44431 = CARTESIAN_POINT ( 'NONE',  ( 11.99999999999999822, 0.000000000000000000, 0.000000000000000000 ) ) ;
#44432 = ADVANCED_FACE ( 'NONE', ( #42913 ), #5959, .T. ) ;
#44433 = ADVANCED_FACE ( 'NONE', ( #32140 ), #42675, .T. ) ;
#44434 = ORIENTED_EDGE ( 'NONE', *, *, #46739, .T. ) ;
#44435 = ORIENTED_EDGE ( 'NONE', *, *, #30609, .F. ) ;
#44436 = EDGE_CURVE ( 'NONE', #43138, #19294, #19077, .T. ) ;
#44437 = EDGE_CURVE ( 'NONE', #30049, #39130, #25323, .T. ) ;
#44438 = DIRECTION ( 'NONE',  ( 0.000000000000000000, 0.000000000000000000, 1.000000000000000000 ) ) ;
#44439 = ORIENTED_EDGE ( 'NONE', *, *, #10186, .T. ) ;
#44440 = AXIS2_PLACEMENT_3D ( 'NONE', #34539, #23299, #42142 ) ;
#44441 = CARTESIAN_POINT ( 'NONE',  ( 10.00000000000000000, 17.67226234102826510, 33.17418723428314564 ) ) ;
#44442 = VERTEX_POINT ( 'NONE', #46334 ) ;
#44443 = CARTESIAN_POINT ( 'NONE',  ( 10.00000000000000000, -37.58145647212453611, -0.6853352020794456489 ) ) ;
#44444 = FACE_OUTER_BOUND ( 'NONE', #21313, .T. ) ;
#44445 = VERTEX_POINT ( 'NONE', #17181 ) ;
#44446 = DIRECTION ( 'NONE',  ( 0.000000000000000000, 0.000000000000000000, 1.000000000000000000 ) ) ;
#44447 = VERTEX_POINT ( 'NONE', #24070 ) ;
#44448 = ORIENTED_EDGE ( 'NONE', *, *, #42208, .T. ) ;
#44449 = EDGE_LOOP ( 'NONE', ( #10198, #47002, #11480, #43776 ) ) ;
#44450 = DIRECTION ( 'NONE',  ( -1.000000000000000000, -0.000000000000000000, -0.000000000000000000 ) ) ;
#44451 = DIRECTION ( 'NONE',  ( 1.000000000000000000, 0.000000000000000000, 0.000000000000000000 ) ) ;
#44452 = CARTESIAN_POINT ( 'NONE',  ( 10.00000000000000000, 0.000000000000000000, 0.000000000000000000 ) ) ;
#44453 = VERTEX_POINT ( 'NONE', #5458 ) ;
#44454 = ORIENTED_EDGE ( 'NONE', *, *, #8404, .F. ) ;
#44455 = DIRECTION ( 'NONE',  ( 0.000000000000000000, 0.000000000000000000, 1.000000000000000000 ) ) ;
#44456 = VERTEX_POINT ( 'NONE', #16958 ) ;
#44457 = FACE_OUTER_BOUND ( 'NONE', #10640, .T. ) ;
#44458 = CIRCLE ( 'NONE', #17100, 37.49900000000000233 ) ;
#44459 = DIRECTION ( 'NONE',  ( 0.000000000000000000, -0.7071067811865536790, 0.7071067811865414665 ) ) ;
#44461 = DIRECTION ( 'NONE',  ( 0.000000000000000000, 0.000000000000000000, -1.000000000000000000 ) ) ;
#44460 = AXIS2_PLACEMENT_3D ( 'NONE', #9974, #10212, #32965 ) ;
#44462 = CARTESIAN_POINT ( 'NONE',  ( 10.00000000000000000, 0.000000000000000000, 0.000000000000000000 ) ) ;
#44463 = CARTESIAN_POINT ( 'NONE',  ( -9.055038557894883766, -98.31460683512894150, -2.500000000000000000 ) ) ;
#44464 = AXIS2_PLACEMENT_3D ( 'NONE', #4490, #22840, #29943 ) ;
#44465 = CARTESIAN_POINT ( 'NONE',  ( 0.000000000000000000, 21.40280677340421889, -36.13751322684397138 ) ) ;
#44466 = ADVANCED_FACE ( 'NONE', ( #47059 ), #39488, .T. ) ;
#44467 = DIRECTION ( 'NONE',  ( -0.000000000000000000, -0.000000000000000000, -1.000000000000000000 ) ) ;
#44468 = CARTESIAN_POINT ( 'NONE',  ( 11.99999999999999822, 80.28980883073758434, 16.65972982744962749 ) ) ;
#44469 = CARTESIAN_POINT ( 'NONE',  ( 0.000000000000000000, -78.73519480814971416, 22.90783923731600069 ) ) ;
#44470 = EDGE_CURVE ( 'NONE', #25450, #41683, #33122, .T. ) ;
#44471 = ORIENTED_EDGE ( 'NONE', *, *, #27739, .T. ) ;
#44472 = DIRECTION ( 'NONE',  ( 1.000000000000000000, -0.000000000000000000, 0.000000000000000000 ) ) ;
#44473 = ORIENTED_EDGE ( 'NONE', *, *, #48138, .T. ) ;
#44474 = EDGE_CURVE ( 'NONE', #13774, #35650, #24535, .T. ) ;
#44475 = DIRECTION ( 'NONE',  ( -1.000000000000000000, -0.000000000000000000, 0.000000000000000000 ) ) ;
#44476 = CARTESIAN_POINT ( 'NONE',  ( -10.00000000000000000, 0.000000000000000000, 0.000000000000000000 ) ) ;
#44477 = CARTESIAN_POINT ( 'NONE',  ( 6.000000000000000000, 10.30890764327501152, -81.34940948281325745 ) ) ;
#44478 = EDGE_CURVE ( 'NONE', #12245, #21082, #14375, .T. ) ;
#44479 = CYLINDRICAL_SURFACE ( 'NONE', #42139, 42.00000000000000000 ) ;
#44480 =( GEOMETRIC_REPRESENTATION_CONTEXT ( 3 ) GLOBAL_UNCERTAINTY_ASSIGNED_CONTEXT ( ( #45766 ) ) GLOBAL_UNIT_ASSIGNED_CONTEXT ( ( #41851, #30107, #37680 ) ) REPRESENTATION_CONTEXT ( 'NONE', 'WORKASPACE' ) );
#44481 = CARTESIAN_POINT ( 'NONE',  ( 0.000000000000000000, 66.50666863322055633, -39.78640506895536078 ) ) ;
#44482 = ORIENTED_EDGE ( 'NONE', *, *, #19554, .T. ) ;
#44483 = DIRECTION ( 'NONE',  ( -0.000000000000000000, 0.9945218953682731788, 0.1045284632676559550 ) ) ;
#44484 = CARTESIAN_POINT ( 'NONE',  ( -10.00000000000000000, 0.000000000000000000, 0.000000000000000000 ) ) ;
#44485 = DIRECTION ( 'NONE',  ( -1.000000000000000000, 0.000000000000000000, 0.000000000000000000 ) ) ;
#44486 = CARTESIAN_POINT ( 'NONE',  ( 10.00000000000000000, -37.16516213103273714, -4.992566952385376844 ) ) ;
#44487 = VERTEX_POINT ( 'NONE', #35313 ) ;
#44488 = EDGE_CURVE ( 'NONE', #41511, #38924, #41730, .T. ) ;
#44489 = EDGE_CURVE ( 'NONE', #17130, #6467, #31616, .T. ) ;
#44490 = ORIENTED_EDGE ( 'NONE', *, *, #322, .T. ) ;
#44491 = EDGE_LOOP ( 'NONE', ( #8756, #8632, #22237, #1457 ) ) ;
#44492 = AXIS2_PLACEMENT_3D ( 'NONE', #37885, #23192, #33716 ) ;
#44493 = ORIENTED_EDGE ( 'NONE', *, *, #17999, .T. ) ;
#44494 = EDGE_LOOP ( 'NONE', ( #30334, #44847, #47303, #20778 ) ) ;
#44495 = LINE ( 'NONE', #2891, #32713 ) ;
#44496 = DIRECTION ( 'NONE',  ( -6.951859121168206841E-17, 1.000000000000000000, 0.000000000000000000 ) ) ;
#44497 = VERTEX_POINT ( 'NONE', #31672 ) ;
#44498 = EDGE_LOOP ( 'NONE', ( #13115, #32707, #33712, #20710 ) ) ;
#44499 = EDGE_CURVE ( 'NONE', #29028, #6991, #46590, .T. ) ;
#44500 = VECTOR ( 'NONE', #33136, 1000.000000000000000 ) ;
#44501 = DIRECTION ( 'NONE',  ( 0.000000000000000000, 0.6494480483301848794, -0.7604059656000299317 ) ) ;
#44502 = ORIENTED_EDGE ( 'NONE', *, *, #2813, .F. ) ;
#44503 = ORIENTED_EDGE ( 'NONE', *, *, #38127, .T. ) ;
#44504 = CARTESIAN_POINT ( 'NONE',  ( 0.000000000000000000, -68.67312586194971402, -35.91791733033549860 ) ) ;
#44505 = VERTEX_POINT ( 'NONE', #24299 ) ;
#44506 = DIRECTION ( 'NONE',  ( 0.000000000000000000, 0.3826834323650841752, 0.9238795325112891810 ) ) ;
#44507 = VERTEX_POINT ( 'NONE', #20624 ) ;
#44508 = VERTEX_POINT ( 'NONE', #36990 ) ;
#44509 = CARTESIAN_POINT ( 'NONE',  ( 0.000000000000000000, -38.55633173627022359, 16.65560815589396526 ) ) ;
#44510 = DIRECTION ( 'NONE',  ( 0.000000000000000000, -0.9510565162951500895, -0.3090169943749582204 ) ) ;
#44511 = CARTESIAN_POINT ( 'NONE',  ( 10.00000000000000000, 0.000000000000000000, 37.49900000000000233 ) ) ;
#44512 = ORIENTED_EDGE ( 'NONE', *, *, #16103, .T. ) ;
#44513 = EDGE_LOOP ( 'NONE', ( #27164, #41504, #14466, #47297 ) ) ;
#44514 = DIRECTION ( 'NONE',  ( 0.000000000000000000, 0.000000000000000000, -1.000000000000000000 ) ) ;
#44515 = AXIS2_PLACEMENT_3D ( 'NONE', #36751, #36285, #17682 ) ;
#44516 = FACE_OUTER_BOUND ( 'NONE', #28986, .T. ) ;
#44517 = ADVANCED_FACE ( 'NONE', ( #10586 ), #28706, .T. ) ;
#44518 = ORIENTED_EDGE ( 'NONE', *, *, #33810, .T. ) ;
#44519 = AXIS2_PLACEMENT_3D ( 'NONE', #47400, #13874, #47621 ) ;
#44520 = VERTEX_POINT ( 'NONE', #25729 ) ;
#44521 = DIRECTION ( 'NONE',  ( -1.000000000000000000, 0.000000000000000000, 0.000000000000000000 ) ) ;
#44522 = CARTESIAN_POINT ( 'NONE',  ( 0.000000000000000000, 0.000000000000000000, 0.000000000000000000 ) ) ;
#44523 = ORIENTED_EDGE ( 'NONE', *, *, #10661, .F. ) ;
#44524 = LINE ( 'NONE', #5705, #8145 ) ;
#44526 = EDGE_CURVE ( 'NONE', #29421, #21411, #46448, .T. ) ;
#44525 = VECTOR ( 'NONE', #2467, 1000.000000000000000 ) ;
#44527 = CARTESIAN_POINT ( 'NONE',  ( 18.80329974962065265, -105.8248132807389084, 5.500000000000000000 ) ) ;
#44528 = CYLINDRICAL_SURFACE ( 'NONE', #18481, 37.49900000000000233 ) ;
#44529 = DIRECTION ( 'NONE',  ( -0.8541291221503275466, 0.5200609990132993854, 0.000000000000000000 ) ) ;
#44530 = LINE ( 'NONE', #25921, #32303 ) ;
#44531 = DIRECTION ( 'NONE',  ( 0.000000000000000000, 0.000000000000000000, 1.000000000000000000 ) ) ;
#44532 = EDGE_CURVE ( 'NONE', #17161, #36444, #8914, .T. ) ;
#44533 = CARTESIAN_POINT ( 'NONE',  ( 0.000000000000000000, -34.94270380257586339, -74.18225833017926618 ) ) ;
#44534 = DIRECTION ( 'NONE',  ( -0.7533909544171994987, -0.6575728627325958531, 2.465190328815662439E-32 ) ) ;
#44535 = DIRECTION ( 'NONE',  ( -1.000000000000000000, 0.000000000000000000, -0.000000000000000000 ) ) ;
#44536 = DIRECTION ( 'NONE',  ( 0.000000000000000000, 0.000000000000000000, 1.000000000000000000 ) ) ;
#44537 = CARTESIAN_POINT ( 'NONE',  ( -10.21100092698785033, -95.54625877152835756, -2.500000000000000000 ) ) ;
#44538 = CARTESIAN_POINT ( 'NONE',  ( 0.000000000000000000, 64.81221759200417409, -50.23322058963276504 ) ) ;
#44539 = DIRECTION ( 'NONE',  ( 0.000000000000000000, -0.4067366430757989315, -0.9135454576426015327 ) ) ;
#44540 = ORIENTED_EDGE ( 'NONE', *, *, #12827, .T. ) ;
#44541 = EDGE_CURVE ( 'NONE', #40027, #21200, #42535, .T. ) ;
#44542 = EDGE_CURVE ( 'NONE', #39825, #38904, #7143, .T. ) ;
#44543 = ORIENTED_EDGE ( 'NONE', *, *, #33177, .F. ) ;
#44544 = EDGE_CURVE ( 'NONE', #39455, #5074, #39390, .T. ) ;
#44545 = DIRECTION ( 'NONE',  ( -1.000000000000000000, 0.000000000000000000, 0.000000000000000000 ) ) ;
#44546 = CARTESIAN_POINT ( 'NONE',  ( 11.99999999999999822, 63.97538442413500093, -51.29473840253155714 ) ) ;
#44547 = VERTEX_POINT ( 'NONE', #22061 ) ;
#44548 = EDGE_CURVE ( 'NONE', #25213, #45055, #40206, .T. ) ;
#44549 = ORIENTED_EDGE ( 'NONE', *, *, #37986, .F. ) ;
#44550 = VECTOR ( 'NONE', #27688, 1000.000000000000227 ) ;
#44551 = AXIS2_PLACEMENT_3D ( 'NONE', #6460, #47565, #28966 ) ;
#44552 = CARTESIAN_POINT ( 'NONE',  ( 0.000000000000000000, -2.663952781845850826, -41.91543099594819921 ) ) ;
#44553 = ORIENTED_EDGE ( 'NONE', *, *, #25343, .T. ) ;
#44554 = FACE_OUTER_BOUND ( 'NONE', #14325, .T. ) ;
#44555 = CIRCLE ( 'NONE', #3110, 31.99999999999998934 ) ;
#44556 = VERTEX_POINT ( 'NONE', #3466 ) ;
#44557 = EDGE_LOOP ( 'NONE', ( #36302, #31471, #40923, #9225 ) ) ;
#44558 = ORIENTED_EDGE ( 'NONE', *, *, #42049, .T. ) ;
#44559 = CARTESIAN_POINT ( 'NONE',  ( 0.000000000000000000, -8.966570791701281351, 81.50828551894223040 ) ) ;
#44560 = AXIS2_PLACEMENT_3D ( 'NONE', #1120, #20206, #16067 ) ;
#44561 = VECTOR ( 'NONE', #22381, 1000.000000000000000 ) ;
#44562 = DIRECTION ( 'NONE',  ( -1.000000000000000000, -0.000000000000000000, -0.000000000000000000 ) ) ;
#44563 = CIRCLE ( 'NONE', #3117, 16.00000000000000711 ) ;
#44564 = ORIENTED_EDGE ( 'NONE', *, *, #37125, .T. ) ;
#44565 = ORIENTED_EDGE ( 'NONE', *, *, #11066, .F. ) ;
#44566 = CARTESIAN_POINT ( 'NONE',  ( 10.00000000000000000, 17.67226234102826510, 33.17418723428314564 ) ) ;
#44567 = VERTEX_POINT ( 'NONE', #32606 ) ;
#44568 = DIRECTION ( 'NONE',  ( 0.000000000000000000, 0.000000000000000000, 1.000000000000000000 ) ) ;
#44569 = LINE ( 'NONE', #25713, #32951 ) ;
#44570 = VERTEX_POINT ( 'NONE', #47532 ) ;
#44571 = LINE ( 'NONE', #37229, #42462 ) ;
#44572 = CYLINDRICAL_SURFACE ( 'NONE', #44267, 37.49900000000000233 ) ;
#44573 = ORIENTED_EDGE ( 'NONE', *, *, #35671, .F. ) ;
#44574 = CARTESIAN_POINT ( 'NONE',  ( 10.00000000000000000, 23.16143007188532366, -73.95703589263949596 ) ) ;
#44575 = CARTESIAN_POINT ( 'NONE',  ( 10.00000000000000000, 30.84782396557218931, 21.32104025579126017 ) ) ;
#44576 = ORIENTED_EDGE ( 'NONE', *, *, #6697, .F. ) ;
#44577 = CARTESIAN_POINT ( 'NONE',  ( 0.000000000000000000, -24.73286445877653961, -73.44644590900085745 ) ) ;
#44578 = VERTEX_POINT ( 'NONE', #47305 ) ;
#44579 = ORIENTED_EDGE ( 'NONE', *, *, #11570, .F. ) ;
#44580 = FACE_OUTER_BOUND ( 'NONE', #37657, .T. ) ;
#44581 = DIRECTION ( 'NONE',  ( 0.000000000000000000, 0.5877852522924685852, 0.8090169943749506709 ) ) ;
#44582 = ORIENTED_EDGE ( 'NONE', *, *, #32808, .F. ) ;
#44583 = EDGE_CURVE ( 'NONE', #37330, #36456, #7462, .T. ) ;
#44584 = DIRECTION ( 'NONE',  ( 0.000000000000000000, 0.07845909572783793529, 0.9969173337331285190 ) ) ;
#44585 = DIRECTION ( 'NONE',  ( 0.000000000000000000, -0.6494480483301739993, -0.7604059656000390355 ) ) ;
#44586 = CARTESIAN_POINT ( 'NONE',  ( 10.00000000000000000, -75.11725578898466438, -2.956366410621452001 ) ) ;
#44587 = EDGE_CURVE ( 'NONE', #10741, #41791, #7340, .T. ) ;
#44588 = LINE ( 'NONE', #36995, #41382 ) ;
#44589 = ADVANCED_FACE ( 'NONE', ( #6669 ), #25013, .T. ) ;
#44590 = CARTESIAN_POINT ( 'NONE',  ( -11.63999999999999702, 1.552852141318844077E-15, -12.50000000000000000 ) ) ;
#44591 = ADVANCED_FACE ( 'NONE', ( #39964 ), #18400, .T. ) ;
#44593 = AXIS2_PLACEMENT_3D ( 'NONE', #25595, #18250, #33190 ) ;
#44592 = CARTESIAN_POINT ( 'NONE',  ( 10.00000000000000000, 4.992566952384984269, 37.16516213103279398 ) ) ;
#44594 = AXIS2_PLACEMENT_3D ( 'NONE', #16229, #45851, #13039 ) ;
#44595 = FACE_OUTER_BOUND ( 'NONE', #4969, .T. ) ;
#44597 = EDGE_CURVE ( 'NONE', #47873, #14947, #29655, .T. ) ;
#44596 = DIRECTION ( 'NONE',  ( 0.000000000000000000, -0.9969173337331270757, -0.07845909572785580988 ) ) ;
#44598 = DIRECTION ( 'NONE',  ( 0.000000000000000000, 0.7071067811865436870, 0.7071067811865513475 ) ) ;
#44599 = LINE ( 'NONE', #25990, #16913 ) ;
#44600 = CIRCLE ( 'NONE', #41458, 12.49999999999999645 ) ;
#44601 = AXIS2_PLACEMENT_3D ( 'NONE', #13505, #28433, #21573 ) ;
#44602 = CARTESIAN_POINT ( 'NONE',  ( 0.000000000000000000, -89.50000000000000000, 2.500000000000000000 ) ) ;
#44603 = DIRECTION ( 'NONE',  ( -1.000000000000000000, 0.000000000000000000, -0.000000000000000000 ) ) ;
#44604 = DIRECTION ( 'NONE',  ( -1.000000000000000000, 0.000000000000000000, 0.000000000000000000 ) ) ;
#44605 = DIRECTION ( 'NONE',  ( -1.000000000000000000, -0.000000000000000000, 0.000000000000000000 ) ) ;
#44606 = CIRCLE ( 'NONE', #1635, 15.99999999999999822 ) ;
#44607 = EDGE_CURVE ( 'NONE', #35473, #25837, #5785, .T. ) ;
#44608 = VECTOR ( 'NONE', #9854, 1000.000000000000000 ) ;
#44609 = ORIENTED_EDGE ( 'NONE', *, *, #13483, .T. ) ;
#44610 = CARTESIAN_POINT ( 'NONE',  ( 103.9230484541331947, -179.9999999999990337, 5.500000000000000000 ) ) ;
#44611 = VECTOR ( 'NONE', #22549, 1000.000000000000000 ) ;
#44612 = VERTEX_POINT ( 'NONE', #47758 ) ;
#44613 = EDGE_CURVE ( 'NONE', #3193, #29274, #34801, .T. ) ;
#44614 = LINE ( 'NONE', #41202, #23654 ) ;
#44615 = SHAPE_DEFINITION_REPRESENTATION ( #10097, #45973 ) ;
#44616 = DIRECTION ( 'NONE',  ( 0.000000000000000000, 0.000000000000000000, 1.000000000000000000 ) ) ;
#44617 = EDGE_LOOP ( 'NONE', ( #7288, #12189, #28799, #3318 ) ) ;
#44618 = EDGE_CURVE ( 'NONE', #3340, #19509, #32369, .T. ) ;
#44619 = PLANE ( 'NONE',  #10424 ) ;
#44620 = VERTEX_POINT ( 'NONE', #48008 ) ;
#44621 = VECTOR ( 'NONE', #41236, 1000.000000000000000 ) ;
#44622 = ADVANCED_FACE ( 'NONE', ( #37244 ), #14498, .T. ) ;
#44623 = CARTESIAN_POINT ( 'NONE',  ( 10.00000000000000000, 0.000000000000000000, 0.000000000000000000 ) ) ;
#44624 = CIRCLE ( 'NONE', #32873, 16.00000000000000000 ) ;
#44625 = CARTESIAN_POINT ( 'NONE',  ( 10.00000000000000000, -33.71516098798792171, 74.74816331893418919 ) ) ;
#44626 = CARTESIAN_POINT ( 'NONE',  ( 12.13205353604972991, -140.1820037904669789, 5.500000000000000000 ) ) ;
#44627 = CONICAL_SURFACE ( 'NONE', #21949, 13.71319123046128752, 0.2094395102393127317 ) ;
#44628 = CIRCLE ( 'NONE', #14938, 37.49900000000000233 ) ;
#44629 = ORIENTED_EDGE ( 'NONE', *, *, #12544, .F. ) ;
#44630 = FACE_OUTER_BOUND ( 'NONE', #18548, .T. ) ;
#44631 = EDGE_LOOP ( 'NONE', ( #8714, #10087, #12012, #7300 ) ) ;
#44632 = AXIS2_PLACEMENT_3D ( 'NONE', #35496, #36452, #17356 ) ;
#44633 = CARTESIAN_POINT ( 'NONE',  ( 10.00000000000000000, 0.000000000000000000, 0.000000000000000000 ) ) ;
#44634 = CARTESIAN_POINT ( 'NONE',  ( 10.00000000000000000, 0.000000000000000000, 0.000000000000000000 ) ) ;
#44635 = VECTOR ( 'NONE', #19834, 1000.000000000000000 ) ;
#44636 = CARTESIAN_POINT ( 'NONE',  ( -10.43921258969510824, -98.89258801967538659, 5.500000000000000000 ) ) ;
#44637 = DIRECTION ( 'NONE',  ( 0.000000000000000000, 0.000000000000000000, 1.000000000000000000 ) ) ;
#44638 = ORIENTED_EDGE ( 'NONE', *, *, #888, .F. ) ;
#44639 = DIRECTION ( 'NONE',  ( 0.000000000000000000, 0.3826834323650841752, 0.9238795325112891810 ) ) ;
#44640 = ORIENTED_EDGE ( 'NONE', *, *, #43219, .F. ) ;
#44641 = ORIENTED_EDGE ( 'NONE', *, *, #29733, .F. ) ;
#44642 = EDGE_CURVE ( 'NONE', #21754, #35739, #27204, .T. ) ;
#44643 = DIRECTION ( 'NONE',  ( 0.000000000000000000, -0.9723699203976741146, -0.2334453638559160493 ) ) ;
#44644 = DIRECTION ( 'NONE',  ( 0.000000000000000000, 0.000000000000000000, 1.000000000000000000 ) ) ;
#44645 = CARTESIAN_POINT ( 'NONE',  ( -17.26469406256017791, -140.1601175325492648, 5.500000000000000000 ) ) ;
#44646 = DIRECTION ( 'NONE',  ( 0.000000000000000000, 0.8090169943749447867, 0.5877852522924769119 ) ) ;
#44647 = EDGE_LOOP ( 'NONE', ( #22376, #21456, #13853, #40773 ) ) ;
#44648 = LINE ( 'NONE', #37544, #8116 ) ;
#44649 = CARTESIAN_POINT ( 'NONE',  ( 10.00000000000000000, -37.22597642581153821, -5.202137450156795850 ) ) ;
#44650 = EDGE_CURVE ( 'NONE', #15618, #42302, #40196, .T. ) ;
#44651 = DIRECTION ( 'NONE',  ( -0.8225049752423776450, -0.5687579148473765889, 0.000000000000000000 ) ) ;
#44652 = DIRECTION ( 'NONE',  ( 0.000000000000000000, 0.3090169943749410675, 0.9510565162951556406 ) ) ;
#44653 = DIRECTION ( 'NONE',  ( 0.6064928550163511956, 0.7950889364178798102, -0.000000000000000000 ) ) ;
#44654 = DIRECTION ( 'NONE',  ( 1.000000000000000000, -0.000000000000000000, -0.000000000000000000 ) ) ;
#44655 = ORIENTED_EDGE ( 'NONE', *, *, #44613, .T. ) ;
#44657 = EDGE_CURVE ( 'NONE', #3694, #21639, #8351, .T. ) ;
#44656 = FACE_OUTER_BOUND ( 'NONE', #43242, .T. ) ;
#44658 = DIRECTION ( 'NONE',  ( 0.000000000000000000, 0.000000000000000000, 1.000000000000000000 ) ) ;
#44659 = LINE ( 'NONE', #18474, #28306 ) ;
#44660 = LINE ( 'NONE', #33164, #1844 ) ;
#44661 = DIRECTION ( 'NONE',  ( 0.000000000000000000, 0.000000000000000000, 1.000000000000000000 ) ) ;
#44662 = AXIS2_PLACEMENT_3D ( 'NONE', #5180, #8109, #46287 ) ;
#44663 = CARTESIAN_POINT ( 'NONE',  ( -18.24502636017238899, -100.7225776329765665, 5.500000000000000000 ) ) ;
#44664 = CARTESIAN_POINT ( 'NONE',  ( 0.000000000000000000, -6.555932627142143865, -37.01155633439065440 ) ) ;
#44665 = DIRECTION ( 'NONE',  ( -1.000000000000000000, 0.000000000000000000, -0.000000000000000000 ) ) ;
#44666 = CARTESIAN_POINT ( 'NONE',  ( -3.000000000000000000, 22.07842321921481243, 8.187992925817422218 ) ) ;
#44667 = AXIS2_PLACEMENT_3D ( 'NONE', #41286, #22668, #1116 ) ;
#44668 = AXIS2_PLACEMENT_3D ( 'NONE', #32243, #17056, #43734 ) ;
#44669 = CARTESIAN_POINT ( 'NONE',  ( 11.99999999999999822, -46.21855187248673502, 62.20884554314003623 ) ) ;
#44670 = VECTOR ( 'NONE', #10940, 1000.000000000000227 ) ;
#44671 = ORIENTED_EDGE ( 'NONE', *, *, #29111, .F. ) ;
#44672 = CIRCLE ( 'NONE', #8606, 31.99999999999999289 ) ;
#44673 = ORIENTED_EDGE ( 'NONE', *, *, #9317, .F. ) ;
#44674 = VECTOR ( 'NONE', #13759, 1000.000000000000000 ) ;
#44675 = FACE_OUTER_BOUND ( 'NONE', #23806, .T. ) ;
#44676 = EDGE_LOOP ( 'NONE', ( #44482, #5695, #15859 ) ) ;
#44677 = PLANE ( 'NONE',  #1129 ) ;
#44678 = CARTESIAN_POINT ( 'NONE',  ( 11.99999999999999822, 0.000000000000000000, 0.000000000000000000 ) ) ;
#44679 = LINE ( 'NONE', #47859, #39446 ) ;
#44680 = ORIENTED_EDGE ( 'NONE', *, *, #34579, .T. ) ;
#44681 = LINE ( 'NONE', #25350, #36713 ) ;
#44682 = ORIENTED_EDGE ( 'NONE', *, *, #48241, .T. ) ;
#44683 = ORIENTED_EDGE ( 'NONE', *, *, #1669, .F. ) ;
#44684 = CARTESIAN_POINT ( 'NONE',  ( -10.00000000000000000, 0.000000000000000000, 0.000000000000000000 ) ) ;
#44685 = CARTESIAN_POINT ( 'NONE',  ( 0.000000000000000000, 15.48615015657637883, -39.04073710021327770 ) ) ;
#44686 = AXIS2_PLACEMENT_3D ( 'NONE', #6552, #4345, #37616 ) ;
#44687 = EDGE_CURVE ( 'NONE', #45907, #13460, #9791, .T. ) ;
#44688 = FACE_BOUND ( 'NONE', #15705, .T. ) ;
#44689 = EDGE_LOOP ( 'NONE', ( #8261, #42345, #963, #18886 ) ) ;
#44691 = ORIENTED_EDGE ( 'NONE', *, *, #25062, .T. ) ;
#44690 = CIRCLE ( 'NONE', #14195, 31.99999999999998579 ) ;
#44692 = EDGE_LOOP ( 'NONE', ( #7299, #35726, #5511, #12651 ) ) ;
#44693 = DIRECTION ( 'NONE',  ( 1.000000000000000000, -0.000000000000000000, -0.000000000000000000 ) ) ;
#44694 = ORIENTED_EDGE ( 'NONE', *, *, #19488, .F. ) ;
#44695 = EDGE_CURVE ( 'NONE', #30299, #31998, #19840, .T. ) ;
#44696 = AXIS2_PLACEMENT_3D ( 'NONE', #253, #8336, #41160 ) ;
#44697 = CARTESIAN_POINT ( 'NONE',  ( -11.70000000000000107, 2.535018874235021196E-15, 20.69999999999999929 ) ) ;
#44698 = CYLINDRICAL_SURFACE ( 'NONE', #10798, 37.49900000000000233 ) ;
#44699 = CYLINDRICAL_SURFACE ( 'NONE', #3357, 77.49899999999999523 ) ;
#44700 = FACE_OUTER_BOUND ( 'NONE', #17045, .T. ) ;
#44701 = CARTESIAN_POINT ( 'NONE',  ( 0.000000000000000000, 36.72794159290241822, 65.59268652807223532 ) ) ;
#44702 = EDGE_CURVE ( 'NONE', #43790, #42577, #34519, .T. ) ;
#44703 = CARTESIAN_POINT ( 'NONE',  ( -22.67106064244953245, -113.6342314410295842, 5.500000000000000000 ) ) ;
#44704 = CIRCLE ( 'NONE', #19671, 77.49900000000000944 ) ;
#44705 = LINE ( 'NONE', #47884, #7661 ) ;
#44706 = FACE_OUTER_BOUND ( 'NONE', #47395, .T. ) ;
#44707 = DIRECTION ( 'NONE',  ( -1.000000000000000000, -0.000000000000000000, -0.000000000000000000 ) ) ;
#44708 = ORIENTED_EDGE ( 'NONE', *, *, #46757, .T. ) ;
#44709 = LINE ( 'NONE', #6793, #25131 ) ;
#44710 = EDGE_LOOP ( 'NONE', ( #16277, #43963, #43600, #36425 ) ) ;
#44712 = EDGE_CURVE ( 'NONE', #3893, #32798, #27693, .T. ) ;
#44711 = CARTESIAN_POINT ( 'NONE',  ( 11.99999999999999822, -20.40083707022829174, -72.35432306680507963 ) ) ;
#44713 = AXIS2_PLACEMENT_3D ( 'NONE', #26886, #37170, #41821 ) ;
#44714 = DIRECTION ( 'NONE',  ( -1.000000000000000000, 0.000000000000000000, 0.000000000000000000 ) ) ;
#44715 = EDGE_CURVE ( 'NONE', #23496, #7974, #23039, .T. ) ;
#44716 = DIRECTION ( 'NONE',  ( -0.000000000000000000, -0.000000000000000000, -1.000000000000000000 ) ) ;
#44717 = DIRECTION ( 'NONE',  ( 1.000000000000000000, 0.000000000000000000, 0.000000000000000000 ) ) ;
#44718 = DIRECTION ( 'NONE',  ( -0.2867529058022021404, 0.9580045777625456616, 0.000000000000000000 ) ) ;
#44719 = LINE ( 'NONE', #29791, #7601 ) ;
#44720 = DIRECTION ( 'NONE',  ( 0.000000000000000000, 0.000000000000000000, -1.000000000000000000 ) ) ;
#44721 = CYLINDRICAL_SURFACE ( 'NONE', #36290, 16.00000000000000000 ) ;
#44722 = VECTOR ( 'NONE', #19770, 1000.000000000000000 ) ;
#44723 = EDGE_CURVE ( 'NONE', #7347, #39648, #21418, .T. ) ;
#44724 = FACE_OUTER_BOUND ( 'NONE', #33067, .T. ) ;
#44725 = CARTESIAN_POINT ( 'NONE',  ( 1.355716935723751293, -120.6418968688129496, -2.500000000000000000 ) ) ;
#44726 = ORIENTED_EDGE ( 'NONE', *, *, #38239, .T. ) ;
#44727 = ORIENTED_EDGE ( 'NONE', *, *, #26489, .F. ) ;
#44728 = AXIS2_PLACEMENT_3D ( 'NONE', #22139, #41243, #11856 ) ;
#44729 = VECTOR ( 'NONE', #23743, 1000.000000000000000 ) ;
#44730 = VERTEX_POINT ( 'NONE', #34282 ) ;
#44731 = DIRECTION ( 'NONE',  ( 0.000000000000000000, 0.000000000000000000, 1.000000000000000000 ) ) ;
#44732 = CARTESIAN_POINT ( 'NONE',  ( 10.00000000000000000, 77.49459641780886443, 0.8261519478433866359 ) ) ;
#44733 = AXIS2_PLACEMENT_3D ( 'NONE', #9142, #39005, #1798 ) ;
#44734 = EDGE_CURVE ( 'NONE', #46550, #31057, #4453, .T. ) ;
#44735 = FACE_OUTER_BOUND ( 'NONE', #48242, .T. ) ;
#44736 = EDGE_CURVE ( 'NONE', #20071, #7163, #15462, .T. ) ;
#44737 = EDGE_LOOP ( 'NONE', ( #24040, #33770, #120, #4118 ) ) ;
#44738 = ORIENTED_EDGE ( 'NONE', *, *, #44357, .F. ) ;
#44739 = ADVANCED_FACE ( 'NONE', ( #23512 ), #30396, .F. ) ;
#44740 = CARTESIAN_POINT ( 'NONE',  ( 11.99999999999999822, 74.18225833017889670, 34.94270380257665209 ) ) ;
#44741 = VERTEX_POINT ( 'NONE', #7630 ) ;
#44742 = DIRECTION ( 'NONE',  ( 0.000000000000000000, 0.000000000000000000, -1.000000000000000000 ) ) ;
#44743 = VERTEX_POINT ( 'NONE', #41898 ) ;
#44744 = CARTESIAN_POINT ( 'NONE',  ( 10.00000000000000000, 22.64427369931169309, 30.00120703465213623 ) ) ;
#44745 = ORIENTED_EDGE ( 'NONE', *, *, #2817, .F. ) ;
#44746 = ORIENTED_EDGE ( 'NONE', *, *, #5715, .F. ) ;
#44747 = DIRECTION ( 'NONE',  ( 0.000000000000000000, -0.9945218953682730678, -0.1045284632676570791 ) ) ;
#44748 = AXIS2_PLACEMENT_3D ( 'NONE', #29592, #44521, #26172 ) ;
#44749 = CARTESIAN_POINT ( 'NONE',  ( 0.000000000000000000, 6.736453364083555329, 36.88895765772635116 ) ) ;
#44750 = VECTOR ( 'NONE', #31935, 1000.000000000000227 ) ;
#44751 = ADVANCED_FACE ( 'NONE', ( #22560 ), #3712, .T. ) ;
#44752 = CARTESIAN_POINT ( 'NONE',  ( 10.00000000000000000, 30.84782396557218931, 21.32104025579126017 ) ) ;
#44753 = ORIENTED_EDGE ( 'NONE', *, *, #22436, .F. ) ;
#44754 = EDGE_CURVE ( 'NONE', #44507, #28263, #4289, .T. ) ;
#44755 = EDGE_CURVE ( 'NONE', #3949, #45561, #11316, .T. ) ;
#44756 = ORIENTED_EDGE ( 'NONE', *, *, #45114, .F. ) ;
#44757 = CIRCLE ( 'NONE', #20514, 82.00000000000000000 ) ;
#44758 = SURFACE_STYLE_USAGE ( .BOTH. , #15401 ) ;
#44759 = CYLINDRICAL_SURFACE ( 'NONE', #27461, 37.49900000000000233 ) ;
#44760 = ORIENTED_EDGE ( 'NONE', *, *, #1873, .T. ) ;
#44761 = VERTEX_POINT ( 'NONE', #33798 ) ;
#44762 = FACE_OUTER_BOUND ( 'NONE', #31803, .T. ) ;
#44763 = EDGE_LOOP ( 'NONE', ( #8260, #36612, #22110, #34629 ) ) ;
#44764 = DIRECTION ( 'NONE',  ( 1.000000000000000000, 0.000000000000000000, 0.000000000000000000 ) ) ;
#44765 = CARTESIAN_POINT ( 'NONE',  ( 0.000000000000000000, 0.000000000000000000, 0.000000000000000000 ) ) ;
#44766 = VECTOR ( 'NONE', #5103, 1000.000000000000000 ) ;
#44767 = CARTESIAN_POINT ( 'NONE',  ( 10.00000000000000000, -65.59268652807237743, 36.72794159290217664 ) ) ;
#44768 = DIRECTION ( 'NONE',  ( 0.000000000000000000, -0.4539904997395542430, 0.8910065241883641241 ) ) ;
#44769 = ORIENTED_EDGE ( 'NONE', *, *, #45463, .F. ) ;
#44770 = FACE_OUTER_BOUND ( 'NONE', #498, .T. ) ;
#44771 = DIRECTION ( 'NONE',  ( 1.000000000000000000, -0.000000000000000000, 0.000000000000000000 ) ) ;
#44772 = AXIS2_PLACEMENT_3D ( 'NONE', #2167, #9741, #17804 ) ;
#44773 = EDGE_CURVE ( 'NONE', #40664, #23509, #1908, .T. ) ;
#44774 = DIRECTION ( 'NONE',  ( -0.2867529058022035837, 0.9580045777625452175, 0.000000000000000000 ) ) ;
#44775 = AXIS2_PLACEMENT_3D ( 'NONE', #15038, #3773, #6730 ) ;
#44776 = DIRECTION ( 'NONE',  ( -0.2306669878475648139, -0.9730327541852491491, 0.000000000000000000 ) ) ;
#44777 = DIRECTION ( 'NONE',  ( -1.000000000000000000, 0.000000000000000000, -0.000000000000000000 ) ) ;
#44778 = AXIS2_PLACEMENT_3D ( 'NONE', #5987, #1577, #13315 ) ;
#44779 = DIRECTION ( 'NONE',  ( 0.000000000000000000, 0.000000000000000000, -1.000000000000000000 ) ) ;
#44780 = DIRECTION ( 'NONE',  ( 1.000000000000000000, 0.000000000000000000, 0.000000000000000000 ) ) ;
#44781 = DIRECTION ( 'NONE',  ( -0.000000000000000000, -0.000000000000000000, -1.000000000000000000 ) ) ;
#44782 = EDGE_LOOP ( 'NONE', ( #7225, #7597, #8448, #5020 ) ) ;
#44783 = EDGE_LOOP ( 'NONE', ( #39423, #43602, #37398, #1837 ) ) ;
#44784 = PRODUCT_DEFINITION_CONTEXT ( 'detailed design', #32577, 'design' ) ;
#44785 = DIRECTION ( 'NONE',  ( 0.000000000000000000, 0.000000000000000000, 1.000000000000000000 ) ) ;
#44786 = CARTESIAN_POINT ( 'NONE',  ( -22.53294031248082163, -134.0273518838794757, 5.500000000000000000 ) ) ;
#44787 = AXIS2_PLACEMENT_3D ( 'NONE', #23064, #30416, #33356 ) ;
#44788 = DIRECTION ( 'NONE',  ( -1.000000000000000000, 0.000000000000000000, 0.000000000000000000 ) ) ;
#44789 = ORIENTED_EDGE ( 'NONE', *, *, #22037, .T. ) ;
#44790 = AXIS2_PLACEMENT_3D ( 'NONE', #16914, #6617, #2002 ) ;
#44791 = EDGE_CURVE ( 'NONE', #23027, #25415, #8105, .T. ) ;
#44792 = CARTESIAN_POINT ( 'NONE',  ( 10.00000000000000000, -74.18225833017864090, -34.94270380257719211 ) ) ;
#44793 = AXIS2_PLACEMENT_3D ( 'NONE', #4558, #46399, #27083 ) ;
#44794 = VECTOR ( 'NONE', #32020, 1000.000000000000000 ) ;
#44795 = ORIENTED_EDGE ( 'NONE', *, *, #12124, .F. ) ;
#44796 = ORIENTED_EDGE ( 'NONE', *, *, #24289, .T. ) ;
#44797 = EDGE_CURVE ( 'NONE', #27040, #46360, #2683, .T. ) ;
#44798 = VERTEX_POINT ( 'NONE', #530 ) ;
#44799 = EDGE_LOOP ( 'NONE', ( #19047, #10527, #15423, #34138 ) ) ;
#44800 = DIRECTION ( 'NONE',  ( -1.000000000000000000, -0.000000000000000000, -0.000000000000000000 ) ) ;
#44801 = EDGE_CURVE ( 'NONE', #32047, #15128, #44908, .T. ) ;
#44802 = AXIS2_PLACEMENT_3D ( 'NONE', #4571, #45936, #19714 ) ;
#44803 = CARTESIAN_POINT ( 'NONE',  ( 11.99999999999999822, -71.87247863392384772, -39.47590169984923136 ) ) ;
#44804 = AXIS2_PLACEMENT_3D ( 'NONE', #44141, #3742, #18666 ) ;
#44805 = AXIS2_PLACEMENT_3D ( 'NONE', #32145, #47064, #6197 ) ;
#44806 = ORIENTED_EDGE ( 'NONE', *, *, #39852, .T. ) ;
#44807 = VERTEX_POINT ( 'NONE', #46777 ) ;
#44808 = DIRECTION ( 'NONE',  ( 0.000000000000000000, 0.000000000000000000, 1.000000000000000000 ) ) ;
#44809 = VECTOR ( 'NONE', #11343, 1000.000000000000000 ) ;
#44810 = VERTEX_POINT ( 'NONE', #46046 ) ;
#44811 = LINE ( 'NONE', #11296, #43404 ) ;
#44812 = LINE ( 'NONE', #11297, #24390 ) ;
#44814 = EDGE_LOOP ( 'NONE', ( #11756, #8329, #46474, #23397 ) ) ;
#44813 = VECTOR ( 'NONE', #47347, 1000.000000000000000 ) ;
#44815 = EDGE_CURVE ( 'NONE', #43484, #1236, #16419, .T. ) ;
#44816 = CARTESIAN_POINT ( 'NONE',  ( 10.00000000000000000, 0.000000000000000000, 0.000000000000000000 ) ) ;
#44817 = CARTESIAN_POINT ( 'NONE',  ( 10.00000000000000000, 0.000000000000000000, 0.000000000000000000 ) ) ;
#44818 = EDGE_CURVE ( 'NONE', #47647, #20, #353, .T. ) ;
#44819 = ORIENTED_EDGE ( 'NONE', *, *, #5429, .T. ) ;
#44820 = CARTESIAN_POINT ( 'NONE',  ( 11.99999999999999822, 0.000000000000000000, 0.000000000000000000 ) ) ;
#44821 = PLANE ( 'NONE',  #36794 ) ;
#44822 = EDGE_LOOP ( 'NONE', ( #11686, #25022, #26215, #47636 ) ) ;
#44823 = DIRECTION ( 'NONE',  ( 0.000000000000000000, 0.000000000000000000, -1.000000000000000000 ) ) ;
#44824 = ORIENTED_EDGE ( 'NONE', *, *, #38235, .F. ) ;
#44825 = ORIENTED_EDGE ( 'NONE', *, *, #38405, .F. ) ;
#44826 = DIRECTION ( 'NONE',  ( 0.000000000000000000, 0.000000000000000000, 1.000000000000000000 ) ) ;
#44827 = FACE_OUTER_BOUND ( 'NONE', #10733, .T. ) ;
#44828 = DIRECTION ( 'NONE',  ( 0.000000000000000000, -0.9510565162951499785, -0.3090169943749582204 ) ) ;
#44829 = LINE ( 'NONE', #26238, #28184 ) ;
#44830 = CARTESIAN_POINT ( 'NONE',  ( 10.00000000000000000, -75.54627589209931671, -17.28742895386164591 ) ) ;
#44831 = DIRECTION ( 'NONE',  ( 1.000000000000000000, 0.000000000000000000, 0.000000000000000000 ) ) ;
#44832 = DIRECTION ( 'NONE',  ( 0.000000000000000000, 0.7431448254773862505, 0.6691306063588672304 ) ) ;
#44833 = AXIS2_PLACEMENT_3D ( 'NONE', #30349, #45497, #45269 ) ;
#44834 = ADVANCED_FACE ( 'NONE', ( #1734 ), #27942, .F. ) ;
#44835 = CYLINDRICAL_SURFACE ( 'NONE', #43470, 82.00000000000000000 ) ;
#44836 = LINE ( 'NONE', #40681, #21565 ) ;
#44837 = DIRECTION ( 'NONE',  ( 0.000000000000000000, 0.000000000000000000, -1.000000000000000000 ) ) ;
#44838 = LINE ( 'NONE', #11073, #34191 ) ;
#44839 = CARTESIAN_POINT ( 'NONE',  ( 11.99999999999999822, -65.64334221924937651, 41.19522573413711797 ) ) ;
#44840 = AXIS2_PLACEMENT_3D ( 'NONE', #10450, #36148, #2604 ) ;
#44841 = CIRCLE ( 'NONE', #31581, 82.00000000000000000 ) ;
#44842 = CARTESIAN_POINT ( 'NONE',  ( 24.95699195200416654, -110.9640411295978595, 5.500000000000000000 ) ) ;
#44843 = CARTESIAN_POINT ( 'NONE',  ( 10.00000000000000000, 26.02418014898407961, -70.52718814184231633 ) ) ;
#44844 = CARTESIAN_POINT ( 'NONE',  ( 0.000000000000000000, -35.92658777277502935, -10.74501242461320594 ) ) ;
#44845 = CARTESIAN_POINT ( 'NONE',  ( 10.00000000000000000, -35.95386929396248377, -10.96151621346525751 ) ) ;
#44846 = VERTEX_POINT ( 'NONE', #9542 ) ;
#44847 = ORIENTED_EDGE ( 'NONE', *, *, #13370, .F. ) ;
#44848 = ORIENTED_EDGE ( 'NONE', *, *, #41040, .F. ) ;
#44850 = CARTESIAN_POINT ( 'NONE',  ( 11.99999999999999822, 55.19960302592141232, -51.03279382321027668 ) ) ;
#44849 = AXIS2_PLACEMENT_3D ( 'NONE', #24275, #21071, #2469 ) ;
#44851 = VECTOR ( 'NONE', #10405, 1000.000000000000000 ) ;
#44852 = ORIENTED_EDGE ( 'NONE', *, *, #36951, .F. ) ;
#44853 = AXIS2_PLACEMENT_3D ( 'NONE', #42860, #38951, #27206 ) ;
#44854 = DIRECTION ( 'NONE',  ( 0.000000000000000000, 0.000000000000000000, 1.000000000000000000 ) ) ;
#44855 = VECTOR ( 'NONE', #10547, 1000.000000000000000 ) ;
#44856 = DIRECTION ( 'NONE',  ( 0.000000000000000000, 0.000000000000000000, 1.000000000000000000 ) ) ;
#44857 = DIRECTION ( 'NONE',  ( -0.7533909544171996098, -0.6575728627325956310, 0.000000000000000000 ) ) ;
#44858 = AXIS2_PLACEMENT_3D ( 'NONE', #3997, #8143, #33839 ) ;
#44859 = ORIENTED_EDGE ( 'NONE', *, *, #36962, .F. ) ;
#44860 = DIRECTION ( 'NONE',  ( 0.000000000000000000, -0.7071067811865389130, -0.7071067811865561215 ) ) ;
#44861 = ADVANCED_FACE ( 'NONE', ( #24241 ), #5647, .T. ) ;
#44862 = ORIENTED_EDGE ( 'NONE', *, *, #31642, .T. ) ;
#44863 = VERTEX_POINT ( 'NONE', #23757 ) ;
#44864 = EDGE_CURVE ( 'NONE', #19937, #7880, #24485, .T. ) ;
#44865 = CIRCLE ( 'NONE', #21417, 11.59999999999999787 ) ;
#44866 = AXIS2_PLACEMENT_3D ( 'NONE', #33333, #48261, #2980 ) ;
#44867 = DIRECTION ( 'NONE',  ( -1.000000000000000000, -1.390371824233641368E-16, 0.000000000000000000 ) ) ;
#44868 = ADVANCED_FACE ( 'NONE', ( #16905 ), #19833, .F. ) ;
#44869 = LINE ( 'NONE', #15267, #35155 ) ;
#44870 = VECTOR ( 'NONE', #38039, 1000.000000000000000 ) ;
#44871 = AXIS2_PLACEMENT_3D ( 'NONE', #2096, #16299, #45922 ) ;
#44873 = ORIENTED_EDGE ( 'NONE', *, *, #16095, .T. ) ;
#44872 = PLANE ( 'NONE',  #20706 ) ;
#44874 = VERTEX_POINT ( 'NONE', #39175 ) ;
#44875 = CARTESIAN_POINT ( 'NONE',  ( -11.63999999999999702, 0.000000000000000000, 12.50000000000000000 ) ) ;
#44876 = DIRECTION ( 'NONE',  ( -1.000000000000000000, 0.000000000000000000, -0.000000000000000000 ) ) ;
#44877 = ADVANCED_FACE ( 'NONE', ( #31609 ), #27684, .T. ) ;
#44878 = CARTESIAN_POINT ( 'NONE',  ( 10.00000000000000000, 65.59268652807210742, 36.72794159290264560 ) ) ;
#44879 = FACE_OUTER_BOUND ( 'NONE', #32068, .T. ) ;
#44880 = VECTOR ( 'NONE', #33229, 1000.000000000000000 ) ;
#44881 = ORIENTED_EDGE ( 'NONE', *, *, #24710, .F. ) ;
#44882 = CARTESIAN_POINT ( 'NONE',  ( 0.000000000000000000, 11.30684508768339569, 76.66974797899841576 ) ) ;
#44883 = VERTEX_POINT ( 'NONE', #2212 ) ;
#44884 = ORIENTED_EDGE ( 'NONE', *, *, #39186, .F. ) ;
#44885 = ADVANCED_FACE ( 'NONE', ( #20316 ), #17136, .T. ) ;
#44886 = CIRCLE ( 'NONE', #40222, 31.99999999999999645 ) ;
#44887 = CARTESIAN_POINT ( 'NONE',  ( 0.000000000000000000, 37.58145647212455032, -0.6853352020786441789 ) ) ;
#44888 = AXIS2_PLACEMENT_3D ( 'NONE', #12971, #23721, #38677 ) ;
#44889 = DIRECTION ( 'NONE',  ( -1.000000000000000000, 0.000000000000000000, -0.000000000000000000 ) ) ;
#44890 = DIRECTION ( 'NONE',  ( 0.000000000000000000, -0.8090169943749402348, -0.5877852522924830181 ) ) ;
#44891 = CARTESIAN_POINT ( 'NONE',  ( 0.000000000000000000, 0.000000000000000000, 0.000000000000000000 ) ) ;
#44892 = VERTEX_POINT ( 'NONE', #9080 ) ;
#44893 = DIRECTION ( 'NONE',  ( -1.000000000000000000, 0.000000000000000000, -0.000000000000000000 ) ) ;
#44894 = FACE_OUTER_BOUND ( 'NONE', #46274, .T. ) ;
#44895 = DIRECTION ( 'NONE',  ( 0.000000000000000000, 0.000000000000000000, 1.000000000000000000 ) ) ;
#44896 = CARTESIAN_POINT ( 'NONE',  ( -1.200000000000000030E-05, 0.9569279952884607310, 2.500000000000015543 ) ) ;
#44897 = EDGE_CURVE ( 'NONE', #31833, #14564, #27724, .T. ) ;
#44898 = CARTESIAN_POINT ( 'NONE',  ( -4.653126046682595884, -146.1313684676804314, -5.500000000000000000 ) ) ;
#44899 = DIRECTION ( 'NONE',  ( -1.000000000000000000, -0.000000000000000000, 0.000000000000000000 ) ) ;
#44900 = CARTESIAN_POINT ( 'NONE',  ( 10.00000000000000000, -37.16516213103280108, 4.992566952384862589 ) ) ;
#44901 = DIRECTION ( 'NONE',  ( -1.000000000000000000, -0.000000000000000000, 0.000000000000000000 ) ) ;
#44903 = AXIS2_PLACEMENT_3D ( 'NONE', #35, #282, #44596 ) ;
#44902 = CARTESIAN_POINT ( 'NONE',  ( 0.000000000000000000, 81.34940948281351325, -10.30890764327296161 ) ) ;
#44904 = CARTESIAN_POINT ( 'NONE',  ( 0.000000000000000000, -46.11716303203136391, -67.80270845531939017 ) ) ;
#44905 = LINE ( 'NONE', #598, #37206 ) ;
#44906 = EDGE_CURVE ( 'NONE', #47208, #42659, #34772, .T. ) ;
#44907 = VERTEX_POINT ( 'NONE', #24013 ) ;
#44908 = CIRCLE ( 'NONE', #9710, 31.99999999999999289 ) ;
#44909 = DIRECTION ( 'NONE',  ( 0.000000000000000000, 0.000000000000000000, 1.000000000000000000 ) ) ;
#44910 = CARTESIAN_POINT ( 'NONE',  ( 0.000000000000000000, 32.34446384429971033, 26.79245525562726371 ) ) ;
#44911 = LINE ( 'NONE', #22870, #14538 ) ;
#44912 = VECTOR ( 'NONE', #18722, 1000.000000000000000 ) ;
#44913 = CARTESIAN_POINT ( 'NONE',  ( 0.000000000000000000, -15.48615015657556171, -39.04073710021360455 ) ) ;
#44914 = CIRCLE ( 'NONE', #2687, 37.49900000000000233 ) ;
#44915 = DIRECTION ( 'NONE',  ( -0.000000000000000000, -0.000000000000000000, -1.000000000000000000 ) ) ;
#44916 = ORIENTED_EDGE ( 'NONE', *, *, #23105, .T. ) ;
#44917 = ORIENTED_EDGE ( 'NONE', *, *, #27180, .T. ) ;
#44918 = VECTOR ( 'NONE', #18725, 1000.000000000000000 ) ;
#44919 = AXIS2_PLACEMENT_3D ( 'NONE', #5188, #20103, #43103 ) ;
#44920 = CIRCLE ( 'NONE', #366, 31.99999999999998224 ) ;
#44921 = ADVANCED_FACE ( 'NONE', ( #1256 ), #4916, .T. ) ;
#44922 = VERTEX_POINT ( 'NONE', #12751 ) ;
#44923 = VECTOR ( 'NONE', #22356, 1000.000000000000000 ) ;
#44924 = EDGE_CURVE ( 'NONE', #17540, #10420, #46492, .T. ) ;
#44925 = VECTOR ( 'NONE', #6369, 1000.000000000000000 ) ;
#44926 = CARTESIAN_POINT ( 'NONE',  ( 10.00000000000000000, -76.41127070299280888, 12.93880638057289012 ) ) ;
#44927 = ORIENTED_EDGE ( 'NONE', *, *, #23426, .F. ) ;
#44928 = VECTOR ( 'NONE', #35858, 1000.000000000000000 ) ;
#44929 = ADVANCED_FACE ( 'NONE', ( #16661 ), #46532, .T. ) ;
#44930 = DIRECTION ( 'NONE',  ( -1.000000000000000000, 0.000000000000000000, 0.000000000000000000 ) ) ;
#44931 = ADVANCED_FACE ( 'NONE', ( #33273 ), #17851, .T. ) ;
#44932 = DIRECTION ( 'NONE',  ( 0.000000000000000000, -0.2079116908177532363, -0.9781476007338069101 ) ) ;
#44933 = DIRECTION ( 'NONE',  ( -1.000000000000000000, -0.000000000000000000, -0.000000000000000000 ) ) ;
#44934 = VERTEX_POINT ( 'NONE', #47949 ) ;
#44935 = LINE ( 'NONE', #11419, #43030 ) ;
#44936 = ORIENTED_EDGE ( 'NONE', *, *, #32986, .F. ) ;
#44937 = VERTEX_POINT ( 'NONE', #36924 ) ;
#44938 = ORIENTED_EDGE ( 'NONE', *, *, #20597, .F. ) ;
#44939 = CARTESIAN_POINT ( 'NONE',  ( -24.50849501662245800, -109.8101191361138831, -2.500000000000000444 ) ) ;
#44940 = LINE ( 'NONE', #11423, #10275 ) ;
#44942 = CYLINDRICAL_SURFACE ( 'NONE', #2450, 82.00000000000000000 ) ;
#44941 = CIRCLE ( 'NONE', #23844, 37.49900000000000944 ) ;
#44943 = ORIENTED_EDGE ( 'NONE', *, *, #606, .T. ) ;
#44944 = ORIENTED_EDGE ( 'NONE', *, *, #14156, .F. ) ;
#44945 = CARTESIAN_POINT ( 'NONE',  ( 0.000000000000000000, -73.95703589263990807, 23.16143007188399139 ) ) ;
#44946 = VERTEX_POINT ( 'NONE', #29108 ) ;
#44947 = CIRCLE ( 'NONE', #45757, 16.00000000000000000 ) ;
#44948 = CARTESIAN_POINT ( 'NONE',  ( -3.000000000000000000, -3.948201729842348850, 23.21447184625293048 ) ) ;
#44949 = FACE_OUTER_BOUND ( 'NONE', #22079, .T. ) ;
#44950 = DIRECTION ( 'NONE',  ( -1.000000000000000000, -0.000000000000000000, -0.000000000000000000 ) ) ;
#44951 = DIRECTION ( 'NONE',  ( -1.000000000000000000, 0.000000000000000000, -0.000000000000000000 ) ) ;
#44952 = CARTESIAN_POINT ( 'NONE',  ( 15.00000000000000000, -3.948201729842032215, 23.21447184625297666 ) ) ;
#44953 = PLANE ( 'NONE',  #12773 ) ;
#44954 = CARTESIAN_POINT ( 'NONE',  ( -10.00000000000000000, 0.000000000000000000, 0.000000000000000000 ) ) ;
#44955 = EDGE_LOOP ( 'NONE', ( #1438, #40314, #8315, #23022 ) ) ;
#44956 = LINE ( 'NONE', #33681, #16408 ) ;
#44957 = CARTESIAN_POINT ( 'NONE',  ( 10.00000000000000000, 68.67312586195046720, -35.91791733033402068 ) ) ;
#44958 = VERTEX_POINT ( 'NONE', #47243 ) ;
#44959 = LINE ( 'NONE', #153, #45464 ) ;
#44960 = EDGE_CURVE ( 'NONE', #47874, #41381, #25433, .T. ) ;
#44961 = AXIS2_PLACEMENT_3D ( 'NONE', #25328, #31990, #46901 ) ;
#44962 = VERTEX_POINT ( 'NONE', #14437 ) ;
#44963 = DIRECTION ( 'NONE',  ( -1.000000000000000000, 0.000000000000000000, -0.000000000000000000 ) ) ;
#44964 = CIRCLE ( 'NONE', #29338, 37.49900000000001654 ) ;
#44965 = CARTESIAN_POINT ( 'NONE',  ( 0.000000000000000000, -38.55633173627022359, 16.65560815589396526 ) ) ;
#44966 = DIRECTION ( 'NONE',  ( -1.000000000000000000, 0.000000000000000000, 0.000000000000000000 ) ) ;
#44967 = LINE ( 'NONE', #45209, #6485 ) ;
#44968 = EDGE_CURVE ( 'NONE', #6290, #48430, #44290, .T. ) ;
#44969 = AXIS2_PLACEMENT_3D ( 'NONE', #36807, #7914, #6958 ) ;
#44970 = VECTOR ( 'NONE', #14722, 1000.000000000000000 ) ;
#44971 = LINE ( 'NONE', #45441, #9120 ) ;
#44972 = CYLINDRICAL_SURFACE ( 'NONE', #34959, 77.49899999999999523 ) ;
#44973 = EDGE_CURVE ( 'NONE', #21860, #30240, #14681, .T. ) ;
#44974 = DIRECTION ( 'NONE',  ( 0.000000000000000000, 0.000000000000000000, 1.000000000000000000 ) ) ;
#44975 = DIRECTION ( 'NONE',  ( 0.000000000000000000, 0.9945218953682732899, -0.1045284632676548031 ) ) ;
#44976 = EDGE_LOOP ( 'NONE', ( #29075, #35522, #27349, #27147 ) ) ;
#44977 = AXIS2_PLACEMENT_3D ( 'NONE', #2936, #36701, #6859 ) ;
#44978 = CARTESIAN_POINT ( 'NONE',  ( 11.99999999999999822, -51.02545421589285723, -55.20638768913812555 ) ) ;
#44979 = DIRECTION ( 'NONE',  ( 0.000000000000000000, 0.000000000000000000, 1.000000000000000000 ) ) ;
#44980 = ORIENTED_EDGE ( 'NONE', *, *, #3962, .T. ) ;
#44981 = VECTOR ( 'NONE', #4027, 1000.000000000000000 ) ;
#44982 = ADVANCED_FACE ( 'NONE', ( #33018 ), #29596, .F. ) ;
#44983 = ORIENTED_EDGE ( 'NONE', *, *, #45035, .F. ) ;
#44984 = ORIENTED_EDGE ( 'NONE', *, *, #23829, .T. ) ;
#44985 = DIRECTION ( 'NONE',  ( 0.8225049752423776450, 0.5687579148473765889, 0.000000000000000000 ) ) ;
#44986 = ADVANCED_FACE ( 'NONE', ( #3156 ), #17614, .F. ) ;
#44987 = DIRECTION ( 'NONE',  ( 1.000000000000000000, 0.000000000000000000, 0.000000000000000000 ) ) ;
#44988 = ORIENTED_EDGE ( 'NONE', *, *, #19399, .T. ) ;
#44989 = VECTOR ( 'NONE', #31897, 1000.000000000000227 ) ;
#44990 = CIRCLE ( 'NONE', #38745, 15.99999999999999822 ) ;
#44991 = EDGE_CURVE ( 'NONE', #34977, #21133, #36692, .T. ) ;
#44992 = DIRECTION ( 'NONE',  ( 0.000000000000000000, 0.000000000000000000, 1.000000000000000000 ) ) ;
#44993 = ORIENTED_EDGE ( 'NONE', *, *, #32758, .T. ) ;
#44994 = CIRCLE ( 'NONE', #23895, 15.99999999999999822 ) ;
#44995 = EDGE_CURVE ( 'NONE', #14629, #5793, #23797, .T. ) ;
#44996 = ORIENTED_EDGE ( 'NONE', *, *, #14535, .F. ) ;
#44997 = AXIS2_PLACEMENT_3D ( 'NONE', #45355, #9133, #23567 ) ;
#44998 = AXIS2_PLACEMENT_3D ( 'NONE', #252, #30140, #45064 ) ;
#44999 = DIRECTION ( 'NONE',  ( 1.000000000000000000, 0.000000000000000000, 0.000000000000000000 ) ) ;
#45001 = ORIENTED_EDGE ( 'NONE', *, *, #16214, .T. ) ;
#45000 = CARTESIAN_POINT ( 'NONE',  ( 10.00000000000000000, -33.80338159004273280, -16.23288003029533044 ) ) ;
#45002 = DIRECTION ( 'NONE',  ( -0.000000000000000000, -0.9135454576426004225, -0.4067366430758009854 ) ) ;
#45003 = ORIENTED_EDGE ( 'NONE', *, *, #9276, .T. ) ;
#45004 = CARTESIAN_POINT ( 'NONE',  ( -8.826826895187510402, -94.96827758698185562, -5.500000000000000000 ) ) ;
#45005 = ORIENTED_EDGE ( 'NONE', *, *, #38351, .F. ) ;
#45006 = ORIENTED_EDGE ( 'NONE', *, *, #4983, .T. ) ;
#45007 = DIRECTION ( 'NONE',  ( -1.000000000000000000, 0.000000000000000000, -0.000000000000000000 ) ) ;
#45008 = VECTOR ( 'NONE', #34879, 1000.000000000000000 ) ;
#45009 = LINE ( 'NONE', #4385, #15074 ) ;
#45010 = CARTESIAN_POINT ( 'NONE',  ( 0.000000000000000000, -46.54456581323762521, -59.03342792756313884 ) ) ;
#45011 = AXIS2_PLACEMENT_3D ( 'NONE', #22625, #12116, #37803 ) ;
#45012 = ORIENTED_EDGE ( 'NONE', *, *, #22753, .T. ) ;
#45013 = ORIENTED_EDGE ( 'NONE', *, *, #45215, .T. ) ;
#45014 = AXIS2_PLACEMENT_3D ( 'NONE', #31377, #27949, #42866 ) ;
#45015 = LINE ( 'NONE', #11489, #45440 ) ;
#45016 = ORIENTED_EDGE ( 'NONE', *, *, #28562, .T. ) ;
#45017 = ORIENTED_EDGE ( 'NONE', *, *, #14405, .F. ) ;
#45018 = DIRECTION ( 'NONE',  ( 1.000000000000000000, -0.000000000000000000, -0.000000000000000000 ) ) ;
#45019 = ORIENTED_EDGE ( 'NONE', *, *, #15979, .T. ) ;
#45020 = CARTESIAN_POINT ( 'NONE',  ( 10.00000000000000000, -35.47612816024539484, 22.48208911017487921 ) ) ;
#45021 = CARTESIAN_POINT ( 'NONE',  ( -11.59517495878806947, -96.12423995607481686, -2.500000000000000000 ) ) ;
#45022 = CARTESIAN_POINT ( 'NONE',  ( 10.00000000000000000, 0.000000000000000000, 0.000000000000000000 ) ) ;
#45023 = DIRECTION ( 'NONE',  ( 0.000000000000000000, 0.000000000000000000, 1.000000000000000000 ) ) ;
#45024 = DIRECTION ( 'NONE',  ( 0.000000000000000000, 0.000000000000000000, -1.000000000000000000 ) ) ;
#45025 = AXIS2_PLACEMENT_3D ( 'NONE', #9673, #27565, #42493 ) ;
#45026 = CARTESIAN_POINT ( 'NONE',  ( 10.00000000000000000, -29.81001611430991360, -22.74946021919165418 ) ) ;
#45027 = DIRECTION ( 'NONE',  ( 0.000000000000000000, 0.000000000000000000, -1.000000000000000000 ) ) ;
#45028 = CIRCLE ( 'NONE', #35631, 16.00000000000000000 ) ;
#45029 = DIRECTION ( 'NONE',  ( 1.000000000000000000, 0.000000000000000000, -0.000000000000000000 ) ) ;
#45030 = CARTESIAN_POINT ( 'NONE',  ( 0.000000000000000000, 51.02545421589324803, 55.20638768913779870 ) ) ;
#45031 = EDGE_CURVE ( 'NONE', #22790, #29332, #29254, .T. ) ;
#45032 = AXIS2_PLACEMENT_3D ( 'NONE', #39498, #6434, #21606 ) ;
#45033 = DIRECTION ( 'NONE',  ( -1.000000000000000000, 0.000000000000000000, 0.000000000000000000 ) ) ;
#45034 = CARTESIAN_POINT ( 'NONE',  ( 10.00000000000000000, 59.03961581697399907, 46.53671651293969802 ) ) ;
#45035 = EDGE_CURVE ( 'NONE', #2188, #20236, #32555, .T. ) ;
#45036 = AXIS2_PLACEMENT_3D ( 'NONE', #7139, #14496, #36745 ) ;
#45037 = LINE ( 'NONE', #11987, #21696 ) ;
#45038 = VERTEX_POINT ( 'NONE', #39902 ) ;
#45039 = AXIS2_PLACEMENT_3D ( 'NONE', #41007, #33882, #47739 ) ;
#45040 = DIRECTION ( 'NONE',  ( 0.000000000000000000, 0.000000000000000000, 1.000000000000000000 ) ) ;
#45041 = VECTOR ( 'NONE', #17436, 1000.000000000000000 ) ;
#45042 = DIRECTION ( 'NONE',  ( -1.000000000000000000, 0.000000000000000000, 0.000000000000000000 ) ) ;
#45043 = EDGE_CURVE ( 'NONE', #32940, #6721, #40147, .T. ) ;
#45044 = VECTOR ( 'NONE', #9841, 1000.000000000000000 ) ;
#45045 = DIRECTION ( 'NONE',  ( 0.000000000000000000, 0.3090169943749572767, 0.9510565162951503115 ) ) ;
#45046 = ORIENTED_EDGE ( 'NONE', *, *, #16160, .F. ) ;
#45047 = ADVANCED_FACE ( 'NONE', ( #6607 ), #40613, .T. ) ;
#45048 = EDGE_CURVE ( 'NONE', #28565, #28374, #2437, .T. ) ;
#45049 = AXIS2_PLACEMENT_3D ( 'NONE', #26430, #19309, #45494 ) ;
#45050 = ORIENTED_EDGE ( 'NONE', *, *, #30472, .T. ) ;
#45051 = LINE ( 'NONE', #7599, #17098 ) ;
#45052 = VERTEX_POINT ( 'NONE', #35978 ) ;
#45053 = ORIENTED_EDGE ( 'NONE', *, *, #37085, .T. ) ;
#45054 = VERTEX_POINT ( 'NONE', #6372 ) ;
#45055 = VERTEX_POINT ( 'NONE', #36218 ) ;
#45056 = EDGE_CURVE ( 'NONE', #17996, #37652, #14406, .T. ) ;
#45057 = DIRECTION ( 'NONE',  ( -1.000000000000000000, -0.000000000000000000, -0.000000000000000000 ) ) ;
#45058 = VECTOR ( 'NONE', #30319, 1000.000000000000114 ) ;
#45059 = FACE_OUTER_BOUND ( 'NONE', #8402, .T. ) ;
#45060 = VERTEX_POINT ( 'NONE', #32317 ) ;
#45061 = DIRECTION ( 'NONE',  ( -0.3311129884571280546, -0.9435911131814402886, 0.000000000000000000 ) ) ;
#45062 = ORIENTED_EDGE ( 'NONE', *, *, #8129, .F. ) ;
#45063 = VECTOR ( 'NONE', #14192, 1000.000000000000000 ) ;
#45064 = DIRECTION ( 'NONE',  ( 0.000000000000000000, 0.8090169943749433434, -0.5877852522924786882 ) ) ;
#45065 = DIRECTION ( 'NONE',  ( 1.000000000000000000, -0.000000000000000000, -0.000000000000000000 ) ) ;
#45066 = VERTEX_POINT ( 'NONE', #7078 ) ;
#45067 = DIRECTION ( 'NONE',  ( -1.000000000000000000, -0.000000000000000000, -0.000000000000000000 ) ) ;
#45068 = DIRECTION ( 'NONE',  ( 0.000000000000000000, -0.3090169943749560555, -0.9510565162951506446 ) ) ;
#45069 = ORIENTED_EDGE ( 'NONE', *, *, #3075, .F. ) ;
#45070 = CARTESIAN_POINT ( 'NONE',  ( 0.000000000000000000, 0.000000000000000000, 0.000000000000000000 ) ) ;
#45071 = DIRECTION ( 'NONE',  ( 0.000000000000000000, 0.9781476007338041345, 0.2079116908177664480 ) ) ;
#45072 = ORIENTED_EDGE ( 'NONE', *, *, #35819, .F. ) ;
#45073 = CIRCLE ( 'NONE', #12243, 82.00000000000000000 ) ;
#45074 = DIRECTION ( 'NONE',  ( -1.000000000000000000, 0.000000000000000000, 0.000000000000000000 ) ) ;
#45075 = ORIENTED_EDGE ( 'NONE', *, *, #29629, .T. ) ;
#45076 = CYLINDRICAL_SURFACE ( 'NONE', #38522, 37.49900000000000233 ) ;
#45077 = DIRECTION ( 'NONE',  ( -0.2079116908177587875, 1.197885328332318196E-16, -0.9781476007338056888 ) ) ;
#45078 = ORIENTED_EDGE ( 'NONE', *, *, #26687, .F. ) ;
#45079 = DIRECTION ( 'NONE',  ( -1.000000000000000000, 0.000000000000000000, 0.000000000000000000 ) ) ;
#45080 = DIRECTION ( 'NONE',  ( 0.000000000000000000, -0.7604059656000227152, -0.6494480483301933171 ) ) ;
#45081 = DIRECTION ( 'NONE',  ( -1.000000000000000000, -0.000000000000000000, 0.000000000000000000 ) ) ;
#45082 = VECTOR ( 'NONE', #42252, 1000.000000000000000 ) ;
#45083 = DIRECTION ( 'NONE',  ( 1.000000000000000000, -0.000000000000000000, 0.000000000000000000 ) ) ;
#45084 = LINE ( 'NONE', #3717, #25089 ) ;
#45085 = AXIS2_PLACEMENT_3D ( 'NONE', #26610, #37140, #41073 ) ;
#45086 = CARTESIAN_POINT ( 'NONE',  ( 0.000000000000000000, 26.08949754953024325, 27.05870788708241648 ) ) ;
#45087 = ORIENTED_EDGE ( 'NONE', *, *, #14203, .F. ) ;
#45088 = EDGE_CURVE ( 'NONE', #39890, #8273, #13718, .T. ) ;
#45089 = CARTESIAN_POINT ( 'NONE',  ( -25.50183398199384754, -112.6408924756582053, 5.500000000000000000 ) ) ;
#45090 = CARTESIAN_POINT ( 'NONE',  ( 0.000000000000000000, 0.000000000000000000, -43.79999999999998295 ) ) ;
#45091 = LINE ( 'NONE', #34059, #12311 ) ;
#45092 = CARTESIAN_POINT ( 'NONE',  ( 0.000000000000000000, -89.50000000000000000, -2.500000000000000000 ) ) ;
#45093 = ADVANCED_FACE ( 'NONE', ( #11249 ), #11729, .T. ) ;
#45094 = DIRECTION ( 'NONE',  ( 0.000000000000000000, -0.000000000000000000, 1.000000000000000000 ) ) ;
#45095 = DIRECTION ( 'NONE',  ( 0.000000000000000000, 0.9945218953682730678, 0.1045284632676570929 ) ) ;
#45096 = CARTESIAN_POINT ( 'NONE',  ( -2.500000000000000000, 16.00000000000000000, -19.01812422950394676 ) ) ;
#45097 = DIRECTION ( 'NONE',  ( 1.000000000000000000, -0.000000000000000000, -0.000000000000000000 ) ) ;
#45098 = EDGE_CURVE ( 'NONE', #24069, #32517, #18305, .T. ) ;
#45099 = EDGE_LOOP ( 'NONE', ( #10063, #5148, #2833, #14960 ) ) ;
#45100 = ORIENTED_EDGE ( 'NONE', *, *, #14867, .T. ) ;
#45101 = LINE ( 'NONE', #41425, #11232 ) ;
#45102 = ORIENTED_EDGE ( 'NONE', *, *, #35422, .T. ) ;
#45103 = FACE_OUTER_BOUND ( 'NONE', #24393, .T. ) ;
#45104 = DIRECTION ( 'NONE',  ( -0.6912384115093119785, 0.7226267767347698268, 0.000000000000000000 ) ) ;
#45105 = VECTOR ( 'NONE', #7581, 1000.000000000000114 ) ;
#45106 = DIRECTION ( 'NONE',  ( -1.000000000000000000, 0.000000000000000000, 0.000000000000000000 ) ) ;
#45107 = VERTEX_POINT ( 'NONE', #45021 ) ;
#45108 = EDGE_CURVE ( 'NONE', #5144, #34646, #3454, .T. ) ;
#45109 = EDGE_CURVE ( 'NONE', #5369, #44237, #30836, .T. ) ;
#45110 = VECTOR ( 'NONE', #40999, 1000.000000000000114 ) ;
#45111 = CYLINDRICAL_SURFACE ( 'NONE', #21392, 31.99999999999998579 ) ;
#45112 = ORIENTED_EDGE ( 'NONE', *, *, #17880, .T. ) ;
#45113 = AXIS2_PLACEMENT_3D ( 'NONE', #29493, #25567, #29728 ) ;
#45114 = EDGE_CURVE ( 'NONE', #9766, #17390, #37074, .T. ) ;
#45115 = AXIS2_PLACEMENT_3D ( 'NONE', #600, #34126, #7216 ) ;
#45116 = DIRECTION ( 'NONE',  ( 1.000000000000000000, 0.000000000000000000, 0.000000000000000000 ) ) ;
#45117 = DIRECTION ( 'NONE',  ( -1.000000000000000000, -0.000000000000000000, 0.000000000000000000 ) ) ;
#45119 = ORIENTED_EDGE ( 'NONE', *, *, #10278, .F. ) ;
#45118 = CARTESIAN_POINT ( 'NONE',  ( -20.62008904684763166, -131.2721749321093512, 2.500000000000000000 ) ) ;
#45120 = EDGE_LOOP ( 'NONE', ( #5799, #560, #17129, #4396 ) ) ;
#45121 = AXIS2_PLACEMENT_3D ( 'NONE', #2564, #48088, #36105 ) ;
#45122 = DIRECTION ( 'NONE',  ( -1.000000000000000000, -0.000000000000000000, -0.000000000000000000 ) ) ;
#45123 = CARTESIAN_POINT ( 'NONE',  ( -0.2999999999999947153, 0.000000000000000000, 0.000000000000000000 ) ) ;
#45124 = CARTESIAN_POINT ( 'NONE',  ( 11.99999999999999822, -62.50884508063395373, -41.76106447765554464 ) ) ;
#45125 = ORIENTED_EDGE ( 'NONE', *, *, #18070, .T. ) ;
#45128 = ORIENTED_EDGE ( 'NONE', *, *, #35159, .T. ) ;
#45127 = CARTESIAN_POINT ( 'NONE',  ( 0.000000000000000000, -35.95386929396248377, -10.96151621346525751 ) ) ;
#45126 = VECTOR ( 'NONE', #44402, 1000.000000000000000 ) ;
#45129 = VERTEX_POINT ( 'NONE', #15635 ) ;
#45130 = DIRECTION ( 'NONE',  ( -0.7585478161175706058, -0.6516173805718078471, 0.000000000000000000 ) ) ;
#45131 = VERTEX_POINT ( 'NONE', #699 ) ;
#45132 = ORIENTED_EDGE ( 'NONE', *, *, #28411, .T. ) ;
#45133 = CARTESIAN_POINT ( 'NONE',  ( -10.00000000000000000, 0.000000000000000000, 0.000000000000000000 ) ) ;
#45134 = AXIS2_PLACEMENT_3D ( 'NONE', #23647, #33698, #42253 ) ;
#45135 = PLANE ( 'NONE',  #28535 ) ;
#45136 = DIRECTION ( 'NONE',  ( 0.000000000000000000, -0.1564344650402380854, 0.9876883405951365491 ) ) ;
#45137 = DIRECTION ( 'NONE',  ( 0.000000000000000000, 0.000000000000000000, 1.000000000000000000 ) ) ;
#45138 = ORIENTED_EDGE ( 'NONE', *, *, #27140, .F. ) ;
#45139 = DIRECTION ( 'NONE',  ( 0.000000000000000000, 0.000000000000000000, 1.000000000000000000 ) ) ;
#45140 = FACE_OUTER_BOUND ( 'NONE', #19767, .T. ) ;
#45141 = DIRECTION ( 'NONE',  ( 0.000000000000000000, 0.000000000000000000, 1.000000000000000000 ) ) ;
#45142 = DIRECTION ( 'NONE',  ( -1.000000000000000000, -0.000000000000000000, 0.000000000000000000 ) ) ;
#45143 = PLANE ( 'NONE',  #7474 ) ;
#45144 = EDGE_CURVE ( 'NONE', #46010, #39534, #48044, .T. ) ;
#45145 = CIRCLE ( 'NONE', #40471, 15.99999999999999822 ) ;
#45146 = CARTESIAN_POINT ( 'NONE',  ( -19.90058851926621131, -132.5883508287165853, 5.500000000000000000 ) ) ;
#45147 = EDGE_LOOP ( 'NONE', ( #26558, #43797, #28908, #34135 ) ) ;
#45148 = CARTESIAN_POINT ( 'NONE',  ( 10.00000000000000000, 0.000000000000000000, 0.000000000000000000 ) ) ;
#45149 = DIRECTION ( 'NONE',  ( -1.000000000000000000, 0.000000000000000000, 0.000000000000000000 ) ) ;
#45150 = EDGE_CURVE ( 'NONE', #26165, #25953, #33991, .T. ) ;
#45151 = DIRECTION ( 'NONE',  ( 0.000000000000000000, -0.5000000000000046629, 0.8660254037844359321 ) ) ;
#45152 = DIRECTION ( 'NONE',  ( -1.000000000000000000, 0.000000000000000000, 0.000000000000000000 ) ) ;
#45153 = ADVANCED_FACE ( 'NONE', ( #18585 ), #15409, .T. ) ;
#45154 = FACE_OUTER_BOUND ( 'NONE', #17717, .T. ) ;
#45155 = AXIS2_PLACEMENT_3D ( 'NONE', #33286, #44058, #44539 ) ;
#45156 = CARTESIAN_POINT ( 'NONE',  ( 0.000000000000000000, 10.41901085202135491, -40.68715046381917944 ) ) ;
#45157 = CARTESIAN_POINT ( 'NONE',  ( 5.999999999999999112, -64.81221759200306565, -50.23322058963418613 ) ) ;
#45158 = DIRECTION ( 'NONE',  ( -1.000000000000000000, 0.000000000000000000, 0.000000000000000000 ) ) ;
#45159 = EDGE_LOOP ( 'NONE', ( #8455, #20533, #38931, #48381 ) ) ;
#45160 = DIRECTION ( 'NONE',  ( -1.000000000000000000, 0.000000000000000000, 0.000000000000000000 ) ) ;
#45161 = ORIENTED_EDGE ( 'NONE', *, *, #12662, .F. ) ;
#45162 = EDGE_CURVE ( 'NONE', #13391, #11885, #33197, .T. ) ;
#45163 = ORIENTED_EDGE ( 'NONE', *, *, #12599, .F. ) ;
#45164 = EDGE_CURVE ( 'NONE', #5635, #30321, #33506, .T. ) ;
#45165 = VECTOR ( 'NONE', #29648, 1000.000000000000000 ) ;
#45166 = EDGE_CURVE ( 'NONE', #31729, #21754, #34462, .T. ) ;
#45167 = ORIENTED_EDGE ( 'NONE', *, *, #20315, .F. ) ;
#45168 = ORIENTED_EDGE ( 'NONE', *, *, #26483, .T. ) ;
#45169 = AXIS2_PLACEMENT_3D ( 'NONE', #15609, #11948, #45465 ) ;
#45170 = CARTESIAN_POINT ( 'NONE',  ( 10.00000000000000000, -36.72794159290288718, 65.59268652807197952 ) ) ;
#45171 = VERTEX_POINT ( 'NONE', #18809 ) ;
#45172 = EDGE_CURVE ( 'NONE', #22252, #44086, #12119, .T. ) ;
#45173 = DIRECTION ( 'NONE',  ( 0.000000000000000000, 0.000000000000000000, 1.000000000000000000 ) ) ;
#45174 = EDGE_LOOP ( 'NONE', ( #2176, #33192, #22660, #20740 ) ) ;
#45175 = DIRECTION ( 'NONE',  ( -1.000000000000000000, 0.000000000000000000, -0.000000000000000000 ) ) ;
#45176 = LINE ( 'NONE', #38306, #46500 ) ;
#45177 = ORIENTED_EDGE ( 'NONE', *, *, #17633, .F. ) ;
#45178 = CARTESIAN_POINT ( 'NONE',  ( 10.00000000000000000, 0.000000000000000000, 0.000000000000000000 ) ) ;
#45179 = ORIENTED_EDGE ( 'NONE', *, *, #33590, .T. ) ;
#45180 = ORIENTED_EDGE ( 'NONE', *, *, #10060, .T. ) ;
#45181 = DIRECTION ( 'NONE',  ( -1.000000000000000000, -0.000000000000000000, -0.000000000000000000 ) ) ;
#45182 = DIRECTION ( 'NONE',  ( -1.000000000000000000, 0.000000000000000000, 0.000000000000000000 ) ) ;
#45183 = VECTOR ( 'NONE', #26348, 1000.000000000000000 ) ;
#45184 = LINE ( 'NONE', #4064, #36106 ) ;
#45185 = ORIENTED_EDGE ( 'NONE', *, *, #8302, .F. ) ;
#45186 = ORIENTED_EDGE ( 'NONE', *, *, #43224, .F. ) ;
#45187 = ORIENTED_EDGE ( 'NONE', *, *, #12780, .T. ) ;
#45188 = LINE ( 'NONE', #19951, #37268 ) ;
#45189 = VERTEX_POINT ( 'NONE', #40859 ) ;
#45190 = DIRECTION ( 'NONE',  ( 0.000000000000000000, 0.9510565162951544194, -0.3090169943749446757 ) ) ;
#45191 = DIRECTION ( 'NONE',  ( 0.000000000000000000, 0.9135454576426003115, 0.4067366430758017071 ) ) ;
#45192 = DIRECTION ( 'NONE',  ( 0.000000000000000000, 0.000000000000000000, 1.000000000000000000 ) ) ;
#45193 = DIRECTION ( 'NONE',  ( 0.000000000000000000, 0.000000000000000000, 1.000000000000000000 ) ) ;
#45194 = FACE_OUTER_BOUND ( 'NONE', #34298, .T. ) ;
#45195 = CARTESIAN_POINT ( 'NONE',  ( 0.000000000000000000, 0.000000000000000000, 0.000000000000000000 ) ) ;
#45196 = DIRECTION ( 'NONE',  ( 0.000000000000000000, -0.9876883405951394357, 0.1564344650402205716 ) ) ;
#45197 = DIRECTION ( 'NONE',  ( -1.000000000000000000, 0.000000000000000000, 0.000000000000000000 ) ) ;
#45198 = DIRECTION ( 'NONE',  ( 0.000000000000000000, 0.4539904997395414754, 0.8910065241883706744 ) ) ;
#45199 = VERTEX_POINT ( 'NONE', #934 ) ;
#45200 = FACE_OUTER_BOUND ( 'NONE', #27880, .T. ) ;
#45201 = CIRCLE ( 'NONE', #38956, 42.00000000000000000 ) ;
#45202 = ORIENTED_EDGE ( 'NONE', *, *, #17618, .T. ) ;
#45203 = ORIENTED_EDGE ( 'NONE', *, *, #32868, .F. ) ;
#45204 = DIRECTION ( 'NONE',  ( 0.000000000000000000, 0.9510565162951523099, 0.3090169943749515591 ) ) ;
#45206 = ADVANCED_FACE ( 'NONE', ( #26659 ), #30824, .F. ) ;
#45205 = CIRCLE ( 'NONE', #35830, 32.00000000000000000 ) ;
#45207 = CARTESIAN_POINT ( 'NONE',  ( 10.00000000000000000, -58.39081064771713869, -50.95692526931392052 ) ) ;
#45208 = FACE_OUTER_BOUND ( 'NONE', #47045, .T. ) ;
#45209 = CARTESIAN_POINT ( 'NONE',  ( 10.00000000000000000, 25.88420570971438650, -27.13269053701069566 ) ) ;
#45210 = EDGE_CURVE ( 'NONE', #34499, #20591, #5860, .T. ) ;
#45211 = AXIS2_PLACEMENT_3D ( 'NONE', #23675, #23930, #42778 ) ;
#45212 = ADVANCED_FACE ( 'NONE', ( #22735 ), #25918, .F. ) ;
#45213 = PLANE ( 'NONE',  #6788 ) ;
#45214 = DIRECTION ( 'NONE',  ( 0.000000000000000000, 0.1564344650402313408, -0.9876883405951376593 ) ) ;
#45215 = EDGE_CURVE ( 'NONE', #34943, #25765, #388, .T. ) ;
#45216 = CYLINDRICAL_SURFACE ( 'NONE', #45085, 82.00000000000000000 ) ;
#45217 = EDGE_CURVE ( 'NONE', #46360, #43938, #15257, .T. ) ;
#45218 = CYLINDRICAL_SURFACE ( 'NONE', #33401, 77.49899999999999523 ) ;
#45219 = EDGE_CURVE ( 'NONE', #43548, #18388, #29288, .T. ) ;
#45220 = PRODUCT_DEFINITION_FORMATION_WITH_SPECIFIED_SOURCE ( 'ANY', '', #47219, .NOT_KNOWN. ) ;
#45221 = SHAPE_REPRESENTATION_RELATIONSHIP ( 'NONE' , 'NONE' ,  #9091, #37976 ) ;
#45222 = DIRECTION ( 'NONE',  ( -1.000000000000000000, 0.000000000000000000, 0.000000000000000000 ) ) ;
#45223 = ORIENTED_EDGE ( 'NONE', *, *, #25907, .T. ) ;
#45224 = CIRCLE ( 'NONE', #10843, 15.99999999999999822 ) ;
#45225 = EDGE_CURVE ( 'NONE', #37785, #12329, #42074, .T. ) ;
#45226 = ORIENTED_EDGE ( 'NONE', *, *, #8780, .F. ) ;
#45227 = DIRECTION ( 'NONE',  ( -1.000000000000000000, -0.000000000000000000, -0.000000000000000000 ) ) ;
#45228 = DIRECTION ( 'NONE',  ( 0.000000000000000000, 0.000000000000000000, 1.000000000000000000 ) ) ;
#45229 = ADVANCED_FACE ( 'NONE', ( #31072 ), #12456, .T. ) ;
#45230 = DIRECTION ( 'NONE',  ( -1.000000000000000000, -0.000000000000000000, 0.000000000000000000 ) ) ;
#45231 = ORIENTED_EDGE ( 'NONE', *, *, #3637, .T. ) ;
#45232 = ORIENTED_EDGE ( 'NONE', *, *, #37138, .T. ) ;
#45233 = VECTOR ( 'NONE', #46381, 1000.000000000000000 ) ;
#45234 = CARTESIAN_POINT ( 'NONE',  ( 0.000000000000000000, 26.02418014898407961, -70.52718814184231633 ) ) ;
#45235 = CYLINDRICAL_SURFACE ( 'NONE', #24292, 11.59999999999999964 ) ;
#45236 = EDGE_CURVE ( 'NONE', #8389, #42455, #44941, .T. ) ;
#45237 = CARTESIAN_POINT ( 'NONE',  ( 4.999999999999999112, 38.55633173627034438, -16.65560815589369881 ) ) ;
#45238 = VERTEX_POINT ( 'NONE', #13176 ) ;
#45239 = CARTESIAN_POINT ( 'NONE',  ( 0.000000000000000000, 81.50828551894240093, -8.966570791699810528 ) ) ;
#45240 = VERTEX_POINT ( 'NONE', #1442 ) ;
#45241 = CARTESIAN_POINT ( 'NONE',  ( 0.000000000000000000, -107.5000000000000000, -40.00000000000000711 ) ) ;
#45242 = CYLINDRICAL_SURFACE ( 'NONE', #26003, 16.00000000000000000 ) ;
#45243 = LINE ( 'NONE', #7562, #974 ) ;
#45244 = ORIENTED_EDGE ( 'NONE', *, *, #12459, .F. ) ;
#45245 = ORIENTED_EDGE ( 'NONE', *, *, #44263, .T. ) ;
#45246 = CIRCLE ( 'NONE', #19439, 31.99999999999998934 ) ;
#45248 = EDGE_CURVE ( 'NONE', #3496, #37278, #1193, .T. ) ;
#45247 = LINE ( 'NONE', #23447, #15717 ) ;
#45249 = CYLINDRICAL_SURFACE ( 'NONE', #46980, 77.49899999999999523 ) ;
#45250 = ORIENTED_EDGE ( 'NONE', *, *, #32367, .T. ) ;
#45251 = ORIENTED_EDGE ( 'NONE', *, *, #37310, .T. ) ;
#45252 = EDGE_CURVE ( 'NONE', #38854, #27962, #44175, .T. ) ;
#45253 = LINE ( 'NONE', #15406, #13489 ) ;
#45254 = EDGE_LOOP ( 'NONE', ( #18668, #40902, #14001, #34743 ) ) ;
#45255 = CYLINDRICAL_SURFACE ( 'NONE', #1916, 16.00000000000000000 ) ;
#45256 = CARTESIAN_POINT ( 'NONE',  ( -26.53422223201112828, -120.6595836127786043, 5.500000000000000000 ) ) ;
#45257 = CARTESIAN_POINT ( 'NONE',  ( 15.00000000000000000, 0.000000000000000000, 0.000000000000000000 ) ) ;
#45258 = DIRECTION ( 'NONE',  ( 1.000000000000000000, -0.000000000000000000, 0.000000000000000000 ) ) ;
#45259 = EDGE_CURVE ( 'NONE', #25953, #9753, #47281, .T. ) ;
#45260 = CARTESIAN_POINT ( 'NONE',  ( 10.00000000000000000, -21.32104025579091910, -30.84782396557241313 ) ) ;
#45261 = CARTESIAN_POINT ( 'NONE',  ( 10.00000000000000000, -73.73191006444561424, -14.66109333815538918 ) ) ;
#45262 = EDGE_CURVE ( 'NONE', #17289, #1183, #9491, .T. ) ;
#45263 = CARTESIAN_POINT ( 'NONE',  ( 0.000000000000000000, 0.000000000000000000, 0.000000000000000000 ) ) ;
#45264 = CARTESIAN_POINT ( 'NONE',  ( 0.000000000000000000, 68.67312586194995561, 35.91791733033500122 ) ) ;
#45265 = CIRCLE ( 'NONE', #42931, 82.00000000000000000 ) ;
#45266 = DIRECTION ( 'NONE',  ( -1.000000000000000000, 0.000000000000000000, 0.000000000000000000 ) ) ;
#45267 = ADVANCED_FACE ( 'NONE', ( #24422 ), #20762, .F. ) ;
#45268 = VECTOR ( 'NONE', #13141, 1000.000000000000000 ) ;
#45269 = DIRECTION ( 'NONE',  ( 0.000000000000000000, -0.7604059656000369261, 0.6494480483301767748 ) ) ;
#45270 = AXIS2_PLACEMENT_3D ( 'NONE', #4088, #3841, #45434 ) ;
#45271 = CARTESIAN_POINT ( 'NONE',  ( 0.000000000000000000, -77.16300072079681627, 27.74655509720641433 ) ) ;
#45272 = AXIS2_PLACEMENT_3D ( 'NONE', #33608, #3515, #7440 ) ;
#45273 = CARTESIAN_POINT ( 'NONE',  ( 10.00000000000000000, -41.81611651403859042, -3.925862922256606602 ) ) ;
#45274 = ORIENTED_EDGE ( 'NONE', *, *, #13217, .F. ) ;
#45275 = UNCERTAINTY_MEASURE_WITH_UNIT (LENGTH_MEASURE( 1.000000000000000082E-05 ), #16379, 'distance_accuracy_value', 'NONE');
#45276 = DIRECTION ( 'NONE',  ( 0.000000000000000000, 0.000000000000000000, 1.000000000000000000 ) ) ;
#45277 = FACE_OUTER_BOUND ( 'NONE', #5044, .T. ) ;
#45278 = FACE_OUTER_BOUND ( 'NONE', #20719, .T. ) ;
#45279 = VERTEX_POINT ( 'NONE', #20030 ) ;
#45280 = VERTEX_POINT ( 'NONE', #45746 ) ;
#45281 = DIRECTION ( 'NONE',  ( 0.000000000000000000, 0.000000000000000000, -1.000000000000000000 ) ) ;
#45282 = VERTEX_POINT ( 'NONE', #19774 ) ;
#45283 = ORIENTED_EDGE ( 'NONE', *, *, #22539, .F. ) ;
#45284 = VERTEX_POINT ( 'NONE', #2162 ) ;
#45285 = VECTOR ( 'NONE', #40927, 1000.000000000000000 ) ;
#45286 = DIRECTION ( 'NONE',  ( 0.000000000000000000, 0.000000000000000000, 1.000000000000000000 ) ) ;
#45288 = ORIENTED_EDGE ( 'NONE', *, *, #47799, .F. ) ;
#45287 = AXIS2_PLACEMENT_3D ( 'NONE', #32696, #43723, #28793 ) ;
#45289 = ORIENTED_EDGE ( 'NONE', *, *, #47705, .T. ) ;
#45290 = CARTESIAN_POINT ( 'NONE',  ( 0.000000000000000000, 79.10210256391368944, 21.60688246758614284 ) ) ;
#45291 = ORIENTED_EDGE ( 'NONE', *, *, #26258, .T. ) ;
#45292 = VECTOR ( 'NONE', #6050, 1000.000000000000000 ) ;
#45293 = CYLINDRICAL_SURFACE ( 'NONE', #30931, 82.00000000000000000 ) ;
#45294 = CARTESIAN_POINT ( 'NONE',  ( 10.00000000000000000, -8.966570791700142706, -81.50828551894234408 ) ) ;
#45295 = ORIENTED_EDGE ( 'NONE', *, *, #26568, .F. ) ;
#45296 = DIRECTION ( 'NONE',  ( 0.000000000000000000, 0.3090169943749482839, -0.9510565162951533091 ) ) ;
#45298 = ORIENTED_EDGE ( 'NONE', *, *, #6147, .F. ) ;
#45297 = DIRECTION ( 'NONE',  ( -1.000000000000000000, 0.000000000000000000, -0.000000000000000000 ) ) ;
#45299 = ORIENTED_EDGE ( 'NONE', *, *, #9160, .T. ) ;
#45300 = DIRECTION ( 'NONE',  ( -1.000000000000000000, 0.000000000000000000, 0.000000000000000000 ) ) ;
#45301 = VERTEX_POINT ( 'NONE', #27891 ) ;
#45302 = EDGE_CURVE ( 'NONE', #29936, #5335, #23700, .T. ) ;
#45303 = DIRECTION ( 'NONE',  ( 0.000000000000000000, 0.000000000000000000, -1.000000000000000000 ) ) ;
#45304 = CARTESIAN_POINT ( 'NONE',  ( 15.00000000000000000, 22.07842321921492612, 8.187992925817123790 ) ) ;
#45305 = ORIENTED_EDGE ( 'NONE', *, *, #13963, .T. ) ;
#45306 = DIRECTION ( 'NONE',  ( -1.000000000000000000, 0.000000000000000000, 0.000000000000000000 ) ) ;
#45307 = DIRECTION ( 'NONE',  ( -1.000000000000000000, 0.000000000000000000, 0.000000000000000000 ) ) ;
#45308 = DIRECTION ( 'NONE',  ( -1.000000000000000000, -0.000000000000000000, -0.000000000000000000 ) ) ;
#45309 = ADVANCED_FACE ( 'NONE', ( #12948 ), #8764, .T. ) ;
#45310 = DIRECTION ( 'NONE',  ( -1.000000000000000000, 0.000000000000000000, -0.000000000000000000 ) ) ;
#45311 = FACE_OUTER_BOUND ( 'NONE', #4728, .T. ) ;
#45312 = EDGE_CURVE ( 'NONE', #36574, #24182, #38657, .T. ) ;
#45313 = CYLINDRICAL_SURFACE ( 'NONE', #19265, 77.49899999999999523 ) ;
#45314 = ORIENTED_EDGE ( 'NONE', *, *, #42573, .T. ) ;
#45315 = CARTESIAN_POINT ( 'NONE',  ( -23.97194136764370498, -131.3950000906648938, -5.500000000000000000 ) ) ;
#45316 = DIRECTION ( 'NONE',  ( 0.000000000000000000, -0.5000000000000038858, -0.8660254037844363761 ) ) ;
#45317 = CARTESIAN_POINT ( 'NONE',  ( 12.50000000000000000, -132.5000000000000000, 40.00000000000000000 ) ) ;
#45318 = ADVANCED_FACE ( 'NONE', ( #12695 ), #12226, .T. ) ;
#45319 = EDGE_CURVE ( 'NONE', #42455, #43390, #31804, .T. ) ;
#45320 = DIRECTION ( 'NONE',  ( 0.000000000000000000, -0.8910065241883627918, -0.4539904997395568520 ) ) ;
#45321 = CARTESIAN_POINT ( 'NONE',  ( 10.00000000000000000, 0.000000000000000000, 0.000000000000000000 ) ) ;
#45322 = FACE_OUTER_BOUND ( 'NONE', #6588, .T. ) ;
#45323 = FACE_OUTER_BOUND ( 'NONE', #13420, .T. ) ;
#45324 = VERTEX_POINT ( 'NONE', #20506 ) ;
#45325 = CARTESIAN_POINT ( 'NONE',  ( 10.00000000000000000, 5.202137450156907761, -37.22597642581151689 ) ) ;
#45326 = ORIENTED_EDGE ( 'NONE', *, *, #29672, .F. ) ;
#45327 = DIRECTION ( 'NONE',  ( 0.000000000000000000, 0.000000000000000000, -1.000000000000000000 ) ) ;
#45328 = AXIS2_PLACEMENT_3D ( 'NONE', #12251, #42096, #45281 ) ;
#45329 = PRODUCT_CONTEXT ( 'NONE', #28226, 'mechanical' ) ;
#45330 = CARTESIAN_POINT ( 'NONE',  ( 10.00000000000000000, 59.03961581697465277, -46.53671651293886669 ) ) ;
#45331 = VERTEX_POINT ( 'NONE', #17079 ) ;
#45332 = AXIS2_PLACEMENT_3D ( 'NONE', #36738, #17898, #33557 ) ;
#45333 = FACE_OUTER_BOUND ( 'NONE', #22424, .T. ) ;
#45334 = VERTEX_POINT ( 'NONE', #16855 ) ;
#45335 = EDGE_CURVE ( 'NONE', #6202, #30049, #8523, .T. ) ;
#45336 = EDGE_CURVE ( 'NONE', #10873, #47251, #31693, .T. ) ;
#45337 = DIRECTION ( 'NONE',  ( 0.000000000000000000, 0.7071067811865439090, 0.7071067811865512365 ) ) ;
#45338 = EDGE_LOOP ( 'NONE', ( #2391, #43716, #24026, #17757 ) ) ;
#45339 = CARTESIAN_POINT ( 'NONE',  ( 0.000000000000000000, 34.94270380257639630, 74.18225833017899618 ) ) ;
#45341 = ORIENTED_EDGE ( 'NONE', *, *, #22409, .F. ) ;
#45340 = CARTESIAN_POINT ( 'NONE',  ( -10.00000000000000000, 0.000000000000000000, 0.000000000000000000 ) ) ;
#45342 = EDGE_CURVE ( 'NONE', #11474, #24209, #33630, .T. ) ;
#45343 = ORIENTED_EDGE ( 'NONE', *, *, #10454, .T. ) ;
#45344 = EDGE_CURVE ( 'NONE', #6863, #1013, #39621, .T. ) ;
#45345 = CARTESIAN_POINT ( 'NONE',  ( 10.00000000000000000, 0.000000000000000000, 0.000000000000000000 ) ) ;
#45346 = CARTESIAN_POINT ( 'NONE',  ( -7.670864526094549163, -97.73662565058241114, 5.500000000000000000 ) ) ;
#45347 = CARTESIAN_POINT ( 'NONE',  ( 0.000000000000000000, -8.966570791701281351, 81.50828551894224461 ) ) ;
#45348 = AXIS2_PLACEMENT_3D ( 'NONE', #126, #28797, #36383 ) ;
#45349 = DIRECTION ( 'NONE',  ( -1.000000000000000000, 0.000000000000000000, 0.000000000000000000 ) ) ;
#45350 = ORIENTED_EDGE ( 'NONE', *, *, #14765, .T. ) ;
#45351 = CIRCLE ( 'NONE', #5496, 82.00000000000000000 ) ;
#45352 = CARTESIAN_POINT ( 'NONE',  ( 10.00000000000000000, 21.53537804866126137, -30.80686688396986028 ) ) ;
#45353 = ORIENTED_EDGE ( 'NONE', *, *, #10737, .T. ) ;
#45354 = VERTEX_POINT ( 'NONE', #7206 ) ;
#45355 = CARTESIAN_POINT ( 'NONE',  ( 0.000000000000000000, 22.64427369931212297, -30.00120703465181293 ) ) ;
#45356 = VECTOR ( 'NONE', #27320, 1000.000000000000114 ) ;
#45357 = VECTOR ( 'NONE', #22302, 1000.000000000000000 ) ;
#45358 = CARTESIAN_POINT ( 'NONE',  ( 0.000000000000000000, 9.615535125379096826, -24.73947219025904687 ) ) ;
#45359 = DIRECTION ( 'NONE',  ( -1.000000000000000000, 0.000000000000000000, -0.000000000000000000 ) ) ;
#45360 = CARTESIAN_POINT ( 'NONE',  ( 0.000000000000000000, 0.000000000000000000, 0.000000000000000000 ) ) ;
#45361 = ORIENTED_EDGE ( 'NONE', *, *, #782, .F. ) ;
#45362 = DIRECTION ( 'NONE',  ( 1.000000000000000000, -0.000000000000000000, 0.000000000000000000 ) ) ;
#45363 = ADVANCED_FACE ( 'NONE', ( #11128 ), #17559, .T. ) ;
#45364 = DIRECTION ( 'NONE',  ( -1.000000000000000000, 0.000000000000000000, 0.000000000000000000 ) ) ;
#45365 = AXIS2_PLACEMENT_3D ( 'NONE', #13844, #43687, #2805 ) ;
#45366 = EDGE_CURVE ( 'NONE', #9989, #7974, #30874, .T. ) ;
#45367 = EDGE_CURVE ( 'NONE', #1493, #25865, #11385, .T. ) ;
#45368 = CARTESIAN_POINT ( 'NONE',  ( 19.29194287201271507, -133.5026271600380880, -2.500000000000000000 ) ) ;
#45369 = CIRCLE ( 'NONE', #3146, 82.00000000000000000 ) ;
#45370 = FACE_OUTER_BOUND ( 'NONE', #4495, .T. ) ;
#45371 = DIRECTION ( 'NONE',  ( -1.000000000000000000, 0.000000000000000000, 0.000000000000000000 ) ) ;
#45372 = AXIS2_PLACEMENT_3D ( 'NONE', #9071, #2203, #35007 ) ;
#45373 = LINE ( 'NONE', #34117, #22301 ) ;
#45374 = CARTESIAN_POINT ( 'NONE',  ( 0.000000000000000000, 0.000000000000000000, 0.000000000000000000 ) ) ;
#45375 = DIRECTION ( 'NONE',  ( 0.000000000000000000, 0.9876883405951372152, 0.1564344650402346160 ) ) ;
#45376 = DIRECTION ( 'NONE',  ( 1.000000000000000000, 0.000000000000000000, 0.000000000000000000 ) ) ;
#45377 = DIRECTION ( 'NONE',  ( 0.000000000000000000, 0.000000000000000000, 1.000000000000000000 ) ) ;
#45378 = LINE ( 'NONE', #15302, #37993 ) ;
#45379 = EDGE_CURVE ( 'NONE', #27354, #19209, #9756, .T. ) ;
#45380 = FACE_OUTER_BOUND ( 'NONE', #3076, .T. ) ;
#45381 = CARTESIAN_POINT ( 'NONE',  ( 6.782329983125267248, 10.49999999999999645, -105.0000000000000000 ) ) ;
#45382 = CYLINDRICAL_SURFACE ( 'NONE', #47387, 77.49899999999999523 ) ;
#45383 = ORIENTED_EDGE ( 'NONE', *, *, #21155, .T. ) ;
#45384 = DIRECTION ( 'NONE',  ( 1.000000000000000000, -0.000000000000000000, -0.000000000000000000 ) ) ;
#45385 = ORIENTED_EDGE ( 'NONE', *, *, #12305, .F. ) ;
#45386 = AXIS2_PLACEMENT_3D ( 'NONE', #21348, #36522, #17428 ) ;
#45387 = VECTOR ( 'NONE', #32477, 1000.000000000000000 ) ;
#45388 = ORIENTED_EDGE ( 'NONE', *, *, #861, .T. ) ;
#45389 = AXIS2_PLACEMENT_3D ( 'NONE', #4735, #46101, #13291 ) ;
#45390 = AXIS2_PLACEMENT_3D ( 'NONE', #10496, #43314, #25413 ) ;
#45391 = EDGE_LOOP ( 'NONE', ( #35166, #27193, #25583, #46863 ) ) ;
#45392 = DIRECTION ( 'NONE',  ( -1.000000000000000000, -0.000000000000000000, -0.000000000000000000 ) ) ;
#45393 = ORIENTED_EDGE ( 'NONE', *, *, #22409, .T. ) ;
#45394 = AXIS2_PLACEMENT_3D ( 'NONE', #746, #38705, #5167 ) ;
#45395 = CIRCLE ( 'NONE', #12603, 11.59999999999999787 ) ;
#45396 = ADVANCED_FACE ( 'NONE', ( #46949 ), #14803, .T. ) ;
#45397 = DIRECTION ( 'NONE',  ( 1.000000000000000000, 0.000000000000000000, 0.000000000000000000 ) ) ;
#45398 = AXIS2_PLACEMENT_3D ( 'NONE', #10259, #28859, #39892 ) ;
#45399 = CARTESIAN_POINT ( 'NONE',  ( 0.000000000000000000, 0.000000000000000000, 0.000000000000000000 ) ) ;
#45401 = ORIENTED_EDGE ( 'NONE', *, *, #42944, .F. ) ;
#45400 = LINE ( 'NONE', #23610, #23075 ) ;
#45402 = EDGE_CURVE ( 'NONE', #39044, #6346, #35543, .T. ) ;
#45403 = EDGE_LOOP ( 'NONE', ( #47430, #2578, #17744, #36903 ) ) ;
#45404 = DIRECTION ( 'NONE',  ( -1.000000000000000000, -0.000000000000000000, 0.000000000000000000 ) ) ;
#45405 = EDGE_LOOP ( 'NONE', ( #28189, #6168, #4596, #3205 ) ) ;
#45406 = EDGE_CURVE ( 'NONE', #4856, #15331, #22269, .T. ) ;
#45407 = ORIENTED_EDGE ( 'NONE', *, *, #27267, .F. ) ;
#45408 = CARTESIAN_POINT ( 'NONE',  ( -0.8815729230226008184, -93.47222532549339746, 5.500000000000000000 ) ) ;
#45409 = CARTESIAN_POINT ( 'NONE',  ( 0.000000000000000000, 0.000000000000000000, 0.000000000000000000 ) ) ;
#45410 = ORIENTED_EDGE ( 'NONE', *, *, #6188, .T. ) ;
#45411 = ORIENTED_EDGE ( 'NONE', *, *, #28363, .F. ) ;
#45412 = ORIENTED_EDGE ( 'NONE', *, *, #44650, .F. ) ;
#45413 = ORIENTED_EDGE ( 'NONE', *, *, #46106, .T. ) ;
#45414 = DIRECTION ( 'NONE',  ( -1.000000000000000000, 0.000000000000000000, -0.000000000000000000 ) ) ;
#45415 = ORIENTED_EDGE ( 'NONE', *, *, #46609, .F. ) ;
#45416 = CYLINDRICAL_SURFACE ( 'NONE', #16080, 31.99999999999998579 ) ;
#45417 = DIRECTION ( 'NONE',  ( -1.000000000000000000, -0.000000000000000000, -0.000000000000000000 ) ) ;
#45418 = DIRECTION ( 'NONE',  ( -0.9781476007338069101, 0.2079116908177532363, 0.000000000000000000 ) ) ;
#45419 = CARTESIAN_POINT ( 'NONE',  ( 6.377742925735834234, -145.7647898336708181, 5.500000000000000000 ) ) ;
#45420 = CARTESIAN_POINT ( 'NONE',  ( -10.43921258969510824, -98.89258801967538659, -2.500000000000000000 ) ) ;
#45421 = CARTESIAN_POINT ( 'NONE',  ( 0.000000000000000000, 37.58145647212453611, 16.68533520207917675 ) ) ;
#45422 = CYLINDRICAL_SURFACE ( 'NONE', #4115, 42.00000000000000000 ) ;
#45423 = ADVANCED_FACE ( 'NONE', ( #47184 ), #40996, .T. ) ;
#45424 = EDGE_CURVE ( 'NONE', #8618, #13986, #13659, .T. ) ;
#45425 = DIRECTION ( 'NONE',  ( 1.000000000000000000, -0.000000000000000000, -0.000000000000000000 ) ) ;
#45426 = CARTESIAN_POINT ( 'NONE',  ( 1.250000000000000000, -12.36245420541525597, -1.199999999999999956 ) ) ;
#45427 = ORIENTED_EDGE ( 'NONE', *, *, #12912, .F. ) ;
#45428 = VECTOR ( 'NONE', #36041, 999.9999999999998863 ) ;
#45429 = CARTESIAN_POINT ( 'NONE',  ( 0.000000000000000000, -64.81221759200306565, -50.23322058963418613 ) ) ;
#45430 = CARTESIAN_POINT ( 'NONE',  ( 10.00000000000000000, 0.000000000000000000, 0.000000000000000000 ) ) ;
#45431 = VERTEX_POINT ( 'NONE', #22391 ) ;
#45432 = VERTEX_POINT ( 'NONE', #28592 ) ;
#45433 = CIRCLE ( 'NONE', #24327, 32.00000000000000000 ) ;
#45434 = DIRECTION ( 'NONE',  ( 0.000000000000000000, 0.000000000000000000, 1.000000000000000000 ) ) ;
#45435 = AXIS2_PLACEMENT_3D ( 'NONE', #36205, #24722, #39164 ) ;
#45436 = AXIS2_PLACEMENT_3D ( 'NONE', #21697, #17287, #13393 ) ;
#45437 = CARTESIAN_POINT ( 'NONE',  ( 0.000000000000000000, -76.66974797899844418, 11.30684508768314522 ) ) ;
#45438 = DIRECTION ( 'NONE',  ( -1.000000000000000000, 0.000000000000000000, 0.000000000000000000 ) ) ;
#45439 = CARTESIAN_POINT ( 'NONE',  ( 10.00000000000000000, -22.74946021919153694, 29.81001611431000597 ) ) ;
#45440 = VECTOR ( 'NONE', #41347, 1000.000000000000000 ) ;
#45441 = CARTESIAN_POINT ( 'NONE',  ( -14.87942725330654348, -141.9795960975983178, 5.500000000000000000 ) ) ;
#45442 = CARTESIAN_POINT ( 'NONE',  ( 0.000000000000000000, 0.000000000000000000, 0.000000000000000000 ) ) ;
#45443 = ADVANCED_FACE ( 'NONE', ( #36157 ), #22135, .T. ) ;
#45444 = CYLINDRICAL_SURFACE ( 'NONE', #16161, 77.49899999999999523 ) ;
#45445 = LINE ( 'NONE', #887, #1404 ) ;
#45446 = AXIS2_PLACEMENT_3D ( 'NONE', #14956, #22540, #44808 ) ;
#45447 = DIRECTION ( 'NONE',  ( -1.000000000000000000, -0.000000000000000000, -0.000000000000000000 ) ) ;
#45448 = ORIENTED_EDGE ( 'NONE', *, *, #44960, .T. ) ;
#45449 = ORIENTED_EDGE ( 'NONE', *, *, #8963, .F. ) ;
#45450 = ORIENTED_EDGE ( 'NONE', *, *, #12109, .F. ) ;
#45451 = ORIENTED_EDGE ( 'NONE', *, *, #44897, .F. ) ;
#45452 = DIRECTION ( 'NONE',  ( 0.000000000000000000, 0.000000000000000000, 1.000000000000000000 ) ) ;
#45453 = DIRECTION ( 'NONE',  ( -1.000000000000000000, 0.000000000000000000, 0.000000000000000000 ) ) ;
#45454 = ORIENTED_EDGE ( 'NONE', *, *, #29102, .T. ) ;
#45455 = CIRCLE ( 'NONE', #7168, 32.00000000000000000 ) ;
#45456 = AXIS2_PLACEMENT_3D ( 'NONE', #28514, #7908, #15025 ) ;
#45457 = FACE_OUTER_BOUND ( 'NONE', #21519, .T. ) ;
#45458 = VECTOR ( 'NONE', #3448, 1000.000000000000000 ) ;
#45459 = VERTEX_POINT ( 'NONE', #48323 ) ;
#45460 = EDGE_CURVE ( 'NONE', #21369, #13195, #43521, .T. ) ;
#45461 = ORIENTED_EDGE ( 'NONE', *, *, #8008, .T. ) ;
#45462 = VECTOR ( 'NONE', #31238, 1000.000000000000000 ) ;
#45463 = EDGE_CURVE ( 'NONE', #36456, #21451, #22620, .T. ) ;
#45464 = VECTOR ( 'NONE', #7750, 1000.000000000000000 ) ;
#45465 = DIRECTION ( 'NONE',  ( 0.000000000000000000, 0.000000000000000000, 1.000000000000000000 ) ) ;
#45466 = DIRECTION ( 'NONE',  ( 0.000000000000000000, 0.3090169943749580539, -0.9510565162951499785 ) ) ;
#45467 = CYLINDRICAL_SURFACE ( 'NONE', #32878, 31.99999999999999289 ) ;
#45468 = VERTEX_POINT ( 'NONE', #2614 ) ;
#45469 = CARTESIAN_POINT ( 'NONE',  ( 0.000000000000000000, -10.30890764327441822, 81.34940948281332851 ) ) ;
#45470 = ADVANCED_FACE ( 'NONE', ( #32501 ), #47427, .T. ) ;
#45471 = ORIENTED_EDGE ( 'NONE', *, *, #32332, .T. ) ;
#45472 = ORIENTED_EDGE ( 'NONE', *, *, #23984, .F. ) ;
#45473 = FACE_OUTER_BOUND ( 'NONE', #37399, .T. ) ;
#45474 = AXIS2_PLACEMENT_3D ( 'NONE', #5573, #9241, #20489 ) ;
#45475 = DIRECTION ( 'NONE',  ( 0.000000000000000000, 0.9969173337331276308, 0.07845909572784864894 ) ) ;
#45476 = FACE_OUTER_BOUND ( 'NONE', #4381, .T. ) ;
#45477 = ORIENTED_EDGE ( 'NONE', *, *, #40567, .T. ) ;
#45478 = EDGE_LOOP ( 'NONE', ( #22043, #10680, #42474, #6067 ) ) ;
#45479 = EDGE_CURVE ( 'NONE', #48002, #5896, #27799, .T. ) ;
#45480 = CARTESIAN_POINT ( 'NONE',  ( 0.000000000000000000, -10.30890764327441289, 81.34940948281332851 ) ) ;
#45481 = DIRECTION ( 'NONE',  ( 0.1276937514489679404, 0.9918136447140103451, 0.000000000000000000 ) ) ;
#45482 = ORIENTED_EDGE ( 'NONE', *, *, #5378, .F. ) ;
#45483 = EDGE_CURVE ( 'NONE', #18791, #46639, #23579, .T. ) ;
#45484 = DIRECTION ( 'NONE',  ( 0.000000000000000000, 0.000000000000000000, 1.000000000000000000 ) ) ;
#45485 = ORIENTED_EDGE ( 'NONE', *, *, #37871, .F. ) ;
#45486 = DIRECTION ( 'NONE',  ( 0.000000000000000000, 1.000000000000000000, 3.491481338843133355E-15 ) ) ;
#45487 = DIRECTION ( 'NONE',  ( -1.000000000000000000, 0.000000000000000000, -0.000000000000000000 ) ) ;
#45488 = DIRECTION ( 'NONE',  ( 0.000000000000000000, 0.000000000000000000, 1.000000000000000000 ) ) ;
#45489 = CARTESIAN_POINT ( 'NONE',  ( 0.000000000000000000, -16.65972982744877484, -80.28980883073775487 ) ) ;
#45490 = DIRECTION ( 'NONE',  ( -1.000000000000000000, -0.000000000000000000, 0.000000000000000000 ) ) ;
#45491 = CARTESIAN_POINT ( 'NONE',  ( 10.00000000000000000, 0.000000000000000000, 0.000000000000000000 ) ) ;
#45492 = FACE_OUTER_BOUND ( 'NONE', #31341, .T. ) ;
#45493 = EDGE_CURVE ( 'NONE', #7237, #41154, #41711, .T. ) ;
#45494 = DIRECTION ( 'NONE',  ( 0.000000000000000000, 0.1564344650402311743, -0.9876883405951376593 ) ) ;
#45495 = CARTESIAN_POINT ( 'NONE',  ( 11.41210121379328335, -99.40233154247455616, 2.500000000000000000 ) ) ;
#45496 = AXIS2_PLACEMENT_3D ( 'NONE', #24227, #35002, #2199 ) ;
#45497 = DIRECTION ( 'NONE',  ( -1.000000000000000000, 0.000000000000000000, 0.000000000000000000 ) ) ;
#45498 = LINE ( 'NONE', #16557, #29308 ) ;
#45499 = DIRECTION ( 'NONE',  ( -1.000000000000000000, 0.000000000000000000, 0.000000000000000000 ) ) ;
#45500 = AXIS2_PLACEMENT_3D ( 'NONE', #25079, #28050, #13846 ) ;
#45501 = ORIENTED_EDGE ( 'NONE', *, *, #4171, .T. ) ;
#45502 = EDGE_CURVE ( 'NONE', #19364, #32361, #16259, .T. ) ;
#45503 = LINE ( 'NONE', #42088, #6594 ) ;
#45504 = AXIS2_PLACEMENT_3D ( 'NONE', #12903, #27841, #43229 ) ;
#45505 = DIRECTION ( 'NONE',  ( -1.000000000000000000, 0.000000000000000000, 0.000000000000000000 ) ) ;
#45506 = DIRECTION ( 'NONE',  ( 0.000000000000000000, 0.7604059656000277112, 0.6494480483301875440 ) ) ;
#45507 = AXIS2_PLACEMENT_3D ( 'NONE', #27895, #42810, #39128 ) ;
#45508 = VERTEX_POINT ( 'NONE', #18930 ) ;
#45509 = ORIENTED_EDGE ( 'NONE', *, *, #1495, .F. ) ;
#45510 = EDGE_CURVE ( 'NONE', #24990, #11779, #9030, .T. ) ;
#45511 = DIRECTION ( 'NONE',  ( 0.000000000000000000, 0.4539904997395476927, -0.8910065241883674547 ) ) ;
#45512 = ORIENTED_EDGE ( 'NONE', *, *, #44587, .T. ) ;
#45513 = EDGE_CURVE ( 'NONE', #33738, #42694, #34844, .T. ) ;
#45514 = ORIENTED_EDGE ( 'NONE', *, *, #26197, .F. ) ;
#45515 = ORIENTED_EDGE ( 'NONE', *, *, #22195, .T. ) ;
#45516 = ORIENTED_EDGE ( 'NONE', *, *, #11751, .T. ) ;
#45517 = ADVANCED_FACE ( 'NONE', ( #8417 ), #27271, .T. ) ;
#45518 = VECTOR ( 'NONE', #30406, 1000.000000000000114 ) ;
#45519 = VECTOR ( 'NONE', #42363, 1000.000000000000000 ) ;
#45520 = CARTESIAN_POINT ( 'NONE',  ( 0.000000000000000000, 22.64427369931212297, -30.00120703465181293 ) ) ;
#45521 = VERTEX_POINT ( 'NONE', #22859 ) ;
#45522 = LINE ( 'NONE', #22365, #27852 ) ;
#45523 = EDGE_CURVE ( 'NONE', #35361, #46530, #32471, .T. ) ;
#45524 = ORIENTED_EDGE ( 'NONE', *, *, #42839, .T. ) ;
#45525 = DIRECTION ( 'NONE',  ( 1.000000000000000000, 0.000000000000000000, 0.000000000000000000 ) ) ;
#45526 = ORIENTED_EDGE ( 'NONE', *, *, #14746, .F. ) ;
#45527 = AXIS2_PLACEMENT_3D ( 'NONE', #11234, #41104, #7561 ) ;
#45528 = DIRECTION ( 'NONE',  ( -1.000000000000000000, -0.000000000000000000, -0.000000000000000000 ) ) ;
#45529 = CYLINDRICAL_SURFACE ( 'NONE', #37705, 16.00000000000000355 ) ;
#45530 = AXIS2_PLACEMENT_3D ( 'NONE', #31434, #39242, #33021 ) ;
#45531 = ORIENTED_EDGE ( 'NONE', *, *, #10454, .F. ) ;
#45532 = LINE ( 'NONE', #38701, #40753 ) ;
#45533 = ORIENTED_EDGE ( 'NONE', *, *, #1678, .T. ) ;
#45534 = CARTESIAN_POINT ( 'NONE',  ( 10.00000000000000000, 36.73666225445988687, -65.58780272294035285 ) ) ;
#45535 = DIRECTION ( 'NONE',  ( -1.000000000000000000, -0.000000000000000000, -0.000000000000000000 ) ) ;
#45536 = VERTEX_POINT ( 'NONE', #38523 ) ;
#45537 = VECTOR ( 'NONE', #16302, 1000.000000000000114 ) ;
#45538 = DIRECTION ( 'NONE',  ( -1.000000000000000000, 0.000000000000000000, 0.000000000000000000 ) ) ;
#45539 = ORIENTED_EDGE ( 'NONE', *, *, #23713, .F. ) ;
#45540 = CARTESIAN_POINT ( 'NONE',  ( 12.00000000000000000, -22.32062822937488988, -14.36278369418800160 ) ) ;
#45541 = CARTESIAN_POINT ( 'NONE',  ( 11.99999999999999822, 0.000000000000000000, 0.000000000000000000 ) ) ;
#45542 = VECTOR ( 'NONE', #45384, 1000.000000000000000 ) ;
#45543 = DIRECTION ( 'NONE',  ( -0.1850432970638667129, 0.9827303690289281857, 0.000000000000000000 ) ) ;
#45544 = FACE_OUTER_BOUND ( 'NONE', #18627, .T. ) ;
#45545 = DIRECTION ( 'NONE',  ( -1.000000000000000000, -0.000000000000000000, -0.000000000000000000 ) ) ;
#45546 = DIRECTION ( 'NONE',  ( -1.000000000000000000, 0.000000000000000000, 0.000000000000000000 ) ) ;
#45547 = CARTESIAN_POINT ( 'NONE',  ( 21.07894319797337701, -103.8699611390234878, 5.500000000000000000 ) ) ;
#45548 = CARTESIAN_POINT ( 'NONE',  ( 10.00000000000000000, 37.58145647212453611, 16.68533520207917675 ) ) ;
#45549 = VERTEX_POINT ( 'NONE', #23344 ) ;
#45550 = DIRECTION ( 'NONE',  ( -0.9435911131814398445, 0.3311129884571295534, 0.000000000000000000 ) ) ;
#45551 = DIRECTION ( 'NONE',  ( -1.000000000000000000, -0.000000000000000000, 0.000000000000000000 ) ) ;
#45552 = DIRECTION ( 'NONE',  ( -1.000000000000000000, 0.000000000000000000, 0.000000000000000000 ) ) ;
#45553 = EDGE_LOOP ( 'NONE', ( #31212, #777, #16877, #3275 ) ) ;
#45554 = DIRECTION ( 'NONE',  ( -1.000000000000000000, -0.000000000000000000, 0.000000000000000000 ) ) ;
#45555 = CARTESIAN_POINT ( 'NONE',  ( 0.000000000000000000, 0.000000000000000000, 0.000000000000000000 ) ) ;
#45557 = CONICAL_SURFACE ( 'NONE', #46339, 13.71319123046128752, 0.2094395102393127317 ) ;
#45556 = FILL_AREA_STYLE_COLOUR ( '', #35799 ) ;
#45558 = DIRECTION ( 'NONE',  ( 0.000000000000000000, 0.000000000000000000, 1.000000000000000000 ) ) ;
#45559 = ORIENTED_EDGE ( 'NONE', *, *, #6749, .T. ) ;
#45560 = VECTOR ( 'NONE', #47013, 1000.000000000000000 ) ;
#45561 = VERTEX_POINT ( 'NONE', #34344 ) ;
#45562 = VECTOR ( 'NONE', #11781, 1000.000000000000000 ) ;
#45563 = FACE_BOUND ( 'NONE', #44498, .T. ) ;
#45564 = ORIENTED_EDGE ( 'NONE', *, *, #37346, .T. ) ;
#45565 = DIRECTION ( 'NONE',  ( -1.000000000000000000, -0.000000000000000000, 0.000000000000000000 ) ) ;
#45566 = AXIS2_PLACEMENT_3D ( 'NONE', #29301, #2605, #32720 ) ;
#45567 = CIRCLE ( 'NONE', #11319, 31.99999999999999645 ) ;
#45568 = ORIENTED_EDGE ( 'NONE', *, *, #6143, .T. ) ;
#45569 = AXIS2_PLACEMENT_3D ( 'NONE', #37905, #19291, #42062 ) ;
#45570 = CARTESIAN_POINT ( 'NONE',  ( -10.00000000000000000, 0.000000000000000000, 0.000000000000000000 ) ) ;
#45571 = AXIS2_PLACEMENT_3D ( 'NONE', #31313, #8527, #46479 ) ;
#45572 = ORIENTED_EDGE ( 'NONE', *, *, #18560, .T. ) ;
#45573 = AXIS2_PLACEMENT_3D ( 'NONE', #33397, #40504, #10393 ) ;
#45574 = ADVANCED_FACE ( 'NONE', ( #23110 ), #30954, .F. ) ;
#45575 = AXIS2_PLACEMENT_3D ( 'NONE', #15971, #30911, #22581 ) ;
#45576 = CARTESIAN_POINT ( 'NONE',  ( -3.000000000000000000, 16.83928648764945279, -16.46020748918028076 ) ) ;
#45577 = ORIENTED_EDGE ( 'NONE', *, *, #22147, .F. ) ;
#45578 = EDGE_CURVE ( 'NONE', #38615, #4357, #16052, .T. ) ;
#45579 = PLANE ( 'NONE',  #3440 ) ;
#45580 = EDGE_LOOP ( 'NONE', ( #10287, #46659, #1413, #32936 ) ) ;
#45581 = EDGE_CURVE ( 'NONE', #361, #697, #45373, .T. ) ;
#45582 = DIRECTION ( 'NONE',  ( -1.000000000000000000, 0.000000000000000000, 0.000000000000000000 ) ) ;
#45584 = VERTEX_POINT ( 'NONE', #4989 ) ;
#45583 = DIRECTION ( 'NONE',  ( 0.000000000000000000, 0.000000000000000000, 1.000000000000000000 ) ) ;
#45585 = EDGE_LOOP ( 'NONE', ( #27604, #30936, #328, #20813 ) ) ;
#45586 = EDGE_CURVE ( 'NONE', #35673, #21593, #820, .T. ) ;
#45587 = VECTOR ( 'NONE', #17869, 1000.000000000000000 ) ;
#45588 = ORIENTED_EDGE ( 'NONE', *, *, #25908, .F. ) ;
#45589 = DIRECTION ( 'NONE',  ( 0.000000000000000000, -0.9876883405951359940, -0.1564344650402420267 ) ) ;
#45590 = DIRECTION ( 'NONE',  ( 0.000000000000000000, -0.8090169943749403458, -0.5877852522924830181 ) ) ;
#45591 = CARTESIAN_POINT ( 'NONE',  ( 0.000000000000000000, 0.000000000000000000, 0.000000000000000000 ) ) ;
#45592 = TOROIDAL_SURFACE ( 'NONE', #24501, 20.69999999999999929, 0.2999999999999981570 ) ;
#45593 = CARTESIAN_POINT ( 'NONE',  ( 10.00000000000000000, 0.000000000000000000, 0.000000000000000000 ) ) ;
#45594 = EDGE_LOOP ( 'NONE', ( #19513, #37407, #13283, #23697 ) ) ;
#45595 = LINE ( 'NONE', #4014, #6045 ) ;
#45596 = ORIENTED_EDGE ( 'NONE', *, *, #1069, .F. ) ;
#45597 = ORIENTED_EDGE ( 'NONE', *, *, #4210, .T. ) ;
#45598 = AXIS2_PLACEMENT_3D ( 'NONE', #41465, #33863, #18692 ) ;
#45599 = DIRECTION ( 'NONE',  ( 0.000000000000000000, 0.000000000000000000, 1.000000000000000000 ) ) ;
#45600 = CIRCLE ( 'NONE', #22930, 82.00000000000000000 ) ;
#45601 = AXIS2_PLACEMENT_3D ( 'NONE', #38850, #35151, #34188 ) ;
#45602 = EDGE_CURVE ( 'NONE', #3020, #46849, #11614, .T. ) ;
#45603 = CARTESIAN_POINT ( 'NONE',  ( 0.000000000000000000, -11.95096189432312350, -23.69967320028773372 ) ) ;
#45604 = CIRCLE ( 'NONE', #3380, 31.99999999999998579 ) ;
#45605 = CARTESIAN_POINT ( 'NONE',  ( -2.499999999999997780, 8.494897427831771708, -19.01812422950394676 ) ) ;
#45606 = LINE ( 'NONE', #29711, #28210 ) ;
#45607 = ORIENTED_EDGE ( 'NONE', *, *, #38021, .T. ) ;
#45608 = CARTESIAN_POINT ( 'NONE',  ( 11.99999999999999822, 0.000000000000000000, 77.49899999999999523 ) ) ;
#45609 = AXIS2_PLACEMENT_3D ( 'NONE', #21953, #18534, #26120 ) ;
#45610 = DIRECTION ( 'NONE',  ( 0.000000000000000000, 0.000000000000000000, 1.000000000000000000 ) ) ;
#45611 = CARTESIAN_POINT ( 'NONE',  ( 0.000000000000000000, 4.992566952384984269, 37.16516213103279398 ) ) ;
#45612 = CYLINDRICAL_SURFACE ( 'NONE', #6412, 82.00000000000000000 ) ;
#45613 = CARTESIAN_POINT ( 'NONE',  ( 0.000000000000000000, 33.71516098798849015, -74.74816331893393340 ) ) ;
#45614 = VECTOR ( 'NONE', #43290, 1000.000000000000000 ) ;
#45615 = VECTOR ( 'NONE', #18936, 1000.000000000000000 ) ;
#45616 = CARTESIAN_POINT ( 'NONE',  ( 15.00000000000000000, 23.49999999999999645, -1.500000000000003997 ) ) ;
#45617 = CARTESIAN_POINT ( 'NONE',  ( 11.99999999999999822, -75.54627589209931671, -17.28742895386162814 ) ) ;
#45618 = CARTESIAN_POINT ( 'NONE',  ( 0.000000000000000000, 31.52238457039637609, -27.75498641678709788 ) ) ;
#45619 = CIRCLE ( 'NONE', #21400, 15.99999999999999822 ) ;
#45620 = LINE ( 'NONE', #30696, #28342 ) ;
#45621 = CARTESIAN_POINT ( 'NONE',  ( 0.000000000000000000, 0.000000000000000000, 0.000000000000000000 ) ) ;
#45622 = AXIS2_PLACEMENT_3D ( 'NONE', #8922, #20914, #20412 ) ;
#45623 = VERTEX_POINT ( 'NONE', #19907 ) ;
#45624 = LINE ( 'NONE', #41719, #31760 ) ;
#45625 = EDGE_CURVE ( 'NONE', #32554, #6182, #9786, .T. ) ;
#45626 = DIRECTION ( 'NONE',  ( 0.000000000000000000, 0.8090169943749445647, 0.5877852522924770229 ) ) ;
#45627 = PLANE ( 'NONE',  #47215 ) ;
#45628 = VERTEX_POINT ( 'NONE', #593 ) ;
#45629 = ORIENTED_EDGE ( 'NONE', *, *, #7745, .F. ) ;
#45630 = EDGE_CURVE ( 'NONE', #45913, #42163, #15523, .T. ) ;
#45631 = EDGE_CURVE ( 'NONE', #36257, #27089, #6692, .T. ) ;
#45632 = DIRECTION ( 'NONE',  ( 0.000000000000000000, 1.000000000000000000, 3.491481338843133355E-15 ) ) ;
#45633 = EDGE_LOOP ( 'NONE', ( #38542, #43087, #27890, #40981 ) ) ;
#45634 = AXIS2_PLACEMENT_3D ( 'NONE', #1576, #31445, #2516 ) ;
#45635 = AXIS2_PLACEMENT_3D ( 'NONE', #22734, #33505, #14914 ) ;
#45636 = CIRCLE ( 'NONE', #14380, 77.49899999999999523 ) ;
#45637 = CIRCLE ( 'NONE', #24545, 31.99999999999998579 ) ;
#45638 = VERTEX_POINT ( 'NONE', #27033 ) ;
#45639 = ORIENTED_EDGE ( 'NONE', *, *, #32874, .F. ) ;
#45640 = DIRECTION ( 'NONE',  ( 0.000000000000000000, 0.000000000000000000, 1.000000000000000000 ) ) ;
#45642 = EDGE_CURVE ( 'NONE', #526, #31086, #41967, .T. ) ;
#45641 = EDGE_LOOP ( 'NONE', ( #6648, #23940, #28387, #23935 ) ) ;
#45643 = VERTEX_POINT ( 'NONE', #13791 ) ;
#45644 = EDGE_CURVE ( 'NONE', #31959, #39227, #12957, .T. ) ;
#45645 = EDGE_CURVE ( 'NONE', #6291, #441, #31724, .T. ) ;
#45646 = AXIS2_PLACEMENT_3D ( 'NONE', #8734, #25949, #16570 ) ;
#45647 = LINE ( 'NONE', #12369, #13641 ) ;
#45648 = CYLINDRICAL_SURFACE ( 'NONE', #731, 37.49900000000000233 ) ;
#45649 = VECTOR ( 'NONE', #22525, 1000.000000000000000 ) ;
#45652 = ORIENTED_EDGE ( 'NONE', *, *, #4809, .T. ) ;
#45651 = DIRECTION ( 'NONE',  ( -1.000000000000000000, -0.000000000000000000, -0.000000000000000000 ) ) ;
#45650 = AXIS2_PLACEMENT_3D ( 'NONE', #25613, #21710, #40557 ) ;
#45653 = ORIENTED_EDGE ( 'NONE', *, *, #29147, .F. ) ;
#45654 = DIRECTION ( 'NONE',  ( -1.000000000000000000, 0.000000000000000000, 0.000000000000000000 ) ) ;
#45655 = EDGE_CURVE ( 'NONE', #41264, #47615, #42924, .T. ) ;
#45656 = VERTEX_POINT ( 'NONE', #9609 ) ;
#45657 = ORIENTED_EDGE ( 'NONE', *, *, #46084, .F. ) ;
#45658 = AXIS2_PLACEMENT_3D ( 'NONE', #16938, #46568, #46317 ) ;
#45659 = DIRECTION ( 'NONE',  ( -1.000000000000000000, 0.000000000000000000, 0.000000000000000000 ) ) ;
#45660 = FACE_OUTER_BOUND ( 'NONE', #20696, .T. ) ;
#45661 = ORIENTED_EDGE ( 'NONE', *, *, #37459, .T. ) ;
#45662 = ORIENTED_EDGE ( 'NONE', *, *, #12305, .T. ) ;
#45663 = CYLINDRICAL_SURFACE ( 'NONE', #13068, 31.99999999999999289 ) ;
#45664 = ORIENTED_EDGE ( 'NONE', *, *, #44542, .T. ) ;
#45665 = CARTESIAN_POINT ( 'NONE',  ( 0.000000000000000000, -0.9646360437375309793, 23.52805723605590416 ) ) ;
#45666 = EDGE_CURVE ( 'NONE', #20, #46331, #42648, .T. ) ;
#45667 = DIRECTION ( 'NONE',  ( 0.000000000000000000, 0.000000000000000000, 1.000000000000000000 ) ) ;
#45668 = DIRECTION ( 'NONE',  ( -1.000000000000000000, 0.000000000000000000, 0.000000000000000000 ) ) ;
#45669 = DIRECTION ( 'NONE',  ( -0.000000000000000000, -0.000000000000000000, -1.000000000000000000 ) ) ;
#45670 = LINE ( 'NONE', #865, #33690 ) ;
#45671 = DIRECTION ( 'NONE',  ( -1.000000000000000000, 0.000000000000000000, 0.000000000000000000 ) ) ;
#45672 = FACE_OUTER_BOUND ( 'NONE', #1464, .T. ) ;
#45673 = CARTESIAN_POINT ( 'NONE',  ( 11.99999999999999822, -51.03279382321048985, -55.19960302592120627 ) ) ;
#45674 = CARTESIAN_POINT ( 'NONE',  ( 0.000000000000000000, -2.946379043146863719, 75.11764819372146462 ) ) ;
#45675 = DIRECTION ( 'NONE',  ( 0.000000000000000000, 0.000000000000000000, 1.000000000000000000 ) ) ;
#45676 = AXIS2_PLACEMENT_3D ( 'NONE', #5175, #42620, #35745 ) ;
#45677 = FACE_OUTER_BOUND ( 'NONE', #41922, .T. ) ;
#45678 = VERTEX_POINT ( 'NONE', #24312 ) ;
#45679 = ORIENTED_EDGE ( 'NONE', *, *, #4651, .T. ) ;
#45680 = DIRECTION ( 'NONE',  ( -1.000000000000000000, -0.000000000000000000, -0.000000000000000000 ) ) ;
#45681 = VECTOR ( 'NONE', #35621, 1000.000000000000000 ) ;
#45682 = AXIS2_PLACEMENT_3D ( 'NONE', #14027, #28950, #43887 ) ;
#45683 = PLANE ( 'NONE',  #16806 ) ;
#45684 = AXIS2_PLACEMENT_3D ( 'NONE', #10572, #46814, #25483 ) ;
#45685 = DIRECTION ( 'NONE',  ( 1.000000000000000000, -0.000000000000000000, -0.000000000000000000 ) ) ;
#45686 = DIRECTION ( 'NONE',  ( -1.000000000000000000, -0.000000000000000000, 0.000000000000000000 ) ) ;
#45687 = EDGE_CURVE ( 'NONE', #25899, #16268, #1202, .T. ) ;
#45688 = CARTESIAN_POINT ( 'NONE',  ( -17.26469406256017791, -140.1601175325492648, -5.500000000000000000 ) ) ;
#45689 = CARTESIAN_POINT ( 'NONE',  ( 10.00000000000000000, 30.80686688397010542, 21.53537804866092387 ) ) ;
#45690 = ORIENTED_EDGE ( 'NONE', *, *, #5365, .F. ) ;
#45691 = EDGE_CURVE ( 'NONE', #22548, #20595, #16735, .T. ) ;
#45692 = CIRCLE ( 'NONE', #15992, 82.00000000000000000 ) ;
#45693 = CIRCLE ( 'NONE', #25378, 37.49900000000000944 ) ;
#45694 = CARTESIAN_POINT ( 'NONE',  ( 1.250000000000000000, -12.36245420541525597, -1.199999999999999956 ) ) ;
#45695 = DIRECTION ( 'NONE',  ( -1.000000000000000000, -0.000000000000000000, -0.000000000000000000 ) ) ;
#45696 = AXIS2_PLACEMENT_3D ( 'NONE', #36430, #36894, #29566 ) ;
#45697 = EDGE_CURVE ( 'NONE', #12035, #43548, #10608, .T. ) ;
#45698 = ORIENTED_EDGE ( 'NONE', *, *, #9005, .F. ) ;
#45699 = SURFACE_STYLE_FILL_AREA ( #22468 ) ;
#45700 = EDGE_CURVE ( 'NONE', #14857, #1751, #37950, .T. ) ;
#45701 = DIRECTION ( 'NONE',  ( 0.000000000000000000, 0.000000000000000000, 1.000000000000000000 ) ) ;
#45702 = AXIS2_PLACEMENT_3D ( 'NONE', #18525, #33922, #41525 ) ;
#45703 = ORIENTED_EDGE ( 'NONE', *, *, #23190, .T. ) ;
#45704 = ORIENTED_EDGE ( 'NONE', *, *, #9280, .T. ) ;
#45705 = EDGE_LOOP ( 'NONE', ( #38361, #4253, #31568, #6216 ) ) ;
#45706 = ORIENTED_EDGE ( 'NONE', *, *, #39943, .T. ) ;
#45707 = ORIENTED_EDGE ( 'NONE', *, *, #16425, .F. ) ;
#45708 = EDGE_LOOP ( 'NONE', ( #16391, #7953, #11705, #31337 ) ) ;
#45709 = FACE_OUTER_BOUND ( 'NONE', #32519, .T. ) ;
#45710 = EDGE_LOOP ( 'NONE', ( #14478, #2428, #25954, #5375 ) ) ;
#45711 = EDGE_CURVE ( 'NONE', #8653, #36574, #5125, .T. ) ;
#45712 = EDGE_CURVE ( 'NONE', #14617, #925, #28557, .T. ) ;
#45713 = ORIENTED_EDGE ( 'NONE', *, *, #2288, .T. ) ;
#45714 = AXIS2_PLACEMENT_3D ( 'NONE', #5117, #42804, #39364 ) ;
#45715 = CARTESIAN_POINT ( 'NONE',  ( 10.00000000000000000, 0.000000000000000000, 0.000000000000000000 ) ) ;
#45716 = AXIS2_PLACEMENT_3D ( 'NONE', #33896, #41497, #34369 ) ;
#45717 = VERTEX_POINT ( 'NONE', #20636 ) ;
#45718 = VERTEX_POINT ( 'NONE', #9866 ) ;
#45719 = ORIENTED_EDGE ( 'NONE', *, *, #23214, .T. ) ;
#45720 = CARTESIAN_POINT ( 'NONE',  ( 10.00000000000000000, 35.95386929396241271, 10.96151621346552751 ) ) ;
#45721 = EDGE_CURVE ( 'NONE', #20063, #5905, #17194, .T. ) ;
#45722 = DIRECTION ( 'NONE',  ( 0.000000000000000000, 0.8910065241883691201, -0.4539904997395446951 ) ) ;
#45723 = CARTESIAN_POINT ( 'NONE',  ( 10.00000000000000000, 0.000000000000000000, 0.000000000000000000 ) ) ;
#45724 = VERTEX_POINT ( 'NONE', #24799 ) ;
#45725 = VECTOR ( 'NONE', #30427, 1000.000000000000114 ) ;
#45726 = AXIS2_PLACEMENT_3D ( 'NONE', #21424, #13606, #17755 ) ;
#45727 = ORIENTED_EDGE ( 'NONE', *, *, #46665, .T. ) ;
#45728 = DIRECTION ( 'NONE',  ( -1.000000000000000000, 0.000000000000000000, 0.000000000000000000 ) ) ;
#45729 = VERTEX_POINT ( 'NONE', #35576 ) ;
#45730 = ORIENTED_EDGE ( 'NONE', *, *, #29086, .F. ) ;
#45731 = CARTESIAN_POINT ( 'NONE',  ( 10.00000000000000000, -41.76937507738831812, 62.50329211542423025 ) ) ;
#45732 = CARTESIAN_POINT ( 'NONE',  ( 14.59956846177685996, -138.4757300459248484, 2.500000000000000000 ) ) ;
#45733 = ORIENTED_EDGE ( 'NONE', *, *, #10789, .T. ) ;
#45734 = CIRCLE ( 'NONE', #48101, 37.49900000000000944 ) ;
#45735 = CARTESIAN_POINT ( 'NONE',  ( -3.000000000000000000, -11.95096189432345390, 23.69967320028757385 ) ) ;
#45736 = CARTESIAN_POINT ( 'NONE',  ( 15.00000000000000000, 18.84667830672579569, -18.68964196561269375 ) ) ;
#45738 = VERTEX_POINT ( 'NONE', #32389 ) ;
#45737 = AXIS2_PLACEMENT_3D ( 'NONE', #46164, #5047, #1377 ) ;
#45739 = ORIENTED_EDGE ( 'NONE', *, *, #10038, .F. ) ;
#45740 = DIRECTION ( 'NONE',  ( 1.000000000000000000, 0.000000000000000000, 0.000000000000000000 ) ) ;
#45741 = LINE ( 'NONE', #19766, #4811 ) ;
#45742 = EDGE_LOOP ( 'NONE', ( #40257, #38936, #20910, #25 ) ) ;
#45743 = APPLICATION_CONTEXT ( 'automotive_design' ) ;
#45744 = DIRECTION ( 'NONE',  ( -1.000000000000000000, -0.000000000000000000, -0.000000000000000000 ) ) ;
#45745 = ORIENTED_EDGE ( 'NONE', *, *, #40350, .T. ) ;
#45746 = CARTESIAN_POINT ( 'NONE',  ( 10.00000000000000000, -27.75498641678720446, -31.52238457039628727 ) ) ;
#45747 = PLANE ( 'NONE',  #23975 ) ;
#45748 = CARTESIAN_POINT ( 'NONE',  ( 0.000000000000000000, -20.41045688087876897, 72.35160999960810102 ) ) ;
#45749 = CIRCLE ( 'NONE', #12146, 31.99999999999998934 ) ;
#45750 = CARTESIAN_POINT ( 'NONE',  ( 0.000000000000000000, 0.000000000000000000, 0.000000000000000000 ) ) ;
#45751 = VERTEX_POINT ( 'NONE', #16969 ) ;
#45752 = DIRECTION ( 'NONE',  ( -1.000000000000000000, 0.000000000000000000, 0.000000000000000000 ) ) ;
#45753 = VECTOR ( 'NONE', #26776, 1000.000000000000000 ) ;
#45754 = DIRECTION ( 'NONE',  ( -0.000000000000000000, -0.000000000000000000, 1.000000000000000000 ) ) ;
#45755 = CARTESIAN_POINT ( 'NONE',  ( 0.000000000000000000, -68.27212725128254078, -31.46837873495049465 ) ) ;
#45756 = EDGE_LOOP ( 'NONE', ( #9158, #20139, #32903, #14518 ) ) ;
#45757 = AXIS2_PLACEMENT_3D ( 'NONE', #30942, #23569, #15512 ) ;
#45758 = EDGE_CURVE ( 'NONE', #15795, #8980, #39499, .T. ) ;
#45759 = CARTESIAN_POINT ( 'NONE',  ( 0.000000000000000000, -22.64427369931191336, 30.00120703465197280 ) ) ;
#45760 = CARTESIAN_POINT ( 'NONE',  ( 12.00000000000000000, -22.32062822937469093, 14.36278369418830181 ) ) ;
#45761 = EDGE_CURVE ( 'NONE', #28089, #34957, #29328, .T. ) ;
#45762 = ORIENTED_EDGE ( 'NONE', *, *, #9933, .T. ) ;
#45763 = ORIENTED_EDGE ( 'NONE', *, *, #11593, .T. ) ;
#45764 = VECTOR ( 'NONE', #8146, 1000.000000000000227 ) ;
#45765 = CIRCLE ( 'NONE', #34041, 42.00000000000000000 ) ;
#45766 = UNCERTAINTY_MEASURE_WITH_UNIT (LENGTH_MEASURE( 1.000000000000000082E-05 ), #41851, 'distance_accuracy_value', 'NONE');
#45767 = DIRECTION ( 'NONE',  ( 0.000000000000000000, 0.000000000000000000, 1.000000000000000000 ) ) ;
#45768 = ORIENTED_EDGE ( 'NONE', *, *, #17413, .F. ) ;
#45769 = VECTOR ( 'NONE', #2560, 999.9999999999998863 ) ;
#45770 = CYLINDRICAL_SURFACE ( 'NONE', #47955, 42.00000000000000000 ) ;
#45771 = CARTESIAN_POINT ( 'NONE',  ( 8.700667342345820288, -98.11853780484867116, 5.500000000000000000 ) ) ;
#45772 = VECTOR ( 'NONE', #15284, 1000.000000000000000 ) ;
#45773 = ORIENTED_EDGE ( 'NONE', *, *, #29559, .T. ) ;
#45774 = AXIS2_PLACEMENT_3D ( 'NONE', #43561, #40376, #3381 ) ;
#45775 = EDGE_CURVE ( 'NONE', #33952, #38558, #8214, .T. ) ;
#45776 = EDGE_CURVE ( 'NONE', #6985, #36193, #41844, .T. ) ;
#45777 = VECTOR ( 'NONE', #28717, 1000.000000000000000 ) ;
#45778 = EDGE_CURVE ( 'NONE', #10773, #5492, #20155, .T. ) ;
#45779 = DIRECTION ( 'NONE',  ( 0.000000000000000000, 0.9510565162951543083, 0.3090169943749448977 ) ) ;
#45780 = ORIENTED_EDGE ( 'NONE', *, *, #47848, .T. ) ;
#45781 = ORIENTED_EDGE ( 'NONE', *, *, #46716, .F. ) ;
#45782 = EDGE_LOOP ( 'NONE', ( #45798, #15847, #30269, #18620 ) ) ;
#45783 = ORIENTED_EDGE ( 'NONE', *, *, #20504, .F. ) ;
#45784 = AXIS2_PLACEMENT_3D ( 'NONE', #47438, #35703, #28346 ) ;
#45785 = ORIENTED_EDGE ( 'NONE', *, *, #40843, .T. ) ;
#45786 = EDGE_CURVE ( 'NONE', #27256, #18839, #17433, .T. ) ;
#45787 = VECTOR ( 'NONE', #26725, 1000.000000000000000 ) ;
#45788 = CARTESIAN_POINT ( 'NONE',  ( -7.670864526094549163, -97.73662565058241114, 5.500000000000000000 ) ) ;
#45789 = EDGE_LOOP ( 'NONE', ( #37811, #4497, #1654, #27636 ) ) ;
#45790 = CARTESIAN_POINT ( 'NONE',  ( 0.000000000000000000, 9.615535125378773529, 24.73947219025917121 ) ) ;
#45791 = ORIENTED_EDGE ( 'NONE', *, *, #31637, .F. ) ;
#45792 = CARTESIAN_POINT ( 'NONE',  ( 0.000000000000000000, -44.88180994100419952, 63.18004540533013369 ) ) ;
#45793 = ORIENTED_EDGE ( 'NONE', *, *, #25417, .F. ) ;
#45794 = CARTESIAN_POINT ( 'NONE',  ( 5.000000000000002665, -78.73519480814971416, 22.90783923731600069 ) ) ;
#45795 = CARTESIAN_POINT ( 'NONE',  ( 10.00000000000000000, -22.64427369931191336, 30.00120703465197280 ) ) ;
#45796 = EDGE_LOOP ( 'NONE', ( #12428, #4761, #32078, #27279 ) ) ;
#45797 = DIRECTION ( 'NONE',  ( 0.000000000000000000, 0.000000000000000000, 1.000000000000000000 ) ) ;
#45798 = ORIENTED_EDGE ( 'NONE', *, *, #11147, .F. ) ;
#45799 = DIRECTION ( 'NONE',  ( -1.000000000000000000, 0.000000000000000000, -0.000000000000000000 ) ) ;
#45800 = LINE ( 'NONE', #16183, #4739 ) ;
#45801 = CIRCLE ( 'NONE', #40321, 77.49900000000000944 ) ;
#45802 = ORIENTED_EDGE ( 'NONE', *, *, #14609, .F. ) ;
#45803 = CARTESIAN_POINT ( 'NONE',  ( 0.000000000000000000, -39.04073710021356192, 15.48615015657568073 ) ) ;
#45804 = ORIENTED_EDGE ( 'NONE', *, *, #25743, .T. ) ;
#45805 = VERTEX_POINT ( 'NONE', #16491 ) ;
#45806 = CARTESIAN_POINT ( 'NONE',  ( 10.00000000000000000, -6.903761155838323837, 77.19088730480521576 ) ) ;
#45807 = DIRECTION ( 'NONE',  ( -1.000000000000000000, 0.000000000000000000, 0.000000000000000000 ) ) ;
#45808 = ORIENTED_EDGE ( 'NONE', *, *, #27479, .F. ) ;
#45809 = CARTESIAN_POINT ( 'NONE',  ( 14.59956846177685996, -138.4757300459248484, 5.500000000000000000 ) ) ;
#45810 = CIRCLE ( 'NONE', #20782, 82.00000000000000000 ) ;
#45811 = DIRECTION ( 'NONE',  ( 0.000000000000000000, -0.9135454576426009776, -0.4067366430758000417 ) ) ;
#45812 = LINE ( 'NONE', #12283, #27665 ) ;
#45813 = CIRCLE ( 'NONE', #16112, 77.49899999999999523 ) ;
#45814 = CARTESIAN_POINT ( 'NONE',  ( 10.00000000000000000, 34.44570377933695227, -69.42325613327405165 ) ) ;
#45815 = DIRECTION ( 'NONE',  ( -1.000000000000000000, 0.000000000000000000, -0.000000000000000000 ) ) ;
#45816 = DIRECTION ( 'NONE',  ( -0.000000000000000000, -0.000000000000000000, -1.000000000000000000 ) ) ;
#45817 = DIRECTION ( 'NONE',  ( -0.000000000000000000, -0.000000000000000000, -1.000000000000000000 ) ) ;
#45818 = CARTESIAN_POINT ( 'NONE',  ( 0.000000000000000000, 31.52238457039599595, 27.75498641678753842 ) ) ;
#45819 = CARTESIAN_POINT ( 'NONE',  ( 0.000000000000000000, -35.47612816024506088, -22.48208911017539435 ) ) ;
#45820 = EDGE_CURVE ( 'NONE', #36993, #23918, #7457, .T. ) ;
#45821 = ORIENTED_EDGE ( 'NONE', *, *, #39302, .T. ) ;
#45822 = EDGE_CURVE ( 'NONE', #41107, #28690, #22336, .T. ) ;
#45823 = CIRCLE ( 'NONE', #33334, 31.99999999999999645 ) ;
#45824 = DIRECTION ( 'NONE',  ( 0.000000000000000000, -0.7071067811865536790, 0.7071067811865412445 ) ) ;
#45825 = CARTESIAN_POINT ( 'NONE',  ( 5.000000000000000000, 36.13751322684419165, 21.40280677340384585 ) ) ;
#45826 = DIRECTION ( 'NONE',  ( 0.000000000000000000, 0.000000000000000000, 1.000000000000000000 ) ) ;
#45827 = VECTOR ( 'NONE', #16237, 1000.000000000000000 ) ;
#45828 = DIRECTION ( 'NONE',  ( 0.000000000000000000, 0.000000000000000000, 1.000000000000000000 ) ) ;
#45829 = EDGE_CURVE ( 'NONE', #1236, #12511, #32842, .T. ) ;
#45830 = VERTEX_POINT ( 'NONE', #25253 ) ;
#45831 = ORIENTED_EDGE ( 'NONE', *, *, #1678, .F. ) ;
#45832 = AXIS2_PLACEMENT_3D ( 'NONE', #12234, #41124, #37926 ) ;
#45833 = DIRECTION ( 'NONE',  ( -1.000000000000000000, 0.000000000000000000, -0.000000000000000000 ) ) ;
#45834 = ADVANCED_FACE ( 'NONE', ( #39978 ), #47769, .T. ) ;
#45835 = ORIENTED_EDGE ( 'NONE', *, *, #28276, .F. ) ;
#45836 = ADVANCED_FACE ( 'NONE', ( #44595 ), #29435, .T. ) ;
#45837 = DIRECTION ( 'NONE',  ( 0.000000000000000000, -0.6494480483301739993, -0.7604059656000392575 ) ) ;
#45838 = SHAPE_DEFINITION_REPRESENTATION ( #20629, #31260 ) ;
#45839 = CARTESIAN_POINT ( 'NONE',  ( 0.000000000000000000, -5.202137450156129717, -37.22597642581163768 ) ) ;
#45840 = AXIS2_PLACEMENT_3D ( 'NONE', #11448, #30284, #42021 ) ;
#45841 = ORIENTED_EDGE ( 'NONE', *, *, #39997, .F. ) ;
#45842 = AXIS2_PLACEMENT_3D ( 'NONE', #13397, #10200, #43020 ) ;
#45843 = ORIENTED_EDGE ( 'NONE', *, *, #33243, .F. ) ;
#45844 = CYLINDRICAL_SURFACE ( 'NONE', #19050, 31.99999999999998579 ) ;
#45845 = AXIS2_PLACEMENT_3D ( 'NONE', #38043, #38275, #38780 ) ;
#45846 = ORIENTED_EDGE ( 'NONE', *, *, #3350, .F. ) ;
#45847 = EDGE_CURVE ( 'NONE', #9112, #7054, #38741, .T. ) ;
#45848 = DIRECTION ( 'NONE',  ( -1.000000000000000000, -0.000000000000000000, 0.000000000000000000 ) ) ;
#45849 = ORIENTED_EDGE ( 'NONE', *, *, #7463, .F. ) ;
#45850 = AXIS2_PLACEMENT_3D ( 'NONE', #27892, #42806, #9258 ) ;
#45851 = DIRECTION ( 'NONE',  ( -1.000000000000000000, 0.000000000000000000, 0.000000000000000000 ) ) ;
#45852 = CARTESIAN_POINT ( 'NONE',  ( 10.00000000000000000, 0.000000000000000000, 0.000000000000000000 ) ) ;
#45853 = ORIENTED_EDGE ( 'NONE', *, *, #23798, .T. ) ;
#45854 = AXIS2_PLACEMENT_3D ( 'NONE', #23768, #1004, #27216 ) ;
#45855 = EDGE_CURVE ( 'NONE', #9305, #15480, #44836, .T. ) ;
#45856 = CIRCLE ( 'NONE', #3630, 42.00000000000000000 ) ;
#45857 = DIRECTION ( 'NONE',  ( -1.000000000000000000, -0.000000000000000000, -0.000000000000000000 ) ) ;
#45858 = CARTESIAN_POINT ( 'NONE',  ( 10.00000000000000000, -37.58145647212455032, 0.6853352020789044152 ) ) ;
#45859 = CARTESIAN_POINT ( 'NONE',  ( 26.28306158492127764, -123.3838844133976522, 2.500000000000000000 ) ) ;
#45860 = CARTESIAN_POINT ( 'NONE',  ( 19.29194287201271862, -133.5026271600380880, 5.500000000000000000 ) ) ;
#45861 = ORIENTED_EDGE ( 'NONE', *, *, #33262, .F. ) ;
#45862 = DIRECTION ( 'NONE',  ( -1.000000000000000000, -0.000000000000000000, -0.000000000000000000 ) ) ;
#45863 = ORIENTED_EDGE ( 'NONE', *, *, #28580, .F. ) ;
#45864 = ORIENTED_EDGE ( 'NONE', *, *, #7480, .T. ) ;
#45865 = CARTESIAN_POINT ( 'NONE',  ( 11.99999999999999822, 0.000000000000000000, 0.000000000000000000 ) ) ;
#45866 = ORIENTED_EDGE ( 'NONE', *, *, #21379, .T. ) ;
#45867 = CARTESIAN_POINT ( 'NONE',  ( 10.00000000000000000, -16.23288003029473359, -33.80338159004301701 ) ) ;
#45868 = DIRECTION ( 'NONE',  ( -0.000000000000000000, -0.000000000000000000, -1.000000000000000000 ) ) ;
#45869 = FACE_OUTER_BOUND ( 'NONE', #39402, .T. ) ;
#45870 = VERTEX_POINT ( 'NONE', #6914 ) ;
#45871 = LINE ( 'NONE', #12814, #8880 ) ;
#45872 = CARTESIAN_POINT ( 'NONE',  ( 15.00000000000000000, 23.59884966291538078, 12.14883922797231008 ) ) ;
#45873 = DIRECTION ( 'NONE',  ( -1.000000000000000000, -0.000000000000000000, -0.000000000000000000 ) ) ;
#45874 = DIRECTION ( 'NONE',  ( 0.000000000000000000, -0.6494480483301739993, -0.7604059656000390355 ) ) ;
#45875 = ADVANCED_FACE ( 'NONE', ( #14509 ), #6682, .T. ) ;
#45876 = CARTESIAN_POINT ( 'NONE',  ( -21.67772167707813935, -110.8034581014852762, 5.500000000000000000 ) ) ;
#45877 = AXIS2_PLACEMENT_3D ( 'NONE', #35118, #9909, #1847 ) ;
#45878 = DIRECTION ( 'NONE',  ( -1.000000000000000000, -0.000000000000000000, -0.000000000000000000 ) ) ;
#45879 = CARTESIAN_POINT ( 'NONE',  ( -4.250000000000000000, -13.95926121303099343, -1.199999999999999956 ) ) ;
#45880 = LINE ( 'NONE', #31439, #3662 ) ;
#45881 = EDGE_CURVE ( 'NONE', #44202, #41727, #31765, .T. ) ;
#45882 = AXIS2_PLACEMENT_3D ( 'NONE', #13724, #6376, #2443 ) ;
#45883 = CARTESIAN_POINT ( 'NONE',  ( 10.00000000000000000, -73.95703589263958122, -23.16143007188506431 ) ) ;
#45884 = DIRECTION ( 'NONE',  ( -1.000000000000000000, 0.000000000000000000, 0.000000000000000000 ) ) ;
#45885 = EDGE_CURVE ( 'NONE', #36640, #25973, #17915, .T. ) ;
#45886 = ORIENTED_EDGE ( 'NONE', *, *, #42232, .F. ) ;
#45887 = VERTEX_POINT ( 'NONE', #36758 ) ;
#45888 = LINE ( 'NONE', #24971, #599 ) ;
#45889 = FACE_OUTER_BOUND ( 'NONE', #3555, .T. ) ;
#45890 = AXIS2_PLACEMENT_3D ( 'NONE', #15047, #34587, #45375 ) ;
#45891 = VERTEX_POINT ( 'NONE', #29176 ) ;
#45892 = ORIENTED_EDGE ( 'NONE', *, *, #26537, .T. ) ;
#45893 = ADVANCED_FACE ( 'NONE', ( #3721 ), #29662, .T. ) ;
#45894 = CARTESIAN_POINT ( 'NONE',  ( 10.00000000000000000, -30.00120703465189465, -22.64427369931201639 ) ) ;
#45895 = DIRECTION ( 'NONE',  ( 1.000000000000000000, 0.000000000000000000, 0.000000000000000000 ) ) ;
#45896 = ORIENTED_EDGE ( 'NONE', *, *, #28580, .T. ) ;
#45897 = VECTOR ( 'NONE', #3289, 1000.000000000000000 ) ;
#45898 = ORIENTED_EDGE ( 'NONE', *, *, #38925, .T. ) ;
#45899 = ORIENTED_EDGE ( 'NONE', *, *, #34019, .F. ) ;
#45900 = VERTEX_POINT ( 'NONE', #25741 ) ;
#45901 = LINE ( 'NONE', #22642, #14447 ) ;
#45902 = CARTESIAN_POINT ( 'NONE',  ( -10.00000000000000000, 0.000000000000000000, 0.000000000000000000 ) ) ;
#45903 = DIRECTION ( 'NONE',  ( -1.000000000000000000, 0.000000000000000000, -0.000000000000000000 ) ) ;
#45904 = VERTEX_POINT ( 'NONE', #36292 ) ;
#45905 = AXIS2_PLACEMENT_3D ( 'NONE', #8769, #37672, #5123 ) ;
#45906 = FACE_OUTER_BOUND ( 'NONE', #46998, .T. ) ;
#45907 = VERTEX_POINT ( 'NONE', #11325 ) ;
#45908 = VERTEX_POINT ( 'NONE', #10335 ) ;
#45909 = ORIENTED_EDGE ( 'NONE', *, *, #9116, .T. ) ;
#45910 = FACE_OUTER_BOUND ( 'NONE', #23279, .T. ) ;
#45911 = DIRECTION ( 'NONE',  ( 0.000000000000000000, 0.9876883405951383255, -0.1564344650402276216 ) ) ;
#45912 = LINE ( 'NONE', #12862, #43896 ) ;
#45913 = VERTEX_POINT ( 'NONE', #33576 ) ;
#45914 = AXIS2_PLACEMENT_3D ( 'NONE', #15239, #33345, #19132 ) ;
#45915 = ORIENTED_EDGE ( 'NONE', *, *, #39126, .T. ) ;
#45916 = CARTESIAN_POINT ( 'NONE',  ( 0.000000000000000000, -60.67117009219176538, 55.16347631943019536 ) ) ;
#45917 = ORIENTED_EDGE ( 'NONE', *, *, #17674, .T. ) ;
#45918 = CYLINDRICAL_SURFACE ( 'NONE', #27009, 16.00000000000000000 ) ;
#45919 = EDGE_CURVE ( 'NONE', #6623, #6273, #37177, .T. ) ;
#45920 = DIRECTION ( 'NONE',  ( 0.3853207896976533209, -0.9227826878668545785, 0.000000000000000000 ) ) ;
#45921 = CARTESIAN_POINT ( 'NONE',  ( -22.53294031248082163, -134.0273518838794757, 5.500000000000000000 ) ) ;
#45922 = DIRECTION ( 'NONE',  ( 0.000000000000000000, 0.1564344650402244852, 0.9876883405951387696 ) ) ;
#45923 = LINE ( 'NONE', #12390, #45356 ) ;
#45924 = FACE_OUTER_BOUND ( 'NONE', #35110, .T. ) ;
#45925 = CARTESIAN_POINT ( 'NONE',  ( 0.000000000000000000, 0.000000000000000000, 0.000000000000000000 ) ) ;
#45926 =( NAMED_UNIT ( * ) SI_UNIT ( $, .STERADIAN. ) SOLID_ANGLE_UNIT ( ) );
#45927 = FACE_OUTER_BOUND ( 'NONE', #34308, .T. ) ;
#45928 = CIRCLE ( 'NONE', #2178, 37.49900000000001654 ) ;
#45929 = CARTESIAN_POINT ( 'NONE',  ( 21.85433023846371370, -135.0628101570779620, -2.500000000000000444 ) ) ;
#45930 = LINE ( 'NONE', #42244, #2001 ) ;
#45931 = VERTEX_POINT ( 'NONE', #2754 ) ;
#45932 = ORIENTED_EDGE ( 'NONE', *, *, #16473, .T. ) ;
#45933 = DIRECTION ( 'NONE',  ( 0.000000000000000000, 0.1564344650402312298, -0.9876883405951375483 ) ) ;
#45934 = CARTESIAN_POINT ( 'NONE',  ( 22.08297821871651934, -111.8242998470044540, 5.500000000000000000 ) ) ;
#45935 = LINE ( 'NONE', #23401, #25115 ) ;
#45936 = DIRECTION ( 'NONE',  ( 0.2306669878475623159, 0.9730327541852497042, -0.000000000000000000 ) ) ;
#45937 = EDGE_CURVE ( 'NONE', #8725, #23235, #19215, .T. ) ;
#45938 = EDGE_CURVE ( 'NONE', #25055, #25836, #8259, .T. ) ;
#45939 = EDGE_CURVE ( 'NONE', #43802, #4790, #25508, .T. ) ;
#45940 = CARTESIAN_POINT ( 'NONE',  ( 11.99999999999999822, -67.80270845531855173, -46.11716303203260736 ) ) ;
#45941 = ADVANCED_FACE ( 'NONE', ( #18413 ), #10831, .T. ) ;
#45942 = VECTOR ( 'NONE', #23817, 1000.000000000000000 ) ;
#45943 = DIRECTION ( 'NONE',  ( -1.000000000000000000, 0.000000000000000000, 0.000000000000000000 ) ) ;
#45944 = CARTESIAN_POINT ( 'NONE',  ( 8.700667342345820288, -98.11853780484867116, 5.500000000000000000 ) ) ;
#45945 = VERTEX_POINT ( 'NONE', #37495 ) ;
#45946 = EDGE_CURVE ( 'NONE', #9070, #27388, #16199, .T. ) ;
#45947 = AXIS2_PLACEMENT_3D ( 'NONE', #40809, #48388, #7269 ) ;
#45948 = EDGE_CURVE ( 'NONE', #37098, #9486, #37999, .T. ) ;
#45949 = ORIENTED_EDGE ( 'NONE', *, *, #43655, .F. ) ;
#45950 = CARTESIAN_POINT ( 'NONE',  ( 0.000000000000000000, 0.000000000000000000, 77.49899999999999523 ) ) ;
#45951 = EDGE_LOOP ( 'NONE', ( #8077, #40264, #41785, #47179 ) ) ;
#45952 = VERTEX_POINT ( 'NONE', #15470 ) ;
#45953 = VECTOR ( 'NONE', #37869, 1000.000000000000000 ) ;
#45954 = ORIENTED_EDGE ( 'NONE', *, *, #1215, .F. ) ;
#45955 = DIRECTION ( 'NONE',  ( 0.000000000000000000, 0.4067366430757889950, -0.9135454576426058626 ) ) ;
#45956 = ORIENTED_EDGE ( 'NONE', *, *, #22803, .T. ) ;
#45957 = ADVANCED_FACE ( 'NONE', ( #27213 ), #23292, .T. ) ;
#45958 = CIRCLE ( 'NONE', #24846, 16.00000000000000000 ) ;
#45959 = CARTESIAN_POINT ( 'NONE',  ( 26.09152095774781799, -124.8716048804687375, -2.500000000000000444 ) ) ;
#45960 = DIRECTION ( 'NONE',  ( 0.000000000000000000, 0.000000000000000000, 1.000000000000000000 ) ) ;
#45961 = ORIENTED_EDGE ( 'NONE', *, *, #14978, .T. ) ;
#45962 = EDGE_CURVE ( 'NONE', #17038, #12299, #18874, .T. ) ;
#45963 = CARTESIAN_POINT ( 'NONE',  ( 0.000000000000000000, -18.89407956138203204, -75.16055320797050854 ) ) ;
#45965 = VERTEX_POINT ( 'NONE', #280 ) ;
#45964 = CARTESIAN_POINT ( 'NONE',  ( 10.00000000000000000, 32.34446384429971744, 26.79245525562727082 ) ) ;
#45966 = VECTOR ( 'NONE', #1487, 999.9999999999998863 ) ;
#45967 = CARTESIAN_POINT ( 'NONE',  ( 0.000000000000000000, 26.79245525562714292, 32.34446384429980981 ) ) ;
#45968 = ADVANCED_FACE ( 'NONE', ( #34781 ), #23914, .T. ) ;
#45969 = ORIENTED_EDGE ( 'NONE', *, *, #20953, .F. ) ;
#45970 = CARTESIAN_POINT ( 'NONE',  ( 10.00000000000000000, -2.956366410621191765, 75.11725578898467859 ) ) ;
#45971 = VERTEX_POINT ( 'NONE', #23520 ) ;
#45972 = ORIENTED_EDGE ( 'NONE', *, *, #40092, .T. ) ;
#45973 = SHAPE_REPRESENTATION ( 'key', ( #11636 ), #48316 ) ;
#45974 = DIRECTION ( 'NONE',  ( -0.7273375899149793211, 0.6862798483830554463, 0.000000000000000000 ) ) ;
#45975 = LINE ( 'NONE', #20254, #14737 ) ;
#45976 = EDGE_CURVE ( 'NONE', #30136, #1874, #19590, .T. ) ;
#45977 = ORIENTED_EDGE ( 'NONE', *, *, #32822, .T. ) ;
#45978 = FACE_OUTER_BOUND ( 'NONE', #13252, .T. ) ;
#45979 = CARTESIAN_POINT ( 'NONE',  ( 6.000000000000000000, -22.90783923731685334, 78.73519480814945837 ) ) ;
#45980 = DIRECTION ( 'NONE',  ( -1.000000000000000000, -0.000000000000000000, 0.000000000000000000 ) ) ;
#45981 = VECTOR ( 'NONE', #6292, 1000.000000000000000 ) ;
#45982 = ADVANCED_FACE ( 'NONE', ( #761 ), #23049, .T. ) ;
#45983 = VERTEX_POINT ( 'NONE', #11794 ) ;
#45984 = ORIENTED_EDGE ( 'NONE', *, *, #32110, .T. ) ;
#45985 = FACE_OUTER_BOUND ( 'NONE', #11545, .T. ) ;
#45986 = CARTESIAN_POINT ( 'NONE',  ( -23.97194136764370853, -131.3950000906648938, 2.500000000000000000 ) ) ;
#45987 = ORIENTED_EDGE ( 'NONE', *, *, #26310, .F. ) ;
#45988 = DIRECTION ( 'NONE',  ( -0.000000000000000000, -0.000000000000000000, -1.000000000000000000 ) ) ;
#45989 = VERTEX_POINT ( 'NONE', #19841 ) ;
#45990 = CARTESIAN_POINT ( 'NONE',  ( 11.99999999999999822, 0.000000000000000000, 0.000000000000000000 ) ) ;
#45991 = CARTESIAN_POINT ( 'NONE',  ( 0.000000000000000000, -54.21277698773713638, 55.38113227695764351 ) ) ;
#45992 = DIRECTION ( 'NONE',  ( 0.000000000000000000, 0.000000000000000000, 1.000000000000000000 ) ) ;
#45993 = ORIENTED_EDGE ( 'NONE', *, *, #16976, .F. ) ;
#45994 = AXIS2_PLACEMENT_3D ( 'NONE', #36775, #18892, #14274 ) ;
#45995 = CARTESIAN_POINT ( 'NONE',  ( 11.99999999999999822, 54.21277698773675979, 55.38113227695801299 ) ) ;
#45996 = EDGE_CURVE ( 'NONE', #37697, #10193, #7488, .T. ) ;
#45997 = EDGE_CURVE ( 'NONE', #33539, #15162, #13746, .T. ) ;
#45998 = DIRECTION ( 'NONE',  ( 0.000000000000000000, -0.5877852522924801315, 0.8090169943749423442 ) ) ;
#45999 = CIRCLE ( 'NONE', #24873, 82.00000000000000000 ) ;
#46000 = DIRECTION ( 'NONE',  ( 1.000000000000000000, -0.000000000000000000, 0.000000000000000000 ) ) ;
#46001 = CYLINDRICAL_SURFACE ( 'NONE', #9126, 37.49900000000000233 ) ;
#46002 = CYLINDRICAL_SURFACE ( 'NONE', #17638, 42.00000000000000000 ) ;
#46003 = EDGE_LOOP ( 'NONE', ( #26704, #38700, #9656, #45100 ) ) ;
#46004 = CYLINDRICAL_SURFACE ( 'NONE', #21375, 16.00000000000000000 ) ;
#46005 =( LENGTH_UNIT ( ) NAMED_UNIT ( * ) SI_UNIT ( .MILLI., .METRE. ) );
#46006 = VERTEX_POINT ( 'NONE', #45315 ) ;
#46007 = EDGE_CURVE ( 'NONE', #12589, #37461, #26485, .T. ) ;
#46008 = ORIENTED_EDGE ( 'NONE', *, *, #2875, .T. ) ;
#46009 = FACE_OUTER_BOUND ( 'NONE', #42280, .T. ) ;
#46010 = VERTEX_POINT ( 'NONE', #15237 ) ;
#46011 = VECTOR ( 'NONE', #46787, 1000.000000000000000 ) ;
#46012 = CARTESIAN_POINT ( 'NONE',  ( 10.00000000000000000, 30.84782396557248418, -21.32104025579081252 ) ) ;
#46013 = DIRECTION ( 'NONE',  ( -1.000000000000000000, -0.000000000000000000, 0.000000000000000000 ) ) ;
#46014 = ORIENTED_EDGE ( 'NONE', *, *, #48016, .T. ) ;
#46015 = DIRECTION ( 'NONE',  ( -1.000000000000000000, 0.000000000000000000, -0.000000000000000000 ) ) ;
#46016 = ORIENTED_EDGE ( 'NONE', *, *, #14825, .F. ) ;
#46017 = ORIENTED_EDGE ( 'NONE', *, *, #41853, .T. ) ;
#46018 = ORIENTED_EDGE ( 'NONE', *, *, #19191, .T. ) ;
#46019 = ORIENTED_EDGE ( 'NONE', *, *, #27267, .T. ) ;
#46020 = ORIENTED_EDGE ( 'NONE', *, *, #47467, .F. ) ;
#46021 = DIRECTION ( 'NONE',  ( -1.000000000000000000, -0.000000000000000000, -0.000000000000000000 ) ) ;
#46022 = ADVANCED_FACE ( 'NONE', ( #12290 ), #42136, .F. ) ;
#46023 = ORIENTED_EDGE ( 'NONE', *, *, #14978, .F. ) ;
#46024 = VERTEX_POINT ( 'NONE', #41414 ) ;
#46025 = CARTESIAN_POINT ( 'NONE',  ( 11.99999999999999822, 12.93880638057426502, -76.41127070299258150 ) ) ;
#46026 = ORIENTED_EDGE ( 'NONE', *, *, #35261, .F. ) ;
#46027 =( REPRESENTATION_RELATIONSHIP ('NONE','NONE', #5957, #22809 ) REPRESENTATION_RELATIONSHIP_WITH_TRANSFORMATION ( #39205 )SHAPE_REPRESENTATION_RELATIONSHIP( ) );
#46028 = FACE_OUTER_BOUND ( 'NONE', #27846, .T. ) ;
#46029 = ADVANCED_FACE ( 'NONE', ( #7869 ), #22805, .F. ) ;
#46030 = CARTESIAN_POINT ( 'NONE',  ( 0.000000000000000000, 8.688484142253939169, 21.88630264137371029 ) ) ;
#46031 = DIRECTION ( 'NONE',  ( 0.000000000000000000, 0.000000000000000000, 1.000000000000000000 ) ) ;
#46032 = EDGE_CURVE ( 'NONE', #16667, #9910, #30951, .T. ) ;
#46033 = ORIENTED_EDGE ( 'NONE', *, *, #44906, .T. ) ;
#46034 = CARTESIAN_POINT ( 'NONE',  ( 0.000000000000000000, 0.000000000000000000, 0.000000000000000000 ) ) ;
#46035 = ORIENTED_EDGE ( 'NONE', *, *, #2013, .F. ) ;
#46036 = CARTESIAN_POINT ( 'NONE',  ( 14.59956846177685996, -138.4757300459248484, 5.500000000000000000 ) ) ;
#46037 = LINE ( 'NONE', #6125, #18799 ) ;
#46038 = ORIENTED_EDGE ( 'NONE', *, *, #33746, .T. ) ;
#46039 = DIRECTION ( 'NONE',  ( 0.000000000000000000, 0.9723699203976756689, 0.2334453638559093602 ) ) ;
#46040 = ORIENTED_EDGE ( 'NONE', *, *, #39654, .F. ) ;
#46041 = ORIENTED_EDGE ( 'NONE', *, *, #6875, .F. ) ;
#46042 = CARTESIAN_POINT ( 'NONE',  ( 0.000000000000000000, 27.05870788708231700, 26.08949754953034272 ) ) ;
#46043 = DIRECTION ( 'NONE',  ( 0.000000000000000000, 0.000000000000000000, 1.000000000000000000 ) ) ;
#46044 = ORIENTED_EDGE ( 'NONE', *, *, #39969, .T. ) ;
#46045 = VECTOR ( 'NONE', #44011, 1000.000000000000000 ) ;
#46046 = CARTESIAN_POINT ( 'NONE',  ( -3.000000000000002665, 0.000000000000000000, 20.64000000000000057 ) ) ;
#46047 = CARTESIAN_POINT ( 'NONE',  ( 10.00000000000000000, 0.000000000000000000, 0.000000000000000000 ) ) ;
#46048 = CARTESIAN_POINT ( 'NONE',  ( 0.000000000000000000, -44.99326035066007279, -68.55367621811190304 ) ) ;
#46049 = ORIENTED_EDGE ( 'NONE', *, *, #33419, .T. ) ;
#46050 = AXIS2_PLACEMENT_3D ( 'NONE', #38369, #26151, #26876 ) ;
#46051 = DIRECTION ( 'NONE',  ( 0.000000000000000000, 0.000000000000000000, -1.000000000000000000 ) ) ;
#46052 = EDGE_CURVE ( 'NONE', #24556, #35257, #8112, .T. ) ;
#46053 = DIRECTION ( 'NONE',  ( -1.000000000000000000, -0.000000000000000000, 0.000000000000000000 ) ) ;
#46054 = EDGE_CURVE ( 'NONE', #11693, #42163, #34291, .T. ) ;
#46055 = DIRECTION ( 'NONE',  ( 0.000000000000000000, 0.000000000000000000, 1.000000000000000000 ) ) ;
#46056 = DIRECTION ( 'NONE',  ( -1.000000000000000000, 0.000000000000000000, 0.000000000000000000 ) ) ;
#46057 = ADVANCED_FACE ( 'NONE', ( #24492 ), #31865, .T. ) ;
#46058 = CARTESIAN_POINT ( 'NONE',  ( 23.11608002360578240, -124.4885236261218182, 5.500000000000000000 ) ) ;
#46059 = DIRECTION ( 'NONE',  ( -1.000000000000000000, -0.000000000000000000, 0.000000000000000000 ) ) ;
#46060 = CARTESIAN_POINT ( 'NONE',  ( 0.000000000000000000, -120.0000000000000000, 2.500000000000000000 ) ) ;
#46061 = DIRECTION ( 'NONE',  ( 1.000000000000000000, 0.000000000000000000, 0.000000000000000000 ) ) ;
#46062 = DIRECTION ( 'NONE',  ( 1.000000000000000000, -0.000000000000000000, -0.000000000000000000 ) ) ;
#46063 = LINE ( 'NONE', #769, #21756 ) ;
#46064 = EDGE_LOOP ( 'NONE', ( #44564, #39507, #45461, #40765 ) ) ;
#46065 = EDGE_CURVE ( 'NONE', #7777, #29618, #11413, .T. ) ;
#46066 = CARTESIAN_POINT ( 'NONE',  ( 0.000000000000000000, -75.16055320797043748, 18.89407956138229494 ) ) ;
#46067 = EDGE_LOOP ( 'NONE', ( #8374, #47687, #19732, #22426 ) ) ;
#46068 = CARTESIAN_POINT ( 'NONE',  ( 0.000000000000000000, -50.23322058963299241, -64.81221759200397514 ) ) ;
#46069 = APPLICATION_PROTOCOL_DEFINITION ( 'draft international standard', 'automotive_design', 1998, #5717 ) ;
#46070 = CARTESIAN_POINT ( 'NONE',  ( 11.99999999999999822, 75.11764819372149304, -2.946379043146603482 ) ) ;
#46071 = EDGE_LOOP ( 'NONE', ( #33553, #40529, #26583, #45713 ) ) ;
#46072 = AXIS2_PLACEMENT_3D ( 'NONE', #26481, #8583, #3963 ) ;
#46073 = AXIS2_PLACEMENT_3D ( 'NONE', #16106, #31774, #46688 ) ;
#46074 = DIRECTION ( 'NONE',  ( 0.000000000000000000, -0.7604059656000369261, 0.6494480483301766638 ) ) ;
#46075 = AXIS2_PLACEMENT_3D ( 'NONE', #31271, #42521, #46911 ) ;
#46076 = ORIENTED_EDGE ( 'NONE', *, *, #43769, .F. ) ;
#46077 = DIRECTION ( 'NONE',  ( -0.000000000000000000, -0.000000000000000000, -1.000000000000000000 ) ) ;
#46078 = CIRCLE ( 'NONE', #24964, 31.99999999999998579 ) ;
#46079 = CARTESIAN_POINT ( 'NONE',  ( 0.000000000000000000, 16.61724383029390140, -20.69703378468903665 ) ) ;
#46080 = ORIENTED_EDGE ( 'NONE', *, *, #6587, .T. ) ;
#46082 = VERTEX_POINT ( 'NONE', #5656 ) ;
#46081 = DIRECTION ( 'NONE',  ( -1.000000000000000000, -0.000000000000000000, -0.000000000000000000 ) ) ;
#46083 = ORIENTED_EDGE ( 'NONE', *, *, #40581, .F. ) ;
#46084 = EDGE_CURVE ( 'NONE', #46329, #32083, #34069, .T. ) ;
#46085 = EDGE_CURVE ( 'NONE', #41024, #1214, #35022, .T. ) ;
#46086 = FACE_OUTER_BOUND ( 'NONE', #40667, .T. ) ;
#46087 = EDGE_CURVE ( 'NONE', #45129, #37535, #32090, .T. ) ;
#46088 = EDGE_LOOP ( 'NONE', ( #19076, #24849, #11883, #43120 ) ) ;
#46089 = CARTESIAN_POINT ( 'NONE',  ( -3.759344165985237129, 0.000000000000000000, 0.000000000000000000 ) ) ;
#46090 = DIRECTION ( 'NONE',  ( 0.000000000000000000, 0.000000000000000000, 1.000000000000000000 ) ) ;
#46091 = FACE_OUTER_BOUND ( 'NONE', #17357, .T. ) ;
#46092 = EDGE_CURVE ( 'NONE', #30519, #8511, #6718, .T. ) ;
#46093 = LINE ( 'NONE', #12560, #10927 ) ;
#46094 = ORIENTED_EDGE ( 'NONE', *, *, #36424, .T. ) ;
#46095 = CARTESIAN_POINT ( 'NONE',  ( 0.000000000000000000, -16.45098606841149902, 33.79645857604508308 ) ) ;
#46096 = ORIENTED_EDGE ( 'NONE', *, *, #37164, .T. ) ;
#46097 = ADVANCED_FACE ( 'NONE', ( #35510 ), #24247, .T. ) ;
#46098 = PLANE ( 'NONE',  #20000 ) ;
#46099 = CARTESIAN_POINT ( 'NONE',  ( 10.00000000000000000, 16.45098606841126454, 33.79645857604518966 ) ) ;
#46100 = DIRECTION ( 'NONE',  ( 0.000000000000000000, 0.000000000000000000, 1.000000000000000000 ) ) ;
#46101 = DIRECTION ( 'NONE',  ( 1.000000000000000000, 0.000000000000000000, 0.000000000000000000 ) ) ;
#46102 = EDGE_LOOP ( 'NONE', ( #46049, #7725, #12998, #22200 ) ) ;
#46103 = DIRECTION ( 'NONE',  ( -1.000000000000000000, -0.000000000000000000, -0.000000000000000000 ) ) ;
#46104 = DIRECTION ( 'NONE',  ( 0.000000000000000000, -0.4539904997395541875, 0.8910065241883642351 ) ) ;
#46105 = DIRECTION ( 'NONE',  ( 0.000000000000000000, 0.000000000000000000, 1.000000000000000000 ) ) ;
#46106 = EDGE_CURVE ( 'NONE', #22551, #7678, #28602, .T. ) ;
#46107 = FACE_OUTER_BOUND ( 'NONE', #41870, .T. ) ;
#46109 = VECTOR ( 'NONE', #4150, 1000.000000000000114 ) ;
#46108 = CARTESIAN_POINT ( 'NONE',  ( 11.99999999999999822, -75.11764819372145041, 29.05362095685286050 ) ) ;
#46110 = VERTEX_POINT ( 'NONE', #46289 ) ;
#46111 = DIRECTION ( 'NONE',  ( -0.000000000000000000, 0.8090169943749426773, -0.5877852522924796874 ) ) ;
#46112 = EDGE_CURVE ( 'NONE', #15338, #25280, #9056, .T. ) ;
#46113 = CARTESIAN_POINT ( 'NONE',  ( 10.00000000000000000, 31.46837873495072913, -68.27212725128242710 ) ) ;
#46114 = FACE_OUTER_BOUND ( 'NONE', #19149, .T. ) ;
#46115 = VECTOR ( 'NONE', #13032, 1000.000000000000114 ) ;
#46116 = CARTESIAN_POINT ( 'NONE',  ( 6.000000000000000000, -81.96053171279903893, 2.543863470248107994 ) ) ;
#46117 = CARTESIAN_POINT ( 'NONE',  ( -3.961125083139900749, -143.2122702051246677, -2.500000000000000000 ) ) ;
#46118 = CIRCLE ( 'NONE', #17966, 31.99999999999998579 ) ;
#46119 = ORIENTED_EDGE ( 'NONE', *, *, #44736, .F. ) ;
#46120 = EDGE_CURVE ( 'NONE', #23364, #41584, #12980, .T. ) ;
#46121 = DIRECTION ( 'NONE',  ( 0.000000000000000000, 0.000000000000000000, 1.000000000000000000 ) ) ;
#46122 = ORIENTED_EDGE ( 'NONE', *, *, #5478, .F. ) ;
#46123 = EDGE_LOOP ( 'NONE', ( #31938, #1127, #45703, #40423 ) ) ;
#46124 = CARTESIAN_POINT ( 'NONE',  ( 10.00000000000000000, 22.64427369931169309, 30.00120703465213623 ) ) ;
#46125 = CARTESIAN_POINT ( 'NONE',  ( 5.000000000000000000, 55.16347631943042984, 60.67117009219156643 ) ) ;
#46126 = VERTEX_POINT ( 'NONE', #20570 ) ;
#46127 = ADVANCED_FACE ( 'NONE', ( #20825 ), #1743, .T. ) ;
#46128 = ORIENTED_EDGE ( 'NONE', *, *, #28888, .F. ) ;
#46129 = ORIENTED_EDGE ( 'NONE', *, *, #26800, .T. ) ;
#46130 = ORIENTED_EDGE ( 'NONE', *, *, #11929, .F. ) ;
#46131 = ORIENTED_EDGE ( 'NONE', *, *, #37032, .T. ) ;
#46132 = VECTOR ( 'NONE', #42953, 1000.000000000000000 ) ;
#46133 = DIRECTION ( 'NONE',  ( -1.000000000000000000, 0.000000000000000000, 0.000000000000000000 ) ) ;
#46134 = AXIS2_PLACEMENT_3D ( 'NONE', #9397, #46626, #1095 ) ;
#46135 = EDGE_CURVE ( 'NONE', #11806, #14848, #43347, .T. ) ;
#46136 = DIRECTION ( 'NONE',  ( 1.000000000000000000, 0.000000000000000000, -0.000000000000000000 ) ) ;
#46137 = CYLINDRICAL_SURFACE ( 'NONE', #13652, 77.49899999999999523 ) ;
#46138 = AXIS2_PLACEMENT_3D ( 'NONE', #21309, #44321, #36247 ) ;
#46139 = VERTEX_POINT ( 'NONE', #20323 ) ;
#46140 = ADVANCED_FACE ( 'NONE', ( #39185 ), #40346, .F. ) ;
#46141 = DIRECTION ( 'NONE',  ( -1.000000000000000000, 0.000000000000000000, 0.000000000000000000 ) ) ;
#46142 = ORIENTED_EDGE ( 'NONE', *, *, #45336, .F. ) ;
#46143 = ORIENTED_EDGE ( 'NONE', *, *, #2298, .F. ) ;
#46144 = ADVANCED_FACE ( 'NONE', ( #42375 ), #8829, .T. ) ;
#46145 = COLOUR_RGB ( '', 0.66274510, 0.83137255, 0.94901961) ;
#46146 = CARTESIAN_POINT ( 'NONE',  ( 0.000000000000000000, 0.000000000000000000, 0.000000000000000000 ) ) ;
#46147 = CARTESIAN_POINT ( 'NONE',  ( -10.00000000000000000, 0.000000000000000000, 0.000000000000000000 ) ) ;
#46148 = VECTOR ( 'NONE', #13840, 1000.000000000000000 ) ;
#46149 = DIRECTION ( 'NONE',  ( 0.000000000000000000, 0.000000000000000000, -1.000000000000000000 ) ) ;
#46150 = VERTEX_POINT ( 'NONE', #39684 ) ;
#46151 = ORIENTED_EDGE ( 'NONE', *, *, #38248, .T. ) ;
#46152 = VECTOR ( 'NONE', #29355, 1000.000000000000000 ) ;
#46153 = CARTESIAN_POINT ( 'NONE',  ( -11.69999999999999929, 0.000000000000000000, 0.000000000000000000 ) ) ;
#46154 = ORIENTED_EDGE ( 'NONE', *, *, #27877, .T. ) ;
#46155 = ADVANCED_FACE ( 'NONE', ( #2218 ), #46539, .F. ) ;
#46156 = FACE_OUTER_BOUND ( 'NONE', #39075, .T. ) ;
#46157 = LINE ( 'NONE', #8943, #11611 ) ;
#46158 = LINE ( 'NONE', #16534, #22858 ) ;
#46159 = LINE ( 'NONE', #23880, #2647 ) ;
#46160 = CARTESIAN_POINT ( 'NONE',  ( 10.00000000000000000, 0.000000000000000000, 0.000000000000000000 ) ) ;
#46161 = FACE_OUTER_BOUND ( 'NONE', #2546, .T. ) ;
#46162 = CARTESIAN_POINT ( 'NONE',  ( 10.00000000000000000, 0.000000000000000000, 0.000000000000000000 ) ) ;
#46163 = ORIENTED_EDGE ( 'NONE', *, *, #33575, .F. ) ;
#46164 = CARTESIAN_POINT ( 'NONE',  ( 10.00000000000000000, 16.45098606841173705, -33.79645857604496229 ) ) ;
#46165 = DIRECTION ( 'NONE',  ( 0.000000000000000000, 0.000000000000000000, -1.000000000000000000 ) ) ;
#46166 = CARTESIAN_POINT ( 'NONE',  ( -19.90058851926621131, -132.5883508287165853, 5.500000000000000000 ) ) ;
#46167 = ORIENTED_EDGE ( 'NONE', *, *, #43863, .F. ) ;
#46168 = DIRECTION ( 'NONE',  ( -1.000000000000000000, 0.000000000000000000, -0.000000000000000000 ) ) ;
#46169 = FACE_OUTER_BOUND ( 'NONE', #8748, .T. ) ;
#46170 = LINE ( 'NONE', #12641, #21269 ) ;
#46171 = DIRECTION ( 'NONE',  ( 0.000000000000000000, -0.9969173337331270757, -0.07845909572785580988 ) ) ;
#46172 = DIRECTION ( 'NONE',  ( -1.000000000000000000, -0.000000000000000000, -0.000000000000000000 ) ) ;
#46173 = DIRECTION ( 'NONE',  ( 0.000000000000000000, 0.9510565162951521989, 0.3090169943749517256 ) ) ;
#46174 = AXIS2_PLACEMENT_3D ( 'NONE', #16485, #30949, #46341 ) ;
#46175 = DIRECTION ( 'NONE',  ( -1.000000000000000000, -0.000000000000000000, -0.000000000000000000 ) ) ;
#46176 = CARTESIAN_POINT ( 'NONE',  ( 0.000000000000000000, 0.000000000000000000, 0.000000000000000000 ) ) ;
#46177 = VECTOR ( 'NONE', #23550, 1000.000000000000000 ) ;
#46178 = ORIENTED_EDGE ( 'NONE', *, *, #39580, .T. ) ;
#46179 = VECTOR ( 'NONE', #24073, 1000.000000000000000 ) ;
#46180 = AXIS2_PLACEMENT_3D ( 'NONE', #32583, #6401, #21318 ) ;
#46181 = CARTESIAN_POINT ( 'NONE',  ( 11.99999999999999822, 51.02545421589402252, -55.20638768913705263 ) ) ;
#46182 = ORIENTED_EDGE ( 'NONE', *, *, #7656, .T. ) ;
#46183 = ORIENTED_EDGE ( 'NONE', *, *, #26691, .F. ) ;
#46184 = AXIS2_PLACEMENT_3D ( 'NONE', #11317, #30159, #37245 ) ;
#46185 = ORIENTED_EDGE ( 'NONE', *, *, #16699, .T. ) ;
#46186 = DIRECTION ( 'NONE',  ( 0.000000000000000000, 0.5224985647159441360, 0.8526401643540951758 ) ) ;
#46187 = ORIENTED_EDGE ( 'NONE', *, *, #43057, .F. ) ;
#46188 = VERTEX_POINT ( 'NONE', #17141 ) ;
#46189 = EDGE_CURVE ( 'NONE', #25478, #5822, #47010, .T. ) ;
#46190 = FACE_OUTER_BOUND ( 'NONE', #1636, .T. ) ;
#46191 = CARTESIAN_POINT ( 'NONE',  ( 0.000000000000000000, -59.03961581697367933, -46.53671651294010303 ) ) ;
#46192 = ORIENTED_EDGE ( 'NONE', *, *, #30842, .T. ) ;
#46193 = EDGE_LOOP ( 'NONE', ( #3911, #27114, #43299, #3644 ) ) ;
#46194 = ADVANCED_FACE ( 'NONE', ( #40621 ), #33027, .T. ) ;
#46195 = CARTESIAN_POINT ( 'NONE',  ( 11.99999999999999822, 0.000000000000000000, 0.000000000000000000 ) ) ;
#46197 = ORIENTED_EDGE ( 'NONE', *, *, #43061, .T. ) ;
#46196 = CARTESIAN_POINT ( 'NONE',  ( -10.00000000000000000, 0.000000000000000000, 0.000000000000000000 ) ) ;
#46198 = VECTOR ( 'NONE', #7393, 1000.000000000000000 ) ;
#46199 = DIRECTION ( 'NONE',  ( 0.000000000000000000, 0.000000000000000000, 1.000000000000000000 ) ) ;
#46200 = ORIENTED_EDGE ( 'NONE', *, *, #47052, .F. ) ;
#46202 = VERTEX_POINT ( 'NONE', #28875 ) ;
#46201 = AXIS2_PLACEMENT_3D ( 'NONE', #46196, #23676, #39598 ) ;
#46203 = DIRECTION ( 'NONE',  ( -1.000000000000000000, -0.000000000000000000, 0.000000000000000000 ) ) ;
#46204 = ORIENTED_EDGE ( 'NONE', *, *, #45406, .T. ) ;
#46205 = VERTEX_POINT ( 'NONE', #29371 ) ;
#46206 = ADVANCED_FACE ( 'NONE', ( #47957 ), #3405, .F. ) ;
#46207 = CARTESIAN_POINT ( 'NONE',  ( 5.000000000000000000, -22.48208911017474065, -35.47612816024548721 ) ) ;
#46208 = CIRCLE ( 'NONE', #19626, 37.49900000000000233 ) ;
#46209 = CIRCLE ( 'NONE', #39963, 31.99999999999999289 ) ;
#46210 = PLANE ( 'NONE',  #28017 ) ;
#46211 = VERTEX_POINT ( 'NONE', #22010 ) ;
#46212 = EDGE_CURVE ( 'NONE', #44331, #1101, #14444, .T. ) ;
#46213 = DIRECTION ( 'NONE',  ( 0.000000000000000000, 0.000000000000000000, 1.000000000000000000 ) ) ;
#46214 = CARTESIAN_POINT ( 'NONE',  ( 5.000000000000000000, -31.52238457039579345, -27.75498641678775158 ) ) ;
#46215 = DIRECTION ( 'NONE',  ( 0.000000000000000000, 0.000000000000000000, 1.000000000000000000 ) ) ;
#46216 = ORIENTED_EDGE ( 'NONE', *, *, #21667, .T. ) ;
#46217 = AXIS2_PLACEMENT_3D ( 'NONE', #26169, #33499, #14429 ) ;
#46218 = ORIENTED_EDGE ( 'NONE', *, *, #4958, .T. ) ;
#46219 = AXIS2_PLACEMENT_3D ( 'NONE', #20317, #35255, #30628 ) ;
#46220 = CARTESIAN_POINT ( 'NONE',  ( 0.000000000000000000, 0.000000000000000000, 0.000000000000000000 ) ) ;
#46221 = FACE_OUTER_BOUND ( 'NONE', #175, .T. ) ;
#46222 = ORIENTED_EDGE ( 'NONE', *, *, #33705, .F. ) ;
#46223 = AXIS2_PLACEMENT_3D ( 'NONE', #32254, #28585, #43516 ) ;
#46224 = CYLINDRICAL_SURFACE ( 'NONE', #38476, 31.99999999999998579 ) ;
#46225 = EDGE_LOOP ( 'NONE', ( #27441, #27419, #17004, #11825 ) ) ;
#46226 = DIRECTION ( 'NONE',  ( -1.000000000000000000, 0.000000000000000000, -0.000000000000000000 ) ) ;
#46227 = DIRECTION ( 'NONE',  ( -1.000000000000000000, 0.000000000000000000, 0.000000000000000000 ) ) ;
#46228 = DIRECTION ( 'NONE',  ( -1.000000000000000000, 0.000000000000000000, 0.000000000000000000 ) ) ;
#46229 = DIRECTION ( 'NONE',  ( 0.000000000000000000, 0.9723699203976773342, -0.2334453638559024491 ) ) ;
#46230 = CARTESIAN_POINT ( 'NONE',  ( 11.99999999999999822, 0.000000000000000000, 0.000000000000000000 ) ) ;
#46231 = DIRECTION ( 'NONE',  ( 0.000000000000000000, 0.2334453638558990629, 0.9723699203976782224 ) ) ;
#46232 = CARTESIAN_POINT ( 'NONE',  ( 0.000000000000000000, 36.88895765772642221, -6.736453364083161865 ) ) ;
#46233 = CARTESIAN_POINT ( 'NONE',  ( 25.81725066941077529, -113.8380548628854854, 5.500000000000000000 ) ) ;
#46234 = VERTEX_POINT ( 'NONE', #48209 ) ;
#46235 = CARTESIAN_POINT ( 'NONE',  ( -2.977765906491215642, 0.000000000000000000, -15.39727592589476579 ) ) ;
#46236 = ORIENTED_EDGE ( 'NONE', *, *, #33225, .T. ) ;
#46237 = ORIENTED_EDGE ( 'NONE', *, *, #33819, .T. ) ;
#46238 = CIRCLE ( 'NONE', #4830, 77.49900000000000944 ) ;
#46239 = EDGE_CURVE ( 'NONE', #27291, #6602, #6379, .T. ) ;
#46240 = VECTOR ( 'NONE', #30993, 1000.000000000000000 ) ;
#46241 = CARTESIAN_POINT ( 'NONE',  ( 0.000000000000000000, -37.22597642581153821, 10.79786254984320415 ) ) ;
#46242 = ORIENTED_EDGE ( 'NONE', *, *, #20173, .F. ) ;
#46243 = AXIS2_PLACEMENT_3D ( 'NONE', #30498, #4328, #26589 ) ;
#46244 = AXIS2_PLACEMENT_3D ( 'NONE', #29036, #3081, #28087 ) ;
#46245 = EDGE_CURVE ( 'NONE', #24728, #47328, #18346, .T. ) ;
#46246 = DIRECTION ( 'NONE',  ( -1.000000000000000000, 0.000000000000000000, -0.000000000000000000 ) ) ;
#46247 = DIRECTION ( 'NONE',  ( -1.000000000000000000, 0.000000000000000000, 0.000000000000000000 ) ) ;
#46248 = EDGE_CURVE ( 'NONE', #8812, #19820, #34098, .T. ) ;
#46249 = ORIENTED_EDGE ( 'NONE', *, *, #46970, .F. ) ;
#46250 = AXIS2_PLACEMENT_3D ( 'NONE', #6308, #17074, #36152 ) ;
#46251 = DIRECTION ( 'NONE',  ( 0.5687579148473744795, -0.8225049752423790883, 0.000000000000000000 ) ) ;
#46252 = VECTOR ( 'NONE', #11037, 1000.000000000000000 ) ;
#46253 = ORIENTED_EDGE ( 'NONE', *, *, #27703, .T. ) ;
#46254 = ORIENTED_EDGE ( 'NONE', *, *, #30777, .F. ) ;
#46255 = VERTEX_POINT ( 'NONE', #10039 ) ;
#46256 = ORIENTED_EDGE ( 'NONE', *, *, #1620, .T. ) ;
#46257 = EDGE_CURVE ( 'NONE', #11877, #11522, #12218, .T. ) ;
#46258 = ADVANCED_FACE ( 'NONE', ( #44298 ), #21773, .T. ) ;
#46259 = EDGE_CURVE ( 'NONE', #35449, #17495, #44269, .T. ) ;
#46260 = DIRECTION ( 'NONE',  ( 0.000000000000000000, -0.1564344650402170744, -0.9876883405951398798 ) ) ;
#46261 = EDGE_LOOP ( 'NONE', ( #8029, #4901, #38821, #22495 ) ) ;
#46262 = ORIENTED_EDGE ( 'NONE', *, *, #26987, .F. ) ;
#46263 = DIRECTION ( 'NONE',  ( -1.000000000000000000, 0.000000000000000000, -0.000000000000000000 ) ) ;
#46264 = ORIENTED_EDGE ( 'NONE', *, *, #4585, .T. ) ;
#46265 = CARTESIAN_POINT ( 'NONE',  ( 11.99999999999999822, 36.72794159290334903, -65.59268652807170952 ) ) ;
#46266 = CYLINDRICAL_SURFACE ( 'NONE', #2779, 16.00000000000000000 ) ;
#46267 = DIRECTION ( 'NONE',  ( 0.000000000000000000, 0.000000000000000000, -1.000000000000000000 ) ) ;
#46268 = ORIENTED_EDGE ( 'NONE', *, *, #47365, .F. ) ;
#46269 = CARTESIAN_POINT ( 'NONE',  ( 11.99999999999999822, 20.40083707022987625, -72.35432306680462489 ) ) ;
#46270 = VERTEX_POINT ( 'NONE', #40867 ) ;
#46271 = CIRCLE ( 'NONE', #44728, 77.49900000000002365 ) ;
#46272 = CARTESIAN_POINT ( 'NONE',  ( 10.00000000000000000, 0.000000000000000000, 0.000000000000000000 ) ) ;
#46273 = DIRECTION ( 'NONE',  ( -1.000000000000000000, 0.000000000000000000, 0.000000000000000000 ) ) ;
#46274 = EDGE_LOOP ( 'NONE', ( #13783, #3930, #13377, #23685 ) ) ;
#46275 = AXIS2_PLACEMENT_3D ( 'NONE', #6472, #35843, #43675 ) ;
#46276 = DIRECTION ( 'NONE',  ( 1.000000000000000000, 0.000000000000000000, 0.000000000000000000 ) ) ;
#46277 = ORIENTED_EDGE ( 'NONE', *, *, #11402, .T. ) ;
#46278 = VERTEX_POINT ( 'NONE', #7329 ) ;
#46279 = CARTESIAN_POINT ( 'NONE',  ( 15.00000000000000000, 14.60985201121729737, 18.46759930825687235 ) ) ;
#46280 = CARTESIAN_POINT ( 'NONE',  ( 11.99999999999999822, 41.76937507738875155, -62.50329211542393892 ) ) ;
#46281 = CIRCLE ( 'NONE', #40788, 31.99999999999998579 ) ;
#46282 = DIRECTION ( 'NONE',  ( -1.000000000000000000, -0.000000000000000000, 0.000000000000000000 ) ) ;
#46283 = DIRECTION ( 'NONE',  ( -1.000000000000000000, 0.000000000000000000, 0.000000000000000000 ) ) ;
#46284 = CARTESIAN_POINT ( 'NONE',  ( 0.000000000000000000, 0.000000000000000000, 0.000000000000000000 ) ) ;
#46285 = CYLINDRICAL_SURFACE ( 'NONE', #31266, 32.50000000000000000 ) ;
#46286 = CIRCLE ( 'NONE', #25160, 31.99999999999998224 ) ;
#46287 = DIRECTION ( 'NONE',  ( 0.000000000000000000, -0.9238795325112906243, 0.3826834323650805114 ) ) ;
#46288 = CARTESIAN_POINT ( 'NONE',  ( 11.99999999999999822, 0.000000000000000000, 0.000000000000000000 ) ) ;
#46289 = CARTESIAN_POINT ( 'NONE',  ( -43.60332556124591008, -123.0000000000000142, -2.500000000000000000 ) ) ;
#46290 = DIRECTION ( 'NONE',  ( 0.000000000000000000, 0.5224985647159441360, 0.8526401643540951758 ) ) ;
#46291 = LINE ( 'NONE', #4926, #9885 ) ;
#46292 = VECTOR ( 'NONE', #30322, 1000.000000000000114 ) ;
#46293 = DIRECTION ( 'NONE',  ( -1.000000000000000000, 0.000000000000000000, 0.000000000000000000 ) ) ;
#46294 = DIRECTION ( 'NONE',  ( 0.000000000000000000, -0.9510565162951500895, -0.3090169943749581649 ) ) ;
#46295 = CARTESIAN_POINT ( 'NONE',  ( 4.999999999999999112, 40.98264845739749518, 9.188173127307448951 ) ) ;
#46296 = PLANE ( 'NONE',  #31151 ) ;
#46297 = VERTEX_POINT ( 'NONE', #22270 ) ;
#46298 = VERTEX_POINT ( 'NONE', #17857 ) ;
#46299 = EDGE_CURVE ( 'NONE', #4301, #13754, #9863, .T. ) ;
#46300 = CYLINDRICAL_SURFACE ( 'NONE', #33891, 37.49900000000000233 ) ;
#46301 = CARTESIAN_POINT ( 'NONE',  ( -10.00000000000000000, 0.000000000000000000, 0.000000000000000000 ) ) ;
#46302 = ADVANCED_FACE ( 'NONE', ( #2684 ), #3663, .T. ) ;
#46303 = PRODUCT_CONTEXT ( 'NONE', #10722, 'mechanical' ) ;
#46304 = VERTEX_POINT ( 'NONE', #13728 ) ;
#46305 = DIRECTION ( 'NONE',  ( 0.000000000000000000, -0.9723699203976789995, 0.2334453638558956767 ) ) ;
#46306 = EDGE_CURVE ( 'NONE', #48285, #26114, #11455, .T. ) ;
#46307 = ORIENTED_EDGE ( 'NONE', *, *, #9217, .T. ) ;
#46308 = AXIS2_PLACEMENT_3D ( 'NONE', #13307, #40463, #28721 ) ;
#46309 = AXIS2_PLACEMENT_3D ( 'NONE', #20200, #39051, #24123 ) ;
#46310 = AXIS2_PLACEMENT_3D ( 'NONE', #40377, #17349, #6836 ) ;
#46311 = CARTESIAN_POINT ( 'NONE',  ( 0.000000000000000000, -21.60688246758530440, -79.10210256391390260 ) ) ;
#46312 = ORIENTED_EDGE ( 'NONE', *, *, #8611, .T. ) ;
#46313 = FILL_AREA_STYLE_COLOUR ( '', #46145 ) ;
#46314 = VECTOR ( 'NONE', #8415, 1000.000000000000000 ) ;
#46315 = EDGE_CURVE ( 'NONE', #47056, #24088, #32564, .T. ) ;
#46316 = EDGE_CURVE ( 'NONE', #9506, #11531, #42709, .T. ) ;
#46317 = DIRECTION ( 'NONE',  ( 0.000000000000000000, 0.1564344650402311743, -0.9876883405951377704 ) ) ;
#46318 = FACE_OUTER_BOUND ( 'NONE', #19557, .T. ) ;
#46319 = ORIENTED_EDGE ( 'NONE', *, *, #20530, .F. ) ;
#46320 = DIRECTION ( 'NONE',  ( 0.000000000000000000, 0.000000000000000000, 1.000000000000000000 ) ) ;
#46321 = AXIS2_PLACEMENT_3D ( 'NONE', #4356, #42263, #42511 ) ;
#46322 = ORIENTED_EDGE ( 'NONE', *, *, #17606, .F. ) ;
#46323 = DIRECTION ( 'NONE',  ( -1.000000000000000000, 0.000000000000000000, 0.000000000000000000 ) ) ;
#46324 = DIRECTION ( 'NONE',  ( 0.000000000000000000, 0.07845909572783793529, 0.9969173337331285190 ) ) ;
#46325 = CARTESIAN_POINT ( 'NONE',  ( 10.00000000000000000, 27.13269053701096922, 25.88420570971410228 ) ) ;
#46326 = FACE_OUTER_BOUND ( 'NONE', #20122, .T. ) ;
#46327 = ADVANCED_FACE ( 'NONE', ( #14196 ), #10528, .T. ) ;
#46328 = DIRECTION ( 'NONE',  ( 0.000000000000000000, 0.000000000000000000, -1.000000000000000000 ) ) ;
#46329 = VERTEX_POINT ( 'NONE', #22511 ) ;
#46330 = DIRECTION ( 'NONE',  ( 0.000000000000000000, 0.9781476007338043566, -0.2079116908177651712 ) ) ;
#46331 = VERTEX_POINT ( 'NONE', #37435 ) ;
#46332 = CYLINDRICAL_SURFACE ( 'NONE', #10621, 16.00000000000000000 ) ;
#46333 = ORIENTED_EDGE ( 'NONE', *, *, #29022, .F. ) ;
#46334 = CARTESIAN_POINT ( 'NONE',  ( -30.50000000000000000, -120.0000000000000000, -2.500000000000000000 ) ) ;
#46335 = DIRECTION ( 'NONE',  ( 0.000000000000000000, 0.8910065241883655673, 0.4539904997395510233 ) ) ;
#46336 = CARTESIAN_POINT ( 'NONE',  ( 11.99999999999999822, 0.000000000000000000, 0.000000000000000000 ) ) ;
#46337 = VERTEX_POINT ( 'NONE', #45264 ) ;
#46338 = DIRECTION ( 'NONE',  ( 0.000000000000000000, -0.4539904997395541320, 0.8910065241883640130 ) ) ;
#46339 = AXIS2_PLACEMENT_3D ( 'NONE', #36544, #47552, #17930 ) ;
#46340 = DIRECTION ( 'NONE',  ( -1.000000000000000000, 0.000000000000000000, -0.000000000000000000 ) ) ;
#46341 = DIRECTION ( 'NONE',  ( 0.000000000000000000, 0.000000000000000000, 1.000000000000000000 ) ) ;
#46342 = DIRECTION ( 'NONE',  ( -1.000000000000000000, -0.000000000000000000, 0.000000000000000000 ) ) ;
#46343 = DIRECTION ( 'NONE',  ( -1.000000000000000000, -0.000000000000000000, -0.000000000000000000 ) ) ;
#46344 = VECTOR ( 'NONE', #28155, 1000.000000000000000 ) ;
#46345 = CARTESIAN_POINT ( 'NONE',  ( 0.000000000000000000, 10.96151621346540317, -35.95386929396244113 ) ) ;
#46346 = DIRECTION ( 'NONE',  ( -1.000000000000000000, 0.000000000000000000, 0.000000000000000000 ) ) ;
#46347 = CARTESIAN_POINT ( 'NONE',  ( 10.00000000000000000, -26.08949754953005495, -27.05870788708258701 ) ) ;
#46348 = CIRCLE ( 'NONE', #32300, 37.49900000000000944 ) ;
#46349 = CYLINDRICAL_SURFACE ( 'NONE', #33007, 37.49900000000000233 ) ;
#46350 = CARTESIAN_POINT ( 'NONE',  ( -9.937067298023309903, 7.583184918921312523, 42.00000000000001421 ) ) ;
#46351 = AXIS2_PLACEMENT_3D ( 'NONE', #43040, #25386, #46724 ) ;
#46352 = ORIENTED_EDGE ( 'NONE', *, *, #965, .F. ) ;
#46353 = CARTESIAN_POINT ( 'NONE',  ( 10.00000000000000000, 27.05870788708267582, -26.08949754952995903 ) ) ;
#46354 = ORIENTED_EDGE ( 'NONE', *, *, #45775, .F. ) ;
#46355 = CARTESIAN_POINT ( 'NONE',  ( 0.000000000000000000, -51.29473840253177741, -63.97538442413482329 ) ) ;
#46356 = EDGE_CURVE ( 'NONE', #5626, #41024, #43485, .T. ) ;
#46357 = ORIENTED_EDGE ( 'NONE', *, *, #44695, .F. ) ;
#46358 = CARTESIAN_POINT ( 'NONE',  ( 10.00000000000000000, -37.22597642581153821, 10.79786254984320415 ) ) ;
#46359 = EDGE_CURVE ( 'NONE', #23354, #46842, #33512, .T. ) ;
#46360 = VERTEX_POINT ( 'NONE', #27159 ) ;
#46361 = EDGE_CURVE ( 'NONE', #5936, #18083, #25506, .T. ) ;
#46362 = DIRECTION ( 'NONE',  ( -1.000000000000000000, 0.000000000000000000, 0.000000000000000000 ) ) ;
#46363 = ORIENTED_EDGE ( 'NONE', *, *, #9048, .T. ) ;
#46364 = VECTOR ( 'NONE', #24975, 1000.000000000000000 ) ;
#46365 = ORIENTED_EDGE ( 'NONE', *, *, #48191, .F. ) ;
#46366 = EDGE_CURVE ( 'NONE', #12926, #371, #34469, .T. ) ;
#46367 = CIRCLE ( 'NONE', #35396, 31.99999999999998934 ) ;
#46368 = CARTESIAN_POINT ( 'NONE',  ( 0.6180191030787338669, -93.50720753887522108, 2.500000000000000000 ) ) ;
#46369 = ORIENTED_EDGE ( 'NONE', *, *, #13271, .F. ) ;
#46370 = ADVANCED_FACE ( 'NONE', ( #8050 ), #23460, .T. ) ;
#46371 = DIRECTION ( 'NONE',  ( 0.000000000000000000, 0.7071067811865439090, 0.7071067811865512365 ) ) ;
#46372 = AXIS2_PLACEMENT_3D ( 'NONE', #48135, #40793, #7742 ) ;
#46373 = AXIS2_PLACEMENT_3D ( 'NONE', #42548, #39108, #5580 ) ;
#46374 = CARTESIAN_POINT ( 'NONE',  ( -3.000000000000000000, -26.23277895567245821, -4.042438405570103477 ) ) ;
#46375 = ORIENTED_EDGE ( 'NONE', *, *, #33825, .T. ) ;
#46376 = DIRECTION ( 'NONE',  ( 0.000000000000000000, 0.000000000000000000, 1.000000000000000000 ) ) ;
#46377 = CIRCLE ( 'NONE', #38557, 15.99999999999999822 ) ;
#46378 = ORIENTED_EDGE ( 'NONE', *, *, #16202, .F. ) ;
#46379 = VECTOR ( 'NONE', #46412, 1000.000000000000000 ) ;
#46380 = ORIENTED_EDGE ( 'NONE', *, *, #19045, .F. ) ;
#46381 = DIRECTION ( 'NONE',  ( 1.000000000000000000, -0.000000000000000000, 0.000000000000000000 ) ) ;
#46382 = DIRECTION ( 'NONE',  ( 0.000000000000000000, -0.9876883405951394357, 0.1564344650402205716 ) ) ;
#46383 = FACE_OUTER_BOUND ( 'NONE', #34598, .T. ) ;
#46384 = EDGE_CURVE ( 'NONE', #12258, #39253, #15175, .T. ) ;
#46385 = ORIENTED_EDGE ( 'NONE', *, *, #26144, .T. ) ;
#46386 = AXIS2_PLACEMENT_3D ( 'NONE', #5991, #2292, #36778 ) ;
#46387 = AXIS2_PLACEMENT_3D ( 'NONE', #3051, #22396, #11134 ) ;
#46388 = ORIENTED_EDGE ( 'NONE', *, *, #34084, .T. ) ;
#46389 = ORIENTED_EDGE ( 'NONE', *, *, #35139, .F. ) ;
#46390 = DIRECTION ( 'NONE',  ( -1.000000000000000000, 0.000000000000000000, -0.000000000000000000 ) ) ;
#46391 = ORIENTED_EDGE ( 'NONE', *, *, #37028, .F. ) ;
#46392 = AXIS2_PLACEMENT_3D ( 'NONE', #21096, #47308, #43630 ) ;
#46393 = DIRECTION ( 'NONE',  ( -1.000000000000000000, 0.000000000000000000, 0.000000000000000000 ) ) ;
#46394 = AXIS2_PLACEMENT_3D ( 'NONE', #1755, #20585, #20843 ) ;
#46395 = CARTESIAN_POINT ( 'NONE',  ( -1.355716935723729089, -119.3581031311870362, -2.500000000000000000 ) ) ;
#46396 = CARTESIAN_POINT ( 'NONE',  ( 11.99999999999999822, 0.000000000000000000, 0.000000000000000000 ) ) ;
#46397 = DIRECTION ( 'NONE',  ( -0.1276937514489679404, -0.9918136447140103451, 0.000000000000000000 ) ) ;
#46398 = LINE ( 'NONE', #16784, #41561 ) ;
#46399 = DIRECTION ( 'NONE',  ( -1.000000000000000000, -0.000000000000000000, -0.000000000000000000 ) ) ;
#46400 = AXIS2_PLACEMENT_3D ( 'NONE', #44623, #10858, #14042 ) ;
#46401 = CARTESIAN_POINT ( 'NONE',  ( 6.000000000000000000, 34.94270380257741238, -74.18225833017852722 ) ) ;
#46402 = EDGE_LOOP ( 'NONE', ( #4122, #26052, #28847, #8613 ) ) ;
#46403 = DIRECTION ( 'NONE',  ( 0.000000000000000000, -1.000000000000000000, -1.047444401652940007E-14 ) ) ;
#46404 = CARTESIAN_POINT ( 'NONE',  ( 0.000000000000000000, 30.41916302227216562, -71.27951684757994144 ) ) ;
#46405 = EDGE_CURVE ( 'NONE', #11579, #33952, #4407, .T. ) ;
#46406 = LINE ( 'NONE', #24847, #33756 ) ;
#46407 = CARTESIAN_POINT ( 'NONE',  ( 70.53423027509757048, -217.0820393249931044, -5.500000000000000000 ) ) ;
#46408 = VERTEX_POINT ( 'NONE', #41845 ) ;
#46409 = EDGE_LOOP ( 'NONE', ( #28931, #14000, #40438, #26108 ) ) ;
#46410 = DIRECTION ( 'NONE',  ( 0.000000000000000000, 0.000000000000000000, -1.000000000000000000 ) ) ;
#46411 = CARTESIAN_POINT ( 'NONE',  ( 11.99999999999999822, 0.000000000000000000, 0.000000000000000000 ) ) ;
#46412 = DIRECTION ( 'NONE',  ( -0.6575728627325957421, 0.7533909544171994987, 0.000000000000000000 ) ) ;
#46413 = CARTESIAN_POINT ( 'NONE',  ( 10.00000000000000000, -62.50329211542407393, -41.76937507738853839 ) ) ;
#46414 = CARTESIAN_POINT ( 'NONE',  ( -3.000000000000000000, -4.261787119644969479, -26.19803753235780519 ) ) ;
#46415 = CARTESIAN_POINT ( 'NONE',  ( 11.99999999999999822, -73.73191006444561424, -14.66109333815538918 ) ) ;
#46416 = CARTESIAN_POINT ( 'NONE',  ( 10.00000000000000178, 0.000000000000000000, 0.000000000000000000 ) ) ;
#46417 = EDGE_LOOP ( 'NONE', ( #46857, #36943 ) ) ;
#46418 = EDGE_CURVE ( 'NONE', #27749, #38028, #8530, .T. ) ;
#46419 = VECTOR ( 'NONE', #12339, 1000.000000000000000 ) ;
#46421 = CIRCLE ( 'NONE', #4220, 77.49899999999999523 ) ;
#46420 = DIRECTION ( 'NONE',  ( -0.7273375899149802093, 0.6862798483830544471, 0.000000000000000000 ) ) ;
#46422 = CIRCLE ( 'NONE', #25288, 31.99999999999999645 ) ;
#46423 = EDGE_CURVE ( 'NONE', #33736, #5920, #8305, .T. ) ;
#46424 = VERTEX_POINT ( 'NONE', #11737 ) ;
#46425 = DIRECTION ( 'NONE',  ( 0.000000000000000000, 0.000000000000000000, 1.000000000000000000 ) ) ;
#46426 = ORIENTED_EDGE ( 'NONE', *, *, #12444, .F. ) ;
#46427 = ADVANCED_FACE ( 'NONE', ( #30572 ), #22988, .T. ) ;
#46428 = EDGE_LOOP ( 'NONE', ( #15341, #6981, #32549, #27851 ) ) ;
#46429 = AXIS2_PLACEMENT_3D ( 'NONE', #12075, #11581, #38009 ) ;
#46430 = AXIS2_PLACEMENT_3D ( 'NONE', #14021, #40940, #21616 ) ;
#46431 = EDGE_CURVE ( 'NONE', #45656, #41935, #13789, .T. ) ;
#46432 = VERTEX_POINT ( 'NONE', #26911 ) ;
#46433 = CIRCLE ( 'NONE', #22977, 82.00000000000000000 ) ;
#46434 = LINE ( 'NONE', #38857, #42153 ) ;
#46435 = ORIENTED_EDGE ( 'NONE', *, *, #44488, .F. ) ;
#46436 = AXIS2_PLACEMENT_3D ( 'NONE', #19621, #564, #15495 ) ;
#46437 = ORIENTED_EDGE ( 'NONE', *, *, #22816, .T. ) ;
#46438 = CARTESIAN_POINT ( 'NONE',  ( -10.90093335751250692, 0.000000000000000000, -13.71399988598171049 ) ) ;
#46439 = CARTESIAN_POINT ( 'NONE',  ( 0.000000000000000000, 0.000000000000000000, 0.000000000000000000 ) ) ;
#46440 = ORIENTED_EDGE ( 'NONE', *, *, #36084, .T. ) ;
#46441 = EDGE_LOOP ( 'NONE', ( #37835, #41335, #43311, #22031 ) ) ;
#46442 = ORIENTED_EDGE ( 'NONE', *, *, #28247, .T. ) ;
#46443 = CIRCLE ( 'NONE', #23763, 32.00000000000000000 ) ;
#46444 = DIRECTION ( 'NONE',  ( 0.000000000000000000, -0.1564344650402170744, -0.9876883405951398798 ) ) ;
#46446 = VERTEX_POINT ( 'NONE', #705 ) ;
#46445 = DIRECTION ( 'NONE',  ( 0.000000000000000000, 0.1564344650402244852, 0.9876883405951387696 ) ) ;
#46447 = EDGE_CURVE ( 'NONE', #2793, #28062, #15644, .T. ) ;
#46449 = CYLINDRICAL_SURFACE ( 'NONE', #36064, 82.00000000000000000 ) ;
#46448 = CIRCLE ( 'NONE', #1082, 31.99999999999999289 ) ;
#46450 = VERTEX_POINT ( 'NONE', #11981 ) ;
#46451 = DIRECTION ( 'NONE',  ( 0.1736481776669309696, 0.9848077530122080203, 0.000000000000000000 ) ) ;
#46452 = ORIENTED_EDGE ( 'NONE', *, *, #6328, .F. ) ;
#46453 = ORIENTED_EDGE ( 'NONE', *, *, #41609, .F. ) ;
#46454 = FACE_OUTER_BOUND ( 'NONE', #18168, .T. ) ;
#46455 = CIRCLE ( 'NONE', #42543, 31.99999999999998579 ) ;
#46456 = CARTESIAN_POINT ( 'NONE',  ( 0.000000000000000000, 71.21200624218852226, -40.65526001592539984 ) ) ;
#46457 = AXIS2_PLACEMENT_3D ( 'NONE', #17257, #47386, #13364 ) ;
#46458 = VERTEX_POINT ( 'NONE', #23233 ) ;
#46459 = CARTESIAN_POINT ( 'NONE',  ( -3.000000000000000000, -10.45096189432344147, 21.10159698893426494 ) ) ;
#46460 = DIRECTION ( 'NONE',  ( 0.000000000000000000, 0.000000000000000000, 1.000000000000000000 ) ) ;
#46461 = VECTOR ( 'NONE', #18447, 1000.000000000000114 ) ;
#46462 = DIRECTION ( 'NONE',  ( 0.000000000000000000, 0.000000000000000000, 1.000000000000000000 ) ) ;
#46463 = ADVANCED_FACE ( 'NONE', ( #19069 ), #480, .F. ) ;
#46464 = ORIENTED_EDGE ( 'NONE', *, *, #14026, .F. ) ;
#46465 = EDGE_LOOP ( 'NONE', ( #13300, #8504, #33501, #25986 ) ) ;
#46466 = CARTESIAN_POINT ( 'NONE',  ( 10.00000000000000000, 0.000000000000000000, 0.000000000000000000 ) ) ;
#46467 = EDGE_CURVE ( 'NONE', #18434, #773, #20025, .T. ) ;
#46468 = LINE ( 'NONE', #31065, #36040 ) ;
#46469 = AXIS2_PLACEMENT_3D ( 'NONE', #15201, #45057, #4833 ) ;
#46470 = VECTOR ( 'NONE', #47962, 1000.000000000000114 ) ;
#46471 = ORIENTED_EDGE ( 'NONE', *, *, #47028, .F. ) ;
#46472 = AXIS2_PLACEMENT_3D ( 'NONE', #26177, #14439, #44768 ) ;
#46473 = CARTESIAN_POINT ( 'NONE',  ( -3.000000000000000000, -3.948201729842038432, -23.21447184625298021 ) ) ;
#46474 = ORIENTED_EDGE ( 'NONE', *, *, #36564, .F. ) ;
#46475 = VECTOR ( 'NONE', #13437, 1000.000000000000000 ) ;
#46476 = DIRECTION ( 'NONE',  ( -1.000000000000000000, 0.000000000000000000, 0.000000000000000000 ) ) ;
#46477 = DIRECTION ( 'NONE',  ( 0.000000000000000000, 0.000000000000000000, -1.000000000000000000 ) ) ;
#46478 = CARTESIAN_POINT ( 'NONE',  ( 6.000000000000000000, 15.33399622253482697, 80.55351364060595643 ) ) ;
#46479 = DIRECTION ( 'NONE',  ( 0.000000000000000000, -0.4539904997395350361, -0.8910065241883738940 ) ) ;
#46480 = VECTOR ( 'NONE', #40798, 1000.000000000000000 ) ;
#46481 = CARTESIAN_POINT ( 'NONE',  ( -3.000000000000000000, -18.13022148937263012, 15.02647892043544608 ) ) ;
#46482 = DIRECTION ( 'NONE',  ( -1.000000000000000000, 0.000000000000000000, 0.000000000000000000 ) ) ;
#46483 = CARTESIAN_POINT ( 'NONE',  ( 11.99999999999999822, 75.16055320797057959, -18.89407956138179046 ) ) ;
#46484 = LINE ( 'NONE', #28113, #9693 ) ;
#46485 = DIRECTION ( 'NONE',  ( 1.000000000000000000, 0.000000000000000000, 0.000000000000000000 ) ) ;
#46486 = EDGE_LOOP ( 'NONE', ( #8572, #13324, #16074, #27477 ) ) ;
#46487 = EDGE_CURVE ( 'NONE', #15615, #40367, #39581, .T. ) ;
#46488 = CARTESIAN_POINT ( 'NONE',  ( 0.000000000000000000, 49.70050353004975818, -59.46389618801909904 ) ) ;
#46489 = ADVANCED_FACE ( 'NONE', ( #7582 ), #32040, .F. ) ;
#46490 =( LENGTH_UNIT ( ) NAMED_UNIT ( * ) SI_UNIT ( .MILLI., .METRE. ) );
#46491 = VERTEX_POINT ( 'NONE', #46232 ) ;
#46492 = CIRCLE ( 'NONE', #12879, 31.99999999999999289 ) ;
#46493 = EDGE_CURVE ( 'NONE', #22815, #31993, #6756, .T. ) ;
#46494 = AXIS2_PLACEMENT_3D ( 'NONE', #41742, #23608, #38550 ) ;
#46495 = AXIS2_PLACEMENT_3D ( 'NONE', #42444, #6214, #24571 ) ;
#46496 = ADVANCED_FACE ( 'NONE', ( #12703 ), #39131, .F. ) ;
#46497 = CARTESIAN_POINT ( 'NONE',  ( -10.00000000000000000, 0.000000000000000000, 0.000000000000000000 ) ) ;
#46498 = DIRECTION ( 'NONE',  ( -1.000000000000000000, 0.000000000000000000, 0.000000000000000000 ) ) ;
#46499 = ORIENTED_EDGE ( 'NONE', *, *, #27644, .F. ) ;
#46500 = VECTOR ( 'NONE', #8444, 1000.000000000000000 ) ;
#46501 = CIRCLE ( 'NONE', #20707, 31.99999999999999289 ) ;
#46502 = CIRCLE ( 'NONE', #31669, 82.00000000000000000 ) ;
#46503 = CARTESIAN_POINT ( 'NONE',  ( 0.000000000000000000, -54.21277698773715059, 55.38113227695762930 ) ) ;
#46504 = ORIENTED_EDGE ( 'NONE', *, *, #40410, .T. ) ;
#46505 = EDGE_LOOP ( 'NONE', ( #5595, #33001, #46129, #47332 ) ) ;
#46506 = ORIENTED_EDGE ( 'NONE', *, *, #4707, .F. ) ;
#46507 = AXIS2_PLACEMENT_3D ( 'NONE', #23756, #42364, #27202 ) ;
#46508 = EDGE_LOOP ( 'NONE', ( #29239, #19172, #10209, #15595 ) ) ;
#46509 = AXIS2_PLACEMENT_3D ( 'NONE', #15342, #4324, #22435 ) ;
#46510 = DIRECTION ( 'NONE',  ( 0.000000000000000000, -0.9723699203976789995, 0.2334453638558956767 ) ) ;
#46511 = EDGE_LOOP ( 'NONE', ( #39945, #38742, #35797, #20029 ) ) ;
#46512 = ORIENTED_EDGE ( 'NONE', *, *, #11632, .T. ) ;
#46513 = CARTESIAN_POINT ( 'NONE',  ( 5.999999999999999112, 46.11716303203283474, -67.80270845531839541 ) ) ;
#46514 = VERTEX_POINT ( 'NONE', #9747 ) ;
#46515 = CARTESIAN_POINT ( 'NONE',  ( 10.00000000000000000, -31.46837873494930093, -68.27212725128309501 ) ) ;
#46516 = DIRECTION ( 'NONE',  ( 0.000000000000000000, 0.000000000000000000, 1.000000000000000000 ) ) ;
#46517 = CARTESIAN_POINT ( 'NONE',  ( 11.99999999999999822, 0.000000000000000000, 0.000000000000000000 ) ) ;
#46518 = ORIENTED_EDGE ( 'NONE', *, *, #44657, .T. ) ;
#46519 = DIRECTION ( 'NONE',  ( 0.000000000000000000, -0.9876883405951394357, 0.1564344650402203496 ) ) ;
#46520 = VERTEX_POINT ( 'NONE', #20771 ) ;
#46521 = DIRECTION ( 'NONE',  ( 0.000000000000000000, 0.9510565162951544194, -0.3090169943749447867 ) ) ;
#46522 = VECTOR ( 'NONE', #24188, 1000.000000000000000 ) ;
#46523 = DIRECTION ( 'NONE',  ( 0.000000000000000000, 0.000000000000000000, 1.000000000000000000 ) ) ;
#46524 = LINE ( 'NONE', #8814, #27212 ) ;
#46525 = EDGE_LOOP ( 'NONE', ( #32950, #4887, #41262, #46154 ) ) ;
#46526 = ORIENTED_EDGE ( 'NONE', *, *, #36015, .F. ) ;
#46527 = DIRECTION ( 'NONE',  ( -1.000000000000000000, 0.000000000000000000, 0.000000000000000000 ) ) ;
#46528 = VECTOR ( 'NONE', #21651, 1000.000000000000000 ) ;
#46529 = DIRECTION ( 'NONE',  ( -1.000000000000000000, 0.000000000000000000, 0.000000000000000000 ) ) ;
#46530 = VERTEX_POINT ( 'NONE', #28112 ) ;
#46531 = EDGE_CURVE ( 'NONE', #17307, #41084, #40370, .T. ) ;
#46532 = CYLINDRICAL_SURFACE ( 'NONE', #15977, 31.99999999999998579 ) ;
#46533 = DIRECTION ( 'NONE',  ( -1.000000000000000000, 0.000000000000000000, 0.000000000000000000 ) ) ;
#46534 = DIRECTION ( 'NONE',  ( -1.000000000000000000, 0.000000000000000000, -0.000000000000000000 ) ) ;
#46535 = DIRECTION ( 'NONE',  ( -1.000000000000000000, -0.000000000000000000, -0.000000000000000000 ) ) ;
#46536 = CARTESIAN_POINT ( 'NONE',  ( 5.822613034544236399, -142.8165987265839760, 5.500000000000000000 ) ) ;
#46537 = CARTESIAN_POINT ( 'NONE',  ( 10.00000000000000000, -55.20638768913797634, 51.02545421589302777 ) ) ;
#46538 = AXIS2_PLACEMENT_3D ( 'NONE', #14776, #25287, #6461 ) ;
#46539 = PLANE ( 'NONE',  #35688 ) ;
#46540 = FACE_OUTER_BOUND ( 'NONE', #16244, .T. ) ;
#46541 = CARTESIAN_POINT ( 'NONE',  ( 0.000000000000000000, 16.00000000000000000, 2.500000000000000000 ) ) ;
#46542 = AXIS2_PLACEMENT_3D ( 'NONE', #5898, #46529, #17360 ) ;
#46543 = CARTESIAN_POINT ( 'NONE',  ( 10.00000000000000000, 27.05870788708231700, 26.08949754953034272 ) ) ;
#46544 = CARTESIAN_POINT ( 'NONE',  ( 10.00000000000000000, -67.80270845531855173, -46.11716303203261447 ) ) ;
#46545 = DIRECTION ( 'NONE',  ( 0.000000000000000000, 0.000000000000000000, 1.000000000000000000 ) ) ;
#46546 = EDGE_CURVE ( 'NONE', #7240, #10549, #8321, .T. ) ;
#46547 = LINE ( 'NONE', #35032, #7715 ) ;
#46548 = AXIS2_PLACEMENT_3D ( 'NONE', #48311, #7194, #29475 ) ;
#46549 = EDGE_CURVE ( 'NONE', #12539, #23303, #19257, .T. ) ;
#46550 = VERTEX_POINT ( 'NONE', #31815 ) ;
#46551 = EDGE_CURVE ( 'NONE', #26074, #22545, #14590, .T. ) ;
#46552 = ORIENTED_EDGE ( 'NONE', *, *, #15266, .F. ) ;
#46553 = CARTESIAN_POINT ( 'NONE',  ( 10.00000000000000000, 16.65560815589411092, 38.55633173627015964 ) ) ;
#46554 = CARTESIAN_POINT ( 'NONE',  ( -3.000000000000000000, 23.59884966291521380, 12.14883922797262805 ) ) ;
#46555 = EDGE_CURVE ( 'NONE', #15600, #32221, #9031, .T. ) ;
#46556 = CONTEXT_DEPENDENT_SHAPE_REPRESENTATION ( #43533, #30886 ) ;
#46557 = VECTOR ( 'NONE', #45266, 1000.000000000000000 ) ;
#46558 = EDGE_CURVE ( 'NONE', #17326, #31057, #5998, .T. ) ;
#46559 = CARTESIAN_POINT ( 'NONE',  ( 10.00000000000000000, 0.000000000000000000, 0.000000000000000000 ) ) ;
#46560 = VERTEX_POINT ( 'NONE', #24685 ) ;
#46561 = AXIS2_PLACEMENT_3D ( 'NONE', #20890, #31684, #28224 ) ;
#46562 = CARTESIAN_POINT ( 'NONE',  ( 10.00000000000000000, 33.00180498840046539, 17.80606268964551120 ) ) ;
#46563 = CARTESIAN_POINT ( 'NONE',  ( 10.00000000000000000, -30.80686688396994910, -21.53537804866113703 ) ) ;
#46564 = EDGE_LOOP ( 'NONE', ( #20470, #7373, #25518, #11237, #16162, #42117 ) ) ;
#46565 = DIRECTION ( 'NONE',  ( 0.000000000000000000, 0.000000000000000000, 1.000000000000000000 ) ) ;
#46566 = CIRCLE ( 'NONE', #30150, 42.00000000000000000 ) ;
#46567 = AXIS2_PLACEMENT_3D ( 'NONE', #33253, #40374, #44272 ) ;
#46568 = DIRECTION ( 'NONE',  ( -1.000000000000000000, 0.000000000000000000, -0.000000000000000000 ) ) ;
#46569 = ORIENTED_EDGE ( 'NONE', *, *, #2636, .F. ) ;
#46570 = LINE ( 'NONE', #38252, #6310 ) ;
#46571 = EDGE_LOOP ( 'NONE', ( #41731, #44390, #45896, #40518 ) ) ;
#46572 = CARTESIAN_POINT ( 'NONE',  ( 0.000000000000000000, 0.000000000000000000, 0.000000000000000000 ) ) ;
#46573 = ORIENTED_EDGE ( 'NONE', *, *, #27768, .T. ) ;
#46574 = CIRCLE ( 'NONE', #19971, 31.99999999999998579 ) ;
#46575 = VERTEX_POINT ( 'NONE', #19783 ) ;
#46576 = CARTESIAN_POINT ( 'NONE',  ( 2.047646702416564768, -96.54137380445985173, 5.500000000000000000 ) ) ;
#46577 = AXIS2_PLACEMENT_3D ( 'NONE', #34105, #38034, #20143 ) ;
#46578 = LINE ( 'NONE', #42412, #37080 ) ;
#46579 = DIRECTION ( 'NONE',  ( -1.000000000000000000, -0.000000000000000000, -0.000000000000000000 ) ) ;
#46580 = DIRECTION ( 'NONE',  ( 0.000000000000000000, 0.7431448254773954654, -0.6691306063588569053 ) ) ;
#46581 = CARTESIAN_POINT ( 'NONE',  ( 0.000000000000000000, -120.0000000000000000, 2.500000000000000000 ) ) ;
#46582 = EDGE_CURVE ( 'NONE', #41890, #18915, #16374, .T. ) ;
#46583 = ORIENTED_EDGE ( 'NONE', *, *, #42213, .F. ) ;
#46584 = CARTESIAN_POINT ( 'NONE',  ( 0.000000000000000000, -2.956366410620109519, -75.11725578898472122 ) ) ;
#46585 = VERTEX_POINT ( 'NONE', #13187 ) ;
#46586 = ORIENTED_EDGE ( 'NONE', *, *, #46910, .T. ) ;
#46587 = DIRECTION ( 'NONE',  ( 1.000000000000000000, -0.000000000000000000, 0.000000000000000000 ) ) ;
#46588 = ORIENTED_EDGE ( 'NONE', *, *, #39027, .T. ) ;
#46589 = EDGE_CURVE ( 'NONE', #34506, #20063, #41185, .T. ) ;
#46590 = LINE ( 'NONE', #13056, #20614 ) ;
#46591 = AXIS2_PLACEMENT_3D ( 'NONE', #2790, #6236, #6008 ) ;
#46592 = CARTESIAN_POINT ( 'NONE',  ( 0.000000000000000000, 62.20884554314020676, 46.21855187248652896 ) ) ;
#46593 = DIRECTION ( 'NONE',  ( 1.000000000000000000, 0.000000000000000000, 0.000000000000000000 ) ) ;
#46594 = ORIENTED_EDGE ( 'NONE', *, *, #9513, .F. ) ;
#46595 = PLANE ( 'NONE',  #31621 ) ;
#46596 = CIRCLE ( 'NONE', #27840, 42.00000000000000000 ) ;
#46597 = ADVANCED_FACE ( 'NONE', ( #31561 ), #46001, .T. ) ;
#46598 = DIRECTION ( 'NONE',  ( -1.000000000000000000, -0.000000000000000000, 0.000000000000000000 ) ) ;
#46599 = LINE ( 'NONE', #34580, #20364 ) ;
#46600 = DIRECTION ( 'NONE',  ( -0.000000000000000000, -0.7431448254773870277, -0.6691306063588662312 ) ) ;
#46601 = AXIS2_PLACEMENT_3D ( 'NONE', #9088, #43097, #35752 ) ;
#46602 = DIRECTION ( 'NONE',  ( -1.000000000000000000, 0.000000000000000000, -0.000000000000000000 ) ) ;
#46603 = DIRECTION ( 'NONE',  ( -1.000000000000000000, 0.000000000000000000, -0.000000000000000000 ) ) ;
#46604 = FILL_AREA_STYLE ('',( #16736 ) ) ;
#46605 = DIRECTION ( 'NONE',  ( -1.000000000000000000, 0.000000000000000000, 0.000000000000000000 ) ) ;
#46606 = CARTESIAN_POINT ( 'NONE',  ( 5.000000000000000000, 79.10210256391368944, 21.60688246758614284 ) ) ;
#46607 = CARTESIAN_POINT ( 'NONE',  ( 10.00000000000000000, -29.81001611430991360, -22.74946021919165418 ) ) ;
#46608 = AXIS2_PLACEMENT_3D ( 'NONE', #9201, #35379, #8958 ) ;
#46609 = EDGE_CURVE ( 'NONE', #14073, #13144, #23711, .T. ) ;
#46610 = EDGE_CURVE ( 'NONE', #31375, #36483, #35716, .T. ) ;
#46611 = AXIS2_PLACEMENT_3D ( 'NONE', #20486, #36143, #21206 ) ;
#46612 = CARTESIAN_POINT ( 'NONE',  ( 10.00000000000000000, 73.95703589263975175, 23.16143007188454206 ) ) ;
#46613 = ORIENTED_EDGE ( 'NONE', *, *, #10394, .F. ) ;
#46614 = CARTESIAN_POINT ( 'NONE',  ( 6.377742925735834234, -145.7647898336708181, -5.500000000000000000 ) ) ;
#46615 = AXIS2_PLACEMENT_3D ( 'NONE', #31436, #46343, #12818 ) ;
#46616 = DIRECTION ( 'NONE',  ( 1.000000000000000000, 0.000000000000000000, 0.000000000000000000 ) ) ;
#46617 = VERTEX_POINT ( 'NONE', #16609 ) ;
#46618 = EDGE_CURVE ( 'NONE', #23653, #16881, #1940, .T. ) ;
#46619 = DIRECTION ( 'NONE',  ( -1.000000000000000000, 0.000000000000000000, 0.000000000000000000 ) ) ;
#46620 = AXIS2_PLACEMENT_3D ( 'NONE', #763, #30405, #15703 ) ;
#46621 = VERTEX_POINT ( 'NONE', #24196 ) ;
#46622 = AXIS2_PLACEMENT_3D ( 'NONE', #7375, #33786, #3946 ) ;
#46623 = ORIENTED_EDGE ( 'NONE', *, *, #33477, .T. ) ;
#46624 = AXIS2_PLACEMENT_3D ( 'NONE', #6613, #21545, #36469 ) ;
#46625 = CARTESIAN_POINT ( 'NONE',  ( 15.00000000000000000, 14.60985201121703980, -18.46759930825707841 ) ) ;
#46626 = DIRECTION ( 'NONE',  ( -1.000000000000000000, -0.000000000000000000, -0.000000000000000000 ) ) ;
#46628 = VERTEX_POINT ( 'NONE', #5604 ) ;
#46627 = CARTESIAN_POINT ( 'NONE',  ( 21.07894319797337701, -103.8699611390234878, 5.500000000000000000 ) ) ;
#46629 = VERTEX_POINT ( 'NONE', #5854 ) ;
#46630 = CARTESIAN_POINT ( 'NONE',  ( 15.00000000000000000, -13.04903810567646971, 19.60159698893442481 ) ) ;
#46631 = VERTEX_POINT ( 'NONE', #35452 ) ;
#46632 = CARTESIAN_POINT ( 'NONE',  ( 0.000000000000000000, 0.000000000000000000, 0.000000000000000000 ) ) ;
#46633 = FACE_OUTER_BOUND ( 'NONE', #35280, .T. ) ;
#46634 = EDGE_CURVE ( 'NONE', #7136, #6044, #20054, .T. ) ;
#46635 = FACE_OUTER_BOUND ( 'NONE', #16945, .T. ) ;
#46636 = AXIS2_PLACEMENT_3D ( 'NONE', #42539, #16347, #4603 ) ;
#46637 = EDGE_CURVE ( 'NONE', #26953, #11582, #536, .T. ) ;
#46638 = VERTEX_POINT ( 'NONE', #40348 ) ;
#46639 = VERTEX_POINT ( 'NONE', #47900 ) ;
#46640 = DIRECTION ( 'NONE',  ( -1.000000000000000000, -0.000000000000000000, -0.000000000000000000 ) ) ;
#46641 = ORIENTED_EDGE ( 'NONE', *, *, #39400, .F. ) ;
#46642 = LINE ( 'NONE', #6479, #40293 ) ;
#46643 = EDGE_CURVE ( 'NONE', #41886, #19983, #13672, .T. ) ;
#46644 = CIRCLE ( 'NONE', #18501, 31.99999999999998934 ) ;
#46645 = DIRECTION ( 'NONE',  ( -0.000000000000000000, -0.000000000000000000, -1.000000000000000000 ) ) ;
#46646 = CARTESIAN_POINT ( 'NONE',  ( 10.00000000000000178, 12.24744871391589029, 2.499999999999999556 ) ) ;
#46647 = LINE ( 'NONE', #31237, #40968 ) ;
#46648 = DIRECTION ( 'NONE',  ( -1.000000000000000000, 0.000000000000000000, 0.000000000000000000 ) ) ;
#46649 = DIRECTION ( 'NONE',  ( -1.000000000000000000, -0.000000000000000000, 0.000000000000000000 ) ) ;
#46650 = ADVANCED_FACE ( 'NONE', ( #6806 ), #13905, .F. ) ;
#46651 = LINE ( 'NONE', #13351, #33026 ) ;
#46652 = ORIENTED_EDGE ( 'NONE', *, *, #31188, .T. ) ;
#46653 = DIRECTION ( 'NONE',  ( 0.000000000000000000, -0.6494480483301739993, -0.7604059656000392575 ) ) ;
#46654 = DIRECTION ( 'NONE',  ( -1.000000000000000000, 0.000000000000000000, 0.000000000000000000 ) ) ;
#46655 = LINE ( 'NONE', #47117, #4837 ) ;
#46656 = DIRECTION ( 'NONE',  ( -1.000000000000000000, -0.000000000000000000, 0.000000000000000000 ) ) ;
#46657 = EDGE_LOOP ( 'NONE', ( #31776, #45072, #30965, #7980 ) ) ;
#46658 = VECTOR ( 'NONE', #4621, 1000.000000000000000 ) ;
#46659 = ORIENTED_EDGE ( 'NONE', *, *, #30713, .T. ) ;
#46660 = CYLINDRICAL_SURFACE ( 'NONE', #41929, 31.99999999999998579 ) ;
#46661 = FACE_OUTER_BOUND ( 'NONE', #34933, .T. ) ;
#46662 = CARTESIAN_POINT ( 'NONE',  ( 20.07203437053270179, -132.2214334768125354, -2.500000000000000000 ) ) ;
#46663 = COLOUR_RGB ( '', 0.40784314, 0.44705882, 0.49803922) ;
#46664 = EDGE_CURVE ( 'NONE', #30440, #23468, #21727, .T. ) ;
#46665 = EDGE_CURVE ( 'NONE', #24209, #1357, #36647, .T. ) ;
#46666 = DIRECTION ( 'NONE',  ( -1.000000000000000000, -0.000000000000000000, 0.000000000000000000 ) ) ;
#46667 = DIRECTION ( 'NONE',  ( 0.000000000000000000, -0.5877852522924801315, 0.8090169943749423442 ) ) ;
#46668 = AXIS2_PLACEMENT_3D ( 'NONE', #22214, #48390, #14871 ) ;
#46669 = DIRECTION ( 'NONE',  ( -1.000000000000000000, 0.000000000000000000, 0.000000000000000000 ) ) ;
#46670 = FACE_OUTER_BOUND ( 'NONE', #23382, .T. ) ;
#46671 = ADVANCED_FACE ( 'NONE', ( #18039 ), #25870, .T. ) ;
#46672 = VERTEX_POINT ( 'NONE', #43999 ) ;
#46673 = DIRECTION ( 'NONE',  ( 0.000000000000000000, -0.8090169943749422332, -0.5877852522924803536 ) ) ;
#46674 = VERTEX_POINT ( 'NONE', #28827 ) ;
#46675 = DIRECTION ( 'NONE',  ( 0.000000000000000000, 0.000000000000000000, -1.000000000000000000 ) ) ;
#46676 = ORIENTED_EDGE ( 'NONE', *, *, #17686, .F. ) ;
#46677 = ORIENTED_EDGE ( 'NONE', *, *, #28693, .T. ) ;
#46678 = CONICAL_SURFACE ( 'NONE', #2123, 15.39727592589476579, 0.2094395102393128150 ) ;
#46679 = ORIENTED_EDGE ( 'NONE', *, *, #28149, .T. ) ;
#46680 = EDGE_CURVE ( 'NONE', #1027, #18777, #10473, .T. ) ;
#46681 = AXIS2_PLACEMENT_3D ( 'NONE', #15805, #393, #4320 ) ;
#46682 =( REPRESENTATION_RELATIONSHIP ('NONE','NONE', #5957, #29385 ) REPRESENTATION_RELATIONSHIP_WITH_TRANSFORMATION ( #19147 )SHAPE_REPRESENTATION_RELATIONSHIP( ) );
#46683 = ORIENTED_EDGE ( 'NONE', *, *, #17736, .T. ) ;
#46684 = VECTOR ( 'NONE', #15643, 1000.000000000000000 ) ;
#46685 = CARTESIAN_POINT ( 'NONE',  ( 10.00000000000000000, -30.41916302227060598, -71.27951684758059514 ) ) ;
#46686 = ORIENTED_EDGE ( 'NONE', *, *, #3455, .F. ) ;
#46687 = VECTOR ( 'NONE', #33092, 1000.000000000000000 ) ;
#46688 = DIRECTION ( 'NONE',  ( 0.000000000000000000, 0.000000000000000000, 1.000000000000000000 ) ) ;
#46690 = ORIENTED_EDGE ( 'NONE', *, *, #16699, .F. ) ;
#46689 = DIRECTION ( 'NONE',  ( 0.000000000000000000, 0.7071067811865487940, -0.7071067811865462405 ) ) ;
#46691 = VERTEX_POINT ( 'NONE', #25390 ) ;
#46692 = ORIENTED_EDGE ( 'NONE', *, *, #42342, .T. ) ;
#46693 = ORIENTED_EDGE ( 'NONE', *, *, #23601, .T. ) ;
#46694 = DIRECTION ( 'NONE',  ( 0.000000000000000000, 0.07845909572784512398, -0.9969173337331279638 ) ) ;
#46696 = ORIENTED_EDGE ( 'NONE', *, *, #30515, .T. ) ;
#46695 = CARTESIAN_POINT ( 'NONE',  ( 11.99999999999999822, 0.000000000000000000, 0.000000000000000000 ) ) ;
#46697 = DIRECTION ( 'NONE',  ( 0.000000000000000000, 0.7071067811865489050, -0.7071067811865462405 ) ) ;
#46698 = ORIENTED_EDGE ( 'NONE', *, *, #27913, .F. ) ;
#46699 = VERTEX_POINT ( 'NONE', #28604 ) ;
#46700 = DIRECTION ( 'NONE',  ( -1.000000000000000000, 0.000000000000000000, 0.000000000000000000 ) ) ;
#46701 = ORIENTED_EDGE ( 'NONE', *, *, #34036, .F. ) ;
#46702 = DIRECTION ( 'NONE',  ( -1.000000000000000000, 0.000000000000000000, 0.000000000000000000 ) ) ;
#46703 = CARTESIAN_POINT ( 'NONE',  ( 10.00000000000000000, -35.92658777277502935, -10.74501242461320594 ) ) ;
#46704 = EDGE_CURVE ( 'NONE', #37684, #22174, #14390, .T. ) ;
#46705 = CYLINDRICAL_SURFACE ( 'NONE', #10388, 77.49899999999999523 ) ;
#46706 = CARTESIAN_POINT ( 'NONE',  ( 2.117611129180199558, -93.54218975225703048, -2.500000000000000444 ) ) ;
#46707 = LINE ( 'NONE', #27875, #41666 ) ;
#46708 = EDGE_CURVE ( 'NONE', #29332, #44202, #25630, .T. ) ;
#46709 = ORIENTED_EDGE ( 'NONE', *, *, #10342, .F. ) ;
#46710 = EDGE_CURVE ( 'NONE', #16544, #24524, #33228, .T. ) ;
#46711 = ORIENTED_EDGE ( 'NONE', *, *, #2641, .F. ) ;
#46712 = DIRECTION ( 'NONE',  ( -1.000000000000000000, 0.000000000000000000, -0.000000000000000000 ) ) ;
#46713 = CARTESIAN_POINT ( 'NONE',  ( 10.00000000000000000, 3.925862922256769583, -41.81611651403858332 ) ) ;
#46714 = VECTOR ( 'NONE', #19402, 1000.000000000000000 ) ;
#46716 = EDGE_CURVE ( 'NONE', #15261, #5216, #21233, .T. ) ;
#46715 = EDGE_LOOP ( 'NONE', ( #46652, #5305, #38631, #11757 ) ) ;
#46717 = EDGE_CURVE ( 'NONE', #6187, #15600, #2392, .T. ) ;
#46718 = DIRECTION ( 'NONE',  ( -1.000000000000000000, 0.000000000000000000, 0.000000000000000000 ) ) ;
#46719 = VERTEX_POINT ( 'NONE', #47193 ) ;
#46720 = DIRECTION ( 'NONE',  ( 0.000000000000000000, -0.9876883405951393247, 0.1564344650402205161 ) ) ;
#46721 = CIRCLE ( 'NONE', #20919, 16.00000000000000000 ) ;
#46722 = DIRECTION ( 'NONE',  ( -0.000000000000000000, -0.000000000000000000, -1.000000000000000000 ) ) ;
#46723 = FACE_OUTER_BOUND ( 'NONE', #6988, .T. ) ;
#46724 = DIRECTION ( 'NONE',  ( 0.000000000000000000, -0.4539904997395350916, -0.8910065241883738940 ) ) ;
#46725 = DIRECTION ( 'NONE',  ( -1.000000000000000000, 0.000000000000000000, 0.000000000000000000 ) ) ;
#46726 = CARTESIAN_POINT ( 'NONE',  ( 0.000000000000000000, 0.000000000000000000, 0.000000000000000000 ) ) ;
#46727 = VERTEX_POINT ( 'NONE', #43530 ) ;
#46728 = AXIS2_PLACEMENT_3D ( 'NONE', #10600, #32620, #47542 ) ;
#46729 = CARTESIAN_POINT ( 'NONE',  ( -3.000000000000000000, 16.83928648764945279, -16.46020748918028076 ) ) ;
#46730 = DIRECTION ( 'NONE',  ( 0.000000000000000000, 0.000000000000000000, 1.000000000000000000 ) ) ;
#46731 = CARTESIAN_POINT ( 'NONE',  ( 0.000000000000000000, 0.000000000000000000, 0.000000000000000000 ) ) ;
#46732 = EDGE_CURVE ( 'NONE', #3614, #25227, #32733, .T. ) ;
#46733 = DIRECTION ( 'NONE',  ( -1.000000000000000000, 0.000000000000000000, -0.000000000000000000 ) ) ;
#46734 = SHAPE_REPRESENTATION_RELATIONSHIP ( 'NONE' , 'NONE' ,  #40966, #605 ) ;
#46735 = ORIENTED_EDGE ( 'NONE', *, *, #33039, .T. ) ;
#46736 = VERTEX_POINT ( 'NONE', #24916 ) ;
#46737 = ORIENTED_EDGE ( 'NONE', *, *, #37141, .F. ) ;
#46738 = AXIS2_PLACEMENT_3D ( 'NONE', #40748, #33637, #22626 ) ;
#46739 = EDGE_CURVE ( 'NONE', #39596, #30049, #20868, .T. ) ;
#46740 = CARTESIAN_POINT ( 'NONE',  ( 11.99999999999999822, 0.000000000000000000, 0.000000000000000000 ) ) ;
#46741 = CARTESIAN_POINT ( 'NONE',  ( -22.67106064244953245, -113.6342314410295842, 5.500000000000000000 ) ) ;
#46742 = ORIENTED_EDGE ( 'NONE', *, *, #42948, .F. ) ;
#46743 = EDGE_CURVE ( 'NONE', #38555, #15249, #47421, .T. ) ;
#46744 = AXIS2_PLACEMENT_3D ( 'NONE', #264, #29890, #22789 ) ;
#46745 = CARTESIAN_POINT ( 'NONE',  ( 0.000000000000000000, 0.000000000000000000, 0.000000000000000000 ) ) ;
#46746 = DIRECTION ( 'NONE',  ( -1.000000000000000000, 0.000000000000000000, 0.000000000000000000 ) ) ;
#46747 = AXIS2_PLACEMENT_3D ( 'NONE', #40465, #34909, #1390 ) ;
#46748 = ORIENTED_EDGE ( 'NONE', *, *, #23669, .F. ) ;
#46749 = ORIENTED_EDGE ( 'NONE', *, *, #40834, .T. ) ;
#46750 = ORIENTED_EDGE ( 'NONE', *, *, #26851, .F. ) ;
#46751 = VECTOR ( 'NONE', #34681, 999.9999999999998863 ) ;
#46752 = EDGE_CURVE ( 'NONE', #12206, #30376, #2882, .T. ) ;
#46753 = DIRECTION ( 'NONE',  ( -1.000000000000000000, 0.000000000000000000, 0.000000000000000000 ) ) ;
#46754 = ORIENTED_EDGE ( 'NONE', *, *, #22465, .F. ) ;
#46755 = DIRECTION ( 'NONE',  ( 0.000000000000000000, 0.000000000000000000, 1.000000000000000000 ) ) ;
#46756 = ORIENTED_EDGE ( 'NONE', *, *, #47613, .F. ) ;
#46757 = EDGE_CURVE ( 'NONE', #16336, #39882, #14145, .T. ) ;
#46758 = CARTESIAN_POINT ( 'NONE',  ( 10.00000000000000000, 41.19522573413826194, -65.64334221924865176 ) ) ;
#46759 = DIRECTION ( 'NONE',  ( 0.000000000000000000, 0.000000000000000000, 1.000000000000000000 ) ) ;
#46760 = ADVANCED_FACE ( 'NONE', ( #7760 ), #33699, .T. ) ;
#46761 = CARTESIAN_POINT ( 'NONE',  ( 11.99999999999999822, 59.03342792756263435, 46.54456581323825048 ) ) ;
#46762 = ORIENTED_EDGE ( 'NONE', *, *, #6457, .F. ) ;
#46763 = ADVANCED_FACE ( 'NONE', ( #11682 ), #45216, .T. ) ;
#46764 = LINE ( 'NONE', #33448, #9474 ) ;
#46765 = VERTEX_POINT ( 'NONE', #34409 ) ;
#46766 = ORIENTED_EDGE ( 'NONE', *, *, #1644, .T. ) ;
#46767 = CIRCLE ( 'NONE', #13911, 16.00000000000000000 ) ;
#46768 = CARTESIAN_POINT ( 'NONE',  ( 6.000000000000000000, -81.90746397400386059, -3.894527615418766242 ) ) ;
#46769 = DIRECTION ( 'NONE',  ( 0.000000000000000000, 0.000000000000000000, 1.000000000000000000 ) ) ;
#46770 = CARTESIAN_POINT ( 'NONE',  ( 0.000000000000000000, -51.02545421589363883, 55.20638768913742922 ) ) ;
#46771 = ORIENTED_EDGE ( 'NONE', *, *, #44195, .T. ) ;
#46772 = ORIENTED_EDGE ( 'NONE', *, *, #15487, .T. ) ;
#46773 = ADVANCED_FACE ( 'NONE', ( #15113 ), #3607, .T. ) ;
#46774 = LINE ( 'NONE', #21275, #16629 ) ;
#46775 = CARTESIAN_POINT ( 'NONE',  ( 23.41451323550360186, -132.5004227906269989, 2.500000000000000000 ) ) ;
#46776 = ORIENTED_EDGE ( 'NONE', *, *, #32793, .F. ) ;
#46777 = CARTESIAN_POINT ( 'NONE',  ( 3.429551818649054340, -146.3199197248623875, 5.500000000000000000 ) ) ;
#46778 = DIRECTION ( 'NONE',  ( -0.8225049752423791993, -0.5687579148473745905, 0.000000000000000000 ) ) ;
#46779 = DIRECTION ( 'NONE',  ( -1.000000000000000000, 0.000000000000000000, 0.000000000000000000 ) ) ;
#46780 = DIRECTION ( 'NONE',  ( 0.000000000000000000, 0.9876883405951383255, -0.1564344650402277048 ) ) ;
#46781 = DIRECTION ( 'NONE',  ( 0.000000000000000000, -0.8090169943749530024, 0.5877852522924653655 ) ) ;
#46782 = DIRECTION ( 'NONE',  ( 0.000000000000000000, 0.000000000000000000, 1.000000000000000000 ) ) ;
#46783 = DIRECTION ( 'NONE',  ( -1.000000000000000000, 0.000000000000000000, 0.000000000000000000 ) ) ;
#46784 = AXIS2_PLACEMENT_3D ( 'NONE', #9717, #40327, #39837 ) ;
#46785 = DIRECTION ( 'NONE',  ( -1.000000000000000000, -0.000000000000000000, -0.000000000000000000 ) ) ;
#46786 = CARTESIAN_POINT ( 'NONE',  ( 0.000000000000000000, 39.04073710021344112, 15.48615015657596672 ) ) ;
#46787 = DIRECTION ( 'NONE',  ( -1.000000000000000000, 0.000000000000000000, -0.000000000000000000 ) ) ;
#46789 = AXIS2_PLACEMENT_3D ( 'NONE', #39039, #23868, #5506 ) ;
#46788 = DIRECTION ( 'NONE',  ( 0.000000000000000000, 0.000000000000000000, 1.000000000000000000 ) ) ;
#46790 = LINE ( 'NONE', #16920, #44381 ) ;
#46791 = ORIENTED_EDGE ( 'NONE', *, *, #34726, .T. ) ;
#46792 = ORIENTED_EDGE ( 'NONE', *, *, #38670, .F. ) ;
#46793 = DIRECTION ( 'NONE',  ( -1.000000000000000000, 0.000000000000000000, -0.000000000000000000 ) ) ;
#46794 = CARTESIAN_POINT ( 'NONE',  ( 15.00000000000000000, 14.60985201121703980, -18.46759930825707841 ) ) ;
#46795 =( GEOMETRIC_REPRESENTATION_CONTEXT ( 3 ) GLOBAL_UNCERTAINTY_ASSIGNED_CONTEXT ( ( #40409 ) ) GLOBAL_UNIT_ASSIGNED_CONTEXT ( ( #16559, #1143, #16094 ) ) REPRESENTATION_CONTEXT ( 'NONE', 'WORKASPACE' ) );
#46796 = DIRECTION ( 'NONE',  ( -1.000000000000000000, -0.000000000000000000, 0.000000000000000000 ) ) ;
#46797 = VERTEX_POINT ( 'NONE', #7991 ) ;
#46798 = AXIS2_PLACEMENT_3D ( 'NONE', #4467, #4225, #30900 ) ;
#46799 = CARTESIAN_POINT ( 'NONE',  ( -10.00000000000000000, 0.000000000000000000, 0.000000000000000000 ) ) ;
#46800 = ORIENTED_EDGE ( 'NONE', *, *, #45342, .T. ) ;
#46801 = CARTESIAN_POINT ( 'NONE',  ( -3.000000000000000000, -19.89357724625003598, 12.59942793731059574 ) ) ;
#46802 = ORIENTED_EDGE ( 'NONE', *, *, #22093, .T. ) ;
#46803 = CARTESIAN_POINT ( 'NONE',  ( 0.000000000000000000, -58.39081064771787766, 50.95692526931307498 ) ) ;
#46804 = DIRECTION ( 'NONE',  ( 0.000000000000000000, -0.8660254037844421493, -0.4999999999999939493 ) ) ;
#46805 = ORIENTED_EDGE ( 'NONE', *, *, #8119, .F. ) ;
#46806 = ADVANCED_FACE ( 'NONE', ( #8250 ), #18761, .F. ) ;
#46808 = VERTEX_POINT ( 'NONE', #41788 ) ;
#46807 = FACE_OUTER_BOUND ( 'NONE', #14670, .T. ) ;
#46809 = VERTEX_POINT ( 'NONE', #4097 ) ;
#46810 = CIRCLE ( 'NONE', #42127, 16.00000000000000000 ) ;
#46811 = ADVANCED_FACE ( 'NONE', ( #19005 ), #45444, .T. ) ;
#46812 = VECTOR ( 'NONE', #8501, 1000.000000000000000 ) ;
#46813 = CARTESIAN_POINT ( 'NONE',  ( -1.250000000000000000, -12.36245420541525597, -1.199999999999999956 ) ) ;
#46814 = DIRECTION ( 'NONE',  ( 0.000000000000000000, -0.8660254037844437036, 0.4999999999999913403 ) ) ;
#46815 = LINE ( 'NONE', #43616, #45044 ) ;
#46816 = EDGE_CURVE ( 'NONE', #22498, #28068, #38113, .T. ) ;
#46817 = LINE ( 'NONE', #36020, #27350 ) ;
#46818 = EDGE_LOOP ( 'NONE', ( #31507, #6699, #34275, #190 ) ) ;
#46819 = CARTESIAN_POINT ( 'NONE',  ( 11.99999999999999822, 0.000000000000000000, 0.000000000000000000 ) ) ;
#46820 = ORIENTED_EDGE ( 'NONE', *, *, #9565, .T. ) ;
#46821 = ORIENTED_EDGE ( 'NONE', *, *, #30753, .F. ) ;
#46822 = EDGE_CURVE ( 'NONE', #2634, #36936, #11478, .T. ) ;
#46823 = CARTESIAN_POINT ( 'NONE',  ( 0.000000000000000000, 33.79645857604513992, 16.45098606841138178 ) ) ;
#46824 = VERTEX_POINT ( 'NONE', #40811 ) ;
#46825 = CARTESIAN_POINT ( 'NONE',  ( 11.99999999999999822, -70.52718814184277107, 26.02418014898285037 ) ) ;
#46826 = ADVANCED_FACE ( 'NONE', ( #41306 ), #41542, .T. ) ;
#46827 = DIRECTION ( 'NONE',  ( -1.000000000000000000, 0.000000000000000000, -0.000000000000000000 ) ) ;
#46828 = CARTESIAN_POINT ( 'NONE',  ( 10.00000000000000000, 37.22597642581150268, 5.202137450157037435 ) ) ;
#46829 = VERTEX_POINT ( 'NONE', #19479 ) ;
#46830 = DIRECTION ( 'NONE',  ( 0.000000000000000000, 0.000000000000000000, 1.000000000000000000 ) ) ;
#46831 = PRODUCT ( 'slow gear_ISO - Spur gear 2M 80T 20PA 12FW ---S80A75H50L38.0N', 'slow gear_ISO - Spur gear 2M 80T 20PA 12FW ---S80A75H50L38.0N', '', ( #4474 ) ) ;
#46832 = CARTESIAN_POINT ( 'NONE',  ( 15.00000000000000000, -0.9646360437375368635, -23.52805723605589705 ) ) ;
#46833 = CARTESIAN_POINT ( 'NONE',  ( -15.44521549751111422, -137.7748507232956001, 5.500000000000000000 ) ) ;
#46834 = MECHANICAL_DESIGN_GEOMETRIC_PRESENTATION_REPRESENTATION (  '', ( #39811 ), #44480 ) ;
#46835 = DIRECTION ( 'NONE',  ( 0.000000000000000000, 0.000000000000000000, -1.000000000000000000 ) ) ;
#46836 = DIRECTION ( 'NONE',  ( 0.6516173805718078471, -0.7585478161175706058, 0.000000000000000000 ) ) ;
#46837 = DIRECTION ( 'NONE',  ( 1.000000000000000000, 0.000000000000000000, 0.000000000000000000 ) ) ;
#46838 = DIRECTION ( 'NONE',  ( -1.000000000000000000, -0.000000000000000000, -0.000000000000000000 ) ) ;
#46839 = CARTESIAN_POINT ( 'NONE',  ( 11.99999999999999822, 0.000000000000000000, 0.000000000000000000 ) ) ;
#46840 = DIRECTION ( 'NONE',  ( -1.000000000000000000, 0.000000000000000000, 0.000000000000000000 ) ) ;
#46841 = DIRECTION ( 'NONE',  ( 0.000000000000000000, -0.8910065241883626808, -0.4539904997395568520 ) ) ;
#46842 = VERTEX_POINT ( 'NONE', #22927 ) ;
#46843 = LINE ( 'NONE', #8907, #7387 ) ;
#46844 = VECTOR ( 'NONE', #34202, 1000.000000000000000 ) ;
#46845 = ORIENTED_EDGE ( 'NONE', *, *, #43976, .F. ) ;
#46846 = DIRECTION ( 'NONE',  ( -1.000000000000000000, 0.000000000000000000, 0.000000000000000000 ) ) ;
#46847 = CIRCLE ( 'NONE', #8533, 31.99999999999998579 ) ;
#46848 = AXIS2_PLACEMENT_3D ( 'NONE', #19278, #23198, #11700 ) ;
#46849 = VERTEX_POINT ( 'NONE', #37623 ) ;
#46850 = CARTESIAN_POINT ( 'NONE',  ( -10.00000000000000000, 0.000000000000000000, 0.000000000000000000 ) ) ;
#46851 = ORIENTED_EDGE ( 'NONE', *, *, #19191, .F. ) ;
#46852 = EDGE_CURVE ( 'NONE', #19636, #14109, #22410, .T. ) ;
#46853 = EDGE_CURVE ( 'NONE', #31655, #45354, #658, .T. ) ;
#46854 = CARTESIAN_POINT ( 'NONE',  ( 23.11608002360578240, -124.4885236261218182, -5.500000000000000000 ) ) ;
#46855 = ORIENTED_EDGE ( 'NONE', *, *, #45712, .F. ) ;
#46856 = ORIENTED_EDGE ( 'NONE', *, *, #14821, .T. ) ;
#46857 = ORIENTED_EDGE ( 'NONE', *, *, #28735, .T. ) ;
#46858 = EDGE_CURVE ( 'NONE', #16326, #41579, #37868, .T. ) ;
#46859 = PLANE ( 'NONE',  #31566 ) ;
#46860 = ORIENTED_EDGE ( 'NONE', *, *, #29459, .T. ) ;
#46861 = DIRECTION ( 'NONE',  ( 0.000000000000000000, -0.2334453638558922350, -0.9723699203976797767 ) ) ;
#46862 = FACE_BOUND ( 'NONE', #2772, .T. ) ;
#46863 = ORIENTED_EDGE ( 'NONE', *, *, #21675, .F. ) ;
#46864 = CARTESIAN_POINT ( 'NONE',  ( 0.000000000000000000, -120.0000000000000000, 125.0000000000000000 ) ) ;
#46865 = ORIENTED_EDGE ( 'NONE', *, *, #953, .F. ) ;
#46866 = ADVANCED_FACE ( 'NONE', ( #26846 ), #7271, .T. ) ;
#46867 = ORIENTED_EDGE ( 'NONE', *, *, #23829, .F. ) ;
#46868 = ORIENTED_EDGE ( 'NONE', *, *, #15325, .T. ) ;
#46869 = EDGE_CURVE ( 'NONE', #14988, #15615, #7554, .T. ) ;
#46870 = EDGE_CURVE ( 'NONE', #18356, #3376, #11197, .T. ) ;
#46871 = DIRECTION ( 'NONE',  ( -0.000000000000000000, 0.5877852522924796874, 0.8090169943749426773 ) ) ;
#46872 = DIRECTION ( 'NONE',  ( 0.000000000000000000, 0.3090169943749411785, 0.9510565162951556406 ) ) ;
#46873 = DIRECTION ( 'NONE',  ( -1.000000000000000000, -0.000000000000000000, -0.000000000000000000 ) ) ;
#46874 = AXIS2_PLACEMENT_3D ( 'NONE', #22799, #41645, #15696 ) ;
#46875 = VERTEX_POINT ( 'NONE', #12894 ) ;
#46876 = ORIENTED_EDGE ( 'NONE', *, *, #2877, .F. ) ;
#46877 = AXIS2_PLACEMENT_3D ( 'NONE', #6993, #21917, #33187 ) ;
#46878 = CARTESIAN_POINT ( 'NONE',  ( 10.00000000000000000, 60.67117009219215618, -55.16347631942976193 ) ) ;
#46879 = ORIENTED_EDGE ( 'NONE', *, *, #25502, .T. ) ;
#46880 = CARTESIAN_POINT ( 'NONE',  ( 0.000000000000000000, 0.000000000000000000, 0.000000000000000000 ) ) ;
#46881 = CIRCLE ( 'NONE', #19490, 16.00000000000000000 ) ;
#46882 = DIRECTION ( 'NONE',  ( 0.000000000000000000, 0.000000000000000000, -1.000000000000000000 ) ) ;
#46883 = DIRECTION ( 'NONE',  ( -0.6575728627325955200, 0.7533909544171996098, 1.230411769795008318E-16 ) ) ;
#46884 = DIRECTION ( 'NONE',  ( 0.000000000000000000, 0.000000000000000000, 1.000000000000000000 ) ) ;
#46885 = DIRECTION ( 'NONE',  ( -1.000000000000000000, 0.000000000000000000, -0.000000000000000000 ) ) ;
#46886 = LINE ( 'NONE', #47372, #37718 ) ;
#46887 = CARTESIAN_POINT ( 'NONE',  ( 0.000000000000000000, 59.46389618801964616, 49.70050353004909738 ) ) ;
#46889 = DIRECTION ( 'NONE',  ( -1.000000000000000000, 0.000000000000000000, 0.000000000000000000 ) ) ;
#46888 = PRODUCT_DEFINITION ( 'UNKNOWN', '', #17834, #11018 ) ;
#46890 = DIRECTION ( 'NONE',  ( 0.000000000000000000, 0.7604059656000323741, -0.6494480483301819929 ) ) ;
#46891 = CYLINDRICAL_SURFACE ( 'NONE', #18401, 31.99999999999999289 ) ;
#46892 = VERTEX_POINT ( 'NONE', #31024 ) ;
#46893 = AXIS2_PLACEMENT_3D ( 'NONE', #26759, #1041, #8399 ) ;
#46894 = DIRECTION ( 'NONE',  ( 0.000000000000000000, 0.000000000000000000, 1.000000000000000000 ) ) ;
#46895 = CYLINDRICAL_SURFACE ( 'NONE', #19014, 16.00000000000000000 ) ;
#46896 = CARTESIAN_POINT ( 'NONE',  ( 11.99999999999999822, 75.16055320797030959, 18.89407956138283851 ) ) ;
#46897 = DIRECTION ( 'NONE',  ( -0.000000000000000000, -0.000000000000000000, -1.000000000000000000 ) ) ;
#46898 = DIRECTION ( 'NONE',  ( 0.000000000000000000, 0.000000000000000000, -1.000000000000000000 ) ) ;
#46899 = DIRECTION ( 'NONE',  ( 0.000000000000000000, -0.8660254037844432595, -0.4999999999999920064 ) ) ;
#46900 = ORIENTED_EDGE ( 'NONE', *, *, #40596, .F. ) ;
#46901 = DIRECTION ( 'NONE',  ( -0.8090169943749426773, -0.5877852522924797984, 0.000000000000000000 ) ) ;
#46902 = EDGE_LOOP ( 'NONE', ( #16323, #31184, #33782, #44032 ) ) ;
#46903 = DIRECTION ( 'NONE',  ( 0.1850432970638656582, -0.9827303690289285187, 0.000000000000000000 ) ) ;
#46904 = ORIENTED_EDGE ( 'NONE', *, *, #47611, .F. ) ;
#46905 = VECTOR ( 'NONE', #41592, 1000.000000000000000 ) ;
#46906 = EDGE_CURVE ( 'NONE', #18388, #18579, #38845, .T. ) ;
#46907 = VECTOR ( 'NONE', #13090, 1000.000000000000000 ) ;
#46908 = ORIENTED_EDGE ( 'NONE', *, *, #16239, .F. ) ;
#46910 = EDGE_CURVE ( 'NONE', #21719, #15799, #30242, .T. ) ;
#46909 = AXIS2_PLACEMENT_3D ( 'NONE', #40418, #3925, #30850 ) ;
#46911 = DIRECTION ( 'NONE',  ( 0.000000000000000000, 0.000000000000000000, 1.000000000000000000 ) ) ;
#46912 = ORIENTED_EDGE ( 'NONE', *, *, #17877, .T. ) ;
#46913 = EDGE_CURVE ( 'NONE', #42101, #21999, #27572, .T. ) ;
#46914 = VECTOR ( 'NONE', #22035, 1000.000000000000114 ) ;
#46915 = ORIENTED_EDGE ( 'NONE', *, *, #24109, .F. ) ;
#46916 = AXIS2_PLACEMENT_3D ( 'NONE', #22313, #29155, #3702 ) ;
#46917 = DIRECTION ( 'NONE',  ( -1.000000000000000000, 0.000000000000000000, 0.000000000000000000 ) ) ;
#46919 = ORIENTED_EDGE ( 'NONE', *, *, #37907, .F. ) ;
#46918 = DIRECTION ( 'NONE',  ( -1.000000000000000000, 0.000000000000000000, 0.000000000000000000 ) ) ;
#46920 = VERTEX_POINT ( 'NONE', #27104 ) ;
#46921 = VERTEX_POINT ( 'NONE', #1626 ) ;
#46922 = ORIENTED_EDGE ( 'NONE', *, *, #12757, .T. ) ;
#46923 = ADVANCED_FACE ( 'NONE', ( #35385 ), #8712, .T. ) ;
#46924 = EDGE_CURVE ( 'NONE', #33911, #19660, #44309, .T. ) ;
#46925 = FACE_OUTER_BOUND ( 'NONE', #18280, .T. ) ;
#46927 = ORIENTED_EDGE ( 'NONE', *, *, #17736, .F. ) ;
#46926 = FACE_OUTER_BOUND ( 'NONE', #41530, .T. ) ;
#46928 = LINE ( 'NONE', #43968, #28244 ) ;
#46929 = ORIENTED_EDGE ( 'NONE', *, *, #26034, .F. ) ;
#46930 = ORIENTED_EDGE ( 'NONE', *, *, #31903, .F. ) ;
#46931 = ORIENTED_EDGE ( 'NONE', *, *, #33029, .F. ) ;
#46932 = CYLINDRICAL_SURFACE ( 'NONE', #16897, 31.99999999999998579 ) ;
#46933 = CARTESIAN_POINT ( 'NONE',  ( 0.000000000000000000, -6.736453364083817341, 36.88895765772630142 ) ) ;
#46934 = CYLINDRICAL_SURFACE ( 'NONE', #651, 16.00000000000000000 ) ;
#46935 = CARTESIAN_POINT ( 'NONE',  ( 12.00000000000000000, 8.688484142254226938, 21.88630264137359305 ) ) ;
#46936 = LINE ( 'NONE', #43025, #39362 ) ;
#46937 = FACE_OUTER_BOUND ( 'NONE', #39298, .T. ) ;
#46938 = EDGE_LOOP ( 'NONE', ( #39103, #5746, #29802, #33117 ) ) ;
#46939 = DIRECTION ( 'NONE',  ( -1.000000000000000000, 0.000000000000000000, 0.000000000000000000 ) ) ;
#46940 = EDGE_CURVE ( 'NONE', #26532, #32853, #35640, .T. ) ;
#46941 = CIRCLE ( 'NONE', #32100, 77.49899999999999523 ) ;
#46942 = DIRECTION ( 'NONE',  ( 0.000000000000000000, -0.2334453638558922350, -0.9723699203976797767 ) ) ;
#46943 = ORIENTED_EDGE ( 'NONE', *, *, #7822, .F. ) ;
#46944 = CIRCLE ( 'NONE', #25814, 77.49899999999998101 ) ;
#46945 = DIRECTION ( 'NONE',  ( 1.000000000000000000, -0.000000000000000000, -0.000000000000000000 ) ) ;
#46946 = EDGE_LOOP ( 'NONE', ( #31280, #35774, #16572, #9813 ) ) ;
#46947 = VECTOR ( 'NONE', #34891, 1000.000000000000000 ) ;
#46948 = VECTOR ( 'NONE', #46753, 1000.000000000000000 ) ;
#46949 = FACE_OUTER_BOUND ( 'NONE', #14695, .T. ) ;
#46950 = DIRECTION ( 'NONE',  ( 0.000000000000000000, 0.3090169943749442316, 0.9510565162951545304 ) ) ;
#46951 = LINE ( 'NONE', #28594, #33972 ) ;
#46952 = DIRECTION ( 'NONE',  ( 1.000000000000000000, 0.000000000000000000, 0.000000000000000000 ) ) ;
#46953 = DIRECTION ( 'NONE',  ( 0.000000000000000000, 0.000000000000000000, 1.000000000000000000 ) ) ;
#46954 = AXIS2_PLACEMENT_3D ( 'NONE', #9598, #47060, #6428 ) ;
#46955 = FACE_OUTER_BOUND ( 'NONE', #19760, .T. ) ;
#46956 = ORIENTED_EDGE ( 'NONE', *, *, #33477, .F. ) ;
#46957 = DIRECTION ( 'NONE',  ( 0.000000000000000000, -0.7431448254773871387, 0.6691306063588661202 ) ) ;
#46958 = CIRCLE ( 'NONE', #26618, 16.00000000000000000 ) ;
#46959 = CARTESIAN_POINT ( 'NONE',  ( 0.000000000000000000, 51.02545421589324803, 55.20638768913779870 ) ) ;
#46960 = CARTESIAN_POINT ( 'NONE',  ( -11.59999999999999787, 0.000000000000000000, -44.99999999999998579 ) ) ;
#46961 = DIRECTION ( 'NONE',  ( 0.000000000000000000, 0.000000000000000000, 1.000000000000000000 ) ) ;
#46962 = ORIENTED_EDGE ( 'NONE', *, *, #39230, .T. ) ;
#46963 = ORIENTED_EDGE ( 'NONE', *, *, #35594, .F. ) ;
#46964 = ORIENTED_EDGE ( 'NONE', *, *, #3767, .T. ) ;
#46965 = ORIENTED_EDGE ( 'NONE', *, *, #18827, .T. ) ;
#46966 = EDGE_CURVE ( 'NONE', #34876, #32798, #36504, .T. ) ;
#46967 = DIRECTION ( 'NONE',  ( 0.000000000000000000, 0.000000000000000000, 1.000000000000000000 ) ) ;
#46968 = CARTESIAN_POINT ( 'NONE',  ( 0.000000000000000000, -41.81611651403864727, 3.925862922256025289 ) ) ;
#46969 = ORIENTED_EDGE ( 'NONE', *, *, #35588, .F. ) ;
#46970 = EDGE_CURVE ( 'NONE', #41232, #36602, #47447, .T. ) ;
#46971 = VECTOR ( 'NONE', #39772, 1000.000000000000000 ) ;
#46972 = AXIS2_PLACEMENT_3D ( 'NONE', #40317, #47631, #2849 ) ;
#46973 = EDGE_CURVE ( 'NONE', #10347, #38387, #6062, .T. ) ;
#46974 = DIRECTION ( 'NONE',  ( 0.000000000000000000, -0.9781476007338070211, 0.2079116908177525425 ) ) ;
#46975 = AXIS2_PLACEMENT_3D ( 'NONE', #1554, #46593, #16725 ) ;
#46976 = AXIS2_PLACEMENT_3D ( 'NONE', #29088, #44270, #32294 ) ;
#46977 = ORIENTED_EDGE ( 'NONE', *, *, #31921, .T. ) ;
#46978 = EDGE_LOOP ( 'NONE', ( #26218, #31043, #5113, #46802 ) ) ;
#46979 = EDGE_LOOP ( 'NONE', ( #18298, #15311, #27655, #31606 ) ) ;
#46980 = AXIS2_PLACEMENT_3D ( 'NONE', #29828, #7311, #22497 ) ;
#46981 = ADVANCED_FACE ( 'NONE', ( #5307 ), #8968, .T. ) ;
#46982 = CIRCLE ( 'NONE', #8669, 77.49899999999999523 ) ;
#46983 = DIRECTION ( 'NONE',  ( 0.000000000000000000, 0.9510565162951523099, 0.3090169943749513926 ) ) ;
#46984 = EDGE_LOOP ( 'NONE', ( #18302, #1640, #27042, #25596 ) ) ;
#46985 = DIRECTION ( 'NONE',  ( -1.000000000000000000, -0.000000000000000000, 0.000000000000000000 ) ) ;
#46986 = ADVANCED_FACE ( 'NONE', ( #8482 ), #31498, .T. ) ;
#46987 = ORIENTED_EDGE ( 'NONE', *, *, #40092, .F. ) ;
#46988 = DIRECTION ( 'NONE',  ( -1.000000000000000000, 0.000000000000000000, 0.000000000000000000 ) ) ;
#46989 = CARTESIAN_POINT ( 'NONE',  ( 1.474095553543393056, -119.7224350544041869, -2.500000000000000000 ) ) ;
#46990 = CARTESIAN_POINT ( 'NONE',  ( 0.000000000000000000, -35.47612816024539484, 22.48208911017487921 ) ) ;
#46991 = ORIENTED_EDGE ( 'NONE', *, *, #10947, .T. ) ;
#46992 = DIRECTION ( 'NONE',  ( 0.000000000000000000, 0.000000000000000000, 1.000000000000000000 ) ) ;
#46993 = ORIENTED_EDGE ( 'NONE', *, *, #46966, .T. ) ;
#46994 = FACE_OUTER_BOUND ( 'NONE', #10415, .T. ) ;
#46995 = EDGE_CURVE ( 'NONE', #11808, #27040, #13082, .T. ) ;
#46996 = CARTESIAN_POINT ( 'NONE',  ( 22.63442173698368620, -133.7816164738524378, -2.500000000000000000 ) ) ;
#46997 = VERTEX_POINT ( 'NONE', #24374 ) ;
#46998 = EDGE_LOOP ( 'NONE', ( #30599, #5268, #3869, #34970 ) ) ;
#46999 = CARTESIAN_POINT ( 'NONE',  ( -12.49999999999999645, 0.000000000000000000, -54.99999999999998579 ) ) ;
#47000 = LINE ( 'NONE', #47240, #23081 ) ;
#47001 = EDGE_LOOP ( 'NONE', ( #5218, #36565, #25268, #2358 ) ) ;
#47002 = ORIENTED_EDGE ( 'NONE', *, *, #30409, .F. ) ;
#47003 = DIRECTION ( 'NONE',  ( -1.000000000000000000, 0.000000000000000000, 0.000000000000000000 ) ) ;
#47004 = DIRECTION ( 'NONE',  ( -1.000000000000000000, 0.000000000000000000, 0.000000000000000000 ) ) ;
#47005 = DIRECTION ( 'NONE',  ( 0.000000000000000000, 0.000000000000000000, 1.000000000000000000 ) ) ;
#47006 = DIRECTION ( 'NONE',  ( 0.000000000000000000, 0.000000000000000000, 1.000000000000000000 ) ) ;
#47008 = AXIS2_PLACEMENT_3D ( 'NONE', #16965, #9860, #2986 ) ;
#47007 = CARTESIAN_POINT ( 'NONE',  ( 11.99999999999999822, -17.28742895386031719, -75.54627589209962935 ) ) ;
#47009 = EDGE_CURVE ( 'NONE', #17273, #39718, #5260, .T. ) ;
#47010 = LINE ( 'NONE', #5183, #41143 ) ;
#47011 = LINE ( 'NONE', #35753, #27793 ) ;
#47012 = AXIS2_PLACEMENT_3D ( 'NONE', #38135, #4601, #909 ) ;
#47013 = DIRECTION ( 'NONE',  ( -1.000000000000000000, -0.000000000000000000, -0.000000000000000000 ) ) ;
#47014 = CARTESIAN_POINT ( 'NONE',  ( 10.00000000000000000, 0.000000000000000000, 0.000000000000000000 ) ) ;
#47015 = LINE ( 'NONE', #35987, #32681 ) ;
#47016 = DIRECTION ( 'NONE',  ( -0.9827303690289285187, -0.1850432970638656860, 0.000000000000000000 ) ) ;
#47017 = DIRECTION ( 'NONE',  ( 0.000000000000000000, 0.000000000000000000, 1.000000000000000000 ) ) ;
#47018 = ORIENTED_EDGE ( 'NONE', *, *, #17208, .F. ) ;
#47019 = ORIENTED_EDGE ( 'NONE', *, *, #30077, .F. ) ;
#47020 = DIRECTION ( 'NONE',  ( 0.000000000000000000, 0.000000000000000000, 1.000000000000000000 ) ) ;
#47021 = CIRCLE ( 'NONE', #117, 82.00000000000000000 ) ;
#47022 = EDGE_CURVE ( 'NONE', #23694, #13395, #9932, .T. ) ;
#47023 = DIRECTION ( 'NONE',  ( -1.000000000000000000, 0.000000000000000000, 0.000000000000000000 ) ) ;
#47024 = CIRCLE ( 'NONE', #6390, 77.49899999999999523 ) ;
#47025 = ADVANCED_FACE ( 'NONE', ( #23649 ), #1392, .T. ) ;
#47026 = DIRECTION ( 'NONE',  ( -1.000000000000000000, 0.000000000000000000, 0.000000000000000000 ) ) ;
#47027 = ORIENTED_EDGE ( 'NONE', *, *, #39897, .F. ) ;
#47028 = EDGE_CURVE ( 'NONE', #28487, #2768, #563, .T. ) ;
#47029 = ORIENTED_EDGE ( 'NONE', *, *, #7421, .T. ) ;
#47030 = ADVANCED_FACE ( 'NONE', ( #12647 ), #47129, .F. ) ;
#47031 = DIRECTION ( 'NONE',  ( 0.000000000000000000, 0.000000000000000000, 1.000000000000000000 ) ) ;
#47032 = ORIENTED_EDGE ( 'NONE', *, *, #35768, .F. ) ;
#47033 = DIRECTION ( 'NONE',  ( 0.000000000000000000, 0.000000000000000000, -1.000000000000000000 ) ) ;
#47034 = ORIENTED_EDGE ( 'NONE', *, *, #34301, .F. ) ;
#47035 = LINE ( 'NONE', #5208, #21910 ) ;
#47036 = ORIENTED_EDGE ( 'NONE', *, *, #11509, .T. ) ;
#47037 = AXIS2_PLACEMENT_3D ( 'NONE', #39180, #36410, #43992 ) ;
#47038 = CARTESIAN_POINT ( 'NONE',  ( 0.000000000000000000, -23.29833615347104825, -3.418703333116803744 ) ) ;
#47039 = AXIS2_PLACEMENT_3D ( 'NONE', #42414, #4963, #5450 ) ;
#47040 = CARTESIAN_POINT ( 'NONE',  ( 5.000000000000000000, -22.48208911017525580, 35.47612816024516036 ) ) ;
#47041 = ORIENTED_EDGE ( 'NONE', *, *, #15735, .F. ) ;
#47042 = DIRECTION ( 'NONE',  ( -0.000000000000000000, -0.000000000000000000, -1.000000000000000000 ) ) ;
#47043 = AXIS2_PLACEMENT_3D ( 'NONE', #10570, #29151, #39946 ) ;
#47044 = ORIENTED_EDGE ( 'NONE', *, *, #15862, .F. ) ;
#47045 = EDGE_LOOP ( 'NONE', ( #48309, #32702, #29519, #22958 ) ) ;
#47046 = MECHANICAL_DESIGN_GEOMETRIC_PRESENTATION_REPRESENTATION (  '', ( #26719 ), #11092 ) ;
#47047 = DIRECTION ( 'NONE',  ( 0.000000000000000000, -0.8910065241883721177, 0.4539904997395382003 ) ) ;
#47048 = AXIS2_PLACEMENT_3D ( 'NONE', #16306, #26598, #22913 ) ;
#47049 = DIRECTION ( 'NONE',  ( -1.000000000000000000, 0.000000000000000000, 0.000000000000000000 ) ) ;
#47050 = CARTESIAN_POINT ( 'NONE',  ( -11.99999999999999645, 0.000000000000000000, 0.000000000000000000 ) ) ;
#47051 = CARTESIAN_POINT ( 'NONE',  ( 10.00000000000000000, 78.73519480814954363, 22.90783923731657978 ) ) ;
#47052 = EDGE_CURVE ( 'NONE', #35187, #31605, #36825, .T. ) ;
#47053 = CARTESIAN_POINT ( 'NONE',  ( 0.000000000000000000, 65.58780272294076497, 36.73666225445916211 ) ) ;
#47054 = EDGE_LOOP ( 'NONE', ( #35306, #20314 ) ) ;
#47055 = DIRECTION ( 'NONE',  ( 0.000000000000000000, 0.000000000000000000, 1.000000000000000000 ) ) ;
#47056 = VERTEX_POINT ( 'NONE', #36591 ) ;
#47057 = CARTESIAN_POINT ( 'NONE',  ( 0.000000000000000000, 0.000000000000000000, 0.000000000000000000 ) ) ;
#47058 = VECTOR ( 'NONE', #28630, 1000.000000000000114 ) ;
#47059 = FACE_OUTER_BOUND ( 'NONE', #38378, .T. ) ;
#47060 = DIRECTION ( 'NONE',  ( -1.000000000000000000, 0.000000000000000000, 0.000000000000000000 ) ) ;
#47061 = CARTESIAN_POINT ( 'NONE',  ( 12.00000000000000000, 16.61724383029390140, 20.69703378468902955 ) ) ;
#47062 = VERTEX_POINT ( 'NONE', #32456 ) ;
#47063 = LINE ( 'NONE', #27995, #15185 ) ;
#47064 = DIRECTION ( 'NONE',  ( -1.000000000000000000, 0.000000000000000000, -0.000000000000000000 ) ) ;
#47065 = DIRECTION ( 'NONE',  ( 0.000000000000000000, -0.9510565162951503115, -0.3090169943749573878 ) ) ;
#47066 = FACE_OUTER_BOUND ( 'NONE', #24455, .T. ) ;
#47067 = DIRECTION ( 'NONE',  ( 0.000000000000000000, -0.4999999999999921174, 0.8660254037844431485 ) ) ;
#47068 = DIRECTION ( 'NONE',  ( -1.000000000000000000, -0.000000000000000000, -0.000000000000000000 ) ) ;
#47069 = DIRECTION ( 'NONE',  ( 0.000000000000000000, 0.000000000000000000, 1.000000000000000000 ) ) ;
#47070 = DIRECTION ( 'NONE',  ( 0.000000000000000000, 0.000000000000000000, -1.000000000000000000 ) ) ;
#47071 = FACE_OUTER_BOUND ( 'NONE', #29930, .T. ) ;
#47072 = DIRECTION ( 'NONE',  ( -0.1045284632676570929, 0.9945218953682730678, 0.000000000000000000 ) ) ;
#47073 = DIRECTION ( 'NONE',  ( 1.000000000000000000, 0.000000000000000000, -0.000000000000000000 ) ) ;
#47074 = ORIENTED_EDGE ( 'NONE', *, *, #101, .F. ) ;
#47075 = CIRCLE ( 'NONE', #9531, 82.00000000000000000 ) ;
#47076 = ORIENTED_EDGE ( 'NONE', *, *, #22083, .T. ) ;
#47077 = DIRECTION ( 'NONE',  ( 0.000000000000000000, 0.9876883405951383255, -0.1564344650402277048 ) ) ;
#47078 = ORIENTED_EDGE ( 'NONE', *, *, #38242, .T. ) ;
#47079 = ADVANCED_FACE ( 'NONE', ( #10408 ), #9680, .T. ) ;
#47080 = DIRECTION ( 'NONE',  ( 0.000000000000000000, -0.4539904997395351471, -0.8910065241883737830 ) ) ;
#47081 = AXIS2_PLACEMENT_3D ( 'NONE', #26952, #18624, #15448 ) ;
#47082 = EDGE_CURVE ( 'NONE', #34673, #22551, #27947, .T. ) ;
#47083 = LINE ( 'NONE', #2518, #5729 ) ;
#47084 = CIRCLE ( 'NONE', #43934, 20.64000000000000057 ) ;
#47085 = ORIENTED_EDGE ( 'NONE', *, *, #3543, .T. ) ;
#47086 = ORIENTED_EDGE ( 'NONE', *, *, #7667, .F. ) ;
#47087 = EDGE_CURVE ( 'NONE', #2398, #27438, #10739, .T. ) ;
#47088 = AXIS2_PLACEMENT_3D ( 'NONE', #35649, #20715, #2121 ) ;
#47089 = CARTESIAN_POINT ( 'NONE',  ( 0.000000000000000000, -69.42325613327466272, 34.44570377933573724 ) ) ;
#47091 = EDGE_CURVE ( 'NONE', #19660, #34492, #21175, .T. ) ;
#47090 = ORIENTED_EDGE ( 'NONE', *, *, #7066, .F. ) ;
#47092 = ORIENTED_EDGE ( 'NONE', *, *, #36950, .T. ) ;
#47093 = FACE_OUTER_BOUND ( 'NONE', #15545, .T. ) ;
#47094 = ORIENTED_EDGE ( 'NONE', *, *, #9010, .T. ) ;
#47095 = PLANE ( 'NONE',  #10954 ) ;
#47096 = CARTESIAN_POINT ( 'NONE',  ( 10.00000000000000000, 39.04073710021366139, -15.48615015657542848 ) ) ;
#47097 = ORIENTED_EDGE ( 'NONE', *, *, #19012, .T. ) ;
#47098 = LINE ( 'NONE', #28026, #46132 ) ;
#47099 = VERTEX_POINT ( 'NONE', #17505 ) ;
#47100 = CARTESIAN_POINT ( 'NONE',  ( 50.00005079999999680, 0.000000000000000000, 0.000000000000000000 ) ) ;
#47101 = CARTESIAN_POINT ( 'NONE',  ( 0.000000000000000000, -120.0000000000000000, -2.500000000000000000 ) ) ;
#47102 = CARTESIAN_POINT ( 'NONE',  ( 23.49916127795269460, -121.5130826919798039, -5.500000000000000000 ) ) ;
#47103 = VECTOR ( 'NONE', #2280, 1000.000000000000227 ) ;
#47104 = AXIS2_PLACEMENT_3D ( 'NONE', #8461, #23386, #27318 ) ;
#47105 = VERTEX_POINT ( 'NONE', #13601 ) ;
#47106 = CARTESIAN_POINT ( 'NONE',  ( 16.84844760790522855, -103.5491698323862124, -5.500000000000000000 ) ) ;
#47107 = ORIENTED_EDGE ( 'NONE', *, *, #46366, .T. ) ;
#47108 = CIRCLE ( 'NONE', #13498, 16.00000000000000000 ) ;
#47109 = DIRECTION ( 'NONE',  ( -1.000000000000000000, 0.000000000000000000, 0.000000000000000000 ) ) ;
#47110 = CARTESIAN_POINT ( 'NONE',  ( -0.8815729230226008184, -93.47222532549339746, -5.500000000000000000 ) ) ;
#47111 = LINE ( 'NONE', #47368, #21221 ) ;
#47112 = DIRECTION ( 'NONE',  ( 1.000000000000000000, 0.000000000000000000, 0.000000000000000000 ) ) ;
#47113 = DIRECTION ( 'NONE',  ( -1.000000000000000000, 0.000000000000000000, -0.000000000000000000 ) ) ;
#47114 = CARTESIAN_POINT ( 'NONE',  ( 10.00000000000000000, 0.000000000000000000, 0.000000000000000000 ) ) ;
#47115 = DIRECTION ( 'NONE',  ( 0.000000000000000000, 0.000000000000000000, -1.000000000000000000 ) ) ;
#47116 = FACE_OUTER_BOUND ( 'NONE', #38368, .T. ) ;
#47117 = CARTESIAN_POINT ( 'NONE',  ( 5.000000000000000000, 27.75498641678742473, 31.52238457039609187 ) ) ;
#47118 = DIRECTION ( 'NONE',  ( -1.000000000000000000, -0.000000000000000000, -0.000000000000000000 ) ) ;
#47119 = EDGE_CURVE ( 'NONE', #36392, #36384, #29494, .T. ) ;
#47120 = ORIENTED_EDGE ( 'NONE', *, *, #21698, .F. ) ;
#47121 = VECTOR ( 'NONE', #23390, 1000.000000000000000 ) ;
#47122 = CARTESIAN_POINT ( 'NONE',  ( 10.00000000000000000, -39.04073710021333454, -15.48615015657624738 ) ) ;
#47123 = AXIS2_PLACEMENT_3D ( 'NONE', #23848, #31206, #19206 ) ;
#47124 = EDGE_CURVE ( 'NONE', #33083, #9793, #6979, .T. ) ;
#47125 = DIRECTION ( 'NONE',  ( -1.000000000000000000, 0.000000000000000000, 0.000000000000000000 ) ) ;
#47126 = CARTESIAN_POINT ( 'NONE',  ( -42.50000000000000000, 1.932465207890948911E-15, 15.77977592589476608 ) ) ;
#47127 = EDGE_CURVE ( 'NONE', #11149, #5341, #21896, .T. ) ;
#47128 = DIRECTION ( 'NONE',  ( 0.000000000000000000, 0.000000000000000000, 1.000000000000000000 ) ) ;
#47129 = PLANE ( 'NONE',  #34938 ) ;
#47130 = FACE_OUTER_BOUND ( 'NONE', #46946, .T. ) ;
#47131 = ORIENTED_EDGE ( 'NONE', *, *, #22210, .F. ) ;
#47132 = CARTESIAN_POINT ( 'NONE',  ( 12.00000000000000000, 16.83928648764922542, -16.46020748918050458 ) ) ;
#47133 = ORIENTED_EDGE ( 'NONE', *, *, #43406, .T. ) ;
#47134 = CIRCLE ( 'NONE', #15108, 31.99999999999999645 ) ;
#47135 = ADVANCED_FACE ( 'NONE', ( #28541 ), #43476, .T. ) ;
#47136 = CYLINDRICAL_SURFACE ( 'NONE', #13476, 31.99999999999999289 ) ;
#47137 = EDGE_CURVE ( 'NONE', #33199, #13081, #13857, .T. ) ;
#47138 = EDGE_CURVE ( 'NONE', #35412, #42832, #31049, .T. ) ;
#47139 = ORIENTED_EDGE ( 'NONE', *, *, #28175, .F. ) ;
#47140 = AXIS2_PLACEMENT_3D ( 'NONE', #13244, #35754, #32092 ) ;
#47141 = ORIENTED_EDGE ( 'NONE', *, *, #42944, .T. ) ;
#47142 = AXIS2_PLACEMENT_3D ( 'NONE', #10205, #21708, #43743 ) ;
#47143 = AXIS2_PLACEMENT_3D ( 'NONE', #34698, #1180, #18853 ) ;
#47144 = AXIS2_PLACEMENT_3D ( 'NONE', #11193, #3604, #29064 ) ;
#47145 = EDGE_CURVE ( 'NONE', #43074, #11482, #34172, .T. ) ;
#47146 = DIRECTION ( 'NONE',  ( -1.000000000000000000, 0.000000000000000000, 0.000000000000000000 ) ) ;
#47147 = EDGE_LOOP ( 'NONE', ( #36215, #4689, #6937, #3878 ) ) ;
#47148 = VECTOR ( 'NONE', #12953, 1000.000000000000000 ) ;
#47149 = ORIENTED_EDGE ( 'NONE', *, *, #5196, .F. ) ;
#47150 = AXIS2_PLACEMENT_3D ( 'NONE', #41466, #12105, #7921 ) ;
#47151 = CYLINDRICAL_SURFACE ( 'NONE', #43721, 31.99999999999998579 ) ;
#47152 = AXIS2_PLACEMENT_3D ( 'NONE', #38739, #46796, #5200 ) ;
#47154 = ORIENTED_EDGE ( 'NONE', *, *, #24364, .T. ) ;
#47153 = CARTESIAN_POINT ( 'NONE',  ( 0.000000000000000000, -22.74946021919110706, -29.81001611431033282 ) ) ;
#47155 = EDGE_CURVE ( 'NONE', #45830, #42640, #21420, .T. ) ;
#47156 = ORIENTED_EDGE ( 'NONE', *, *, #2013, .T. ) ;
#47157 = EDGE_LOOP ( 'NONE', ( #20234, #6595, #35585, #12304 ) ) ;
#47158 = VERTEX_POINT ( 'NONE', #29002 ) ;
#47159 = CIRCLE ( 'NONE', #17454, 32.00000000000000000 ) ;
#47160 = FACE_OUTER_BOUND ( 'NONE', #42887, .T. ) ;
#47162 = ORIENTED_EDGE ( 'NONE', *, *, #14697, .T. ) ;
#47161 = FACE_OUTER_BOUND ( 'NONE', #20888, .T. ) ;
#47163 = LINE ( 'NONE', #13634, #22795 ) ;
#47164 = ORIENTED_EDGE ( 'NONE', *, *, #23607, .F. ) ;
#47165 = ORIENTED_EDGE ( 'NONE', *, *, #47087, .T. ) ;
#47166 = FACE_OUTER_BOUND ( 'NONE', #39561, .T. ) ;
#47167 = ORIENTED_EDGE ( 'NONE', *, *, #24201, .F. ) ;
#47168 = FACE_OUTER_BOUND ( 'NONE', #38881, .T. ) ;
#47169 = CARTESIAN_POINT ( 'NONE',  ( 5.000000000000002665, -80.55351364060578589, -15.33399622253568673 ) ) ;
#47170 = FACE_BOUND ( 'NONE', #13484, .T. ) ;
#47171 = CYLINDRICAL_SURFACE ( 'NONE', #37005, 15.77977592589476608 ) ;
#47172 = CARTESIAN_POINT ( 'NONE',  ( -10.00000000000000000, 0.000000000000000000, 0.000000000000000000 ) ) ;
#47173 = CIRCLE ( 'NONE', #19030, 31.99999999999998579 ) ;
#47174 = CARTESIAN_POINT ( 'NONE',  ( 0.000000000000000000, 73.73191006444572793, -14.66109333815486515 ) ) ;
#47175 = CARTESIAN_POINT ( 'NONE',  ( 10.00000000000000000, -4.992566952384716927, -37.16516213103282951 ) ) ;
#47176 = ADVANCED_FACE ( 'NONE', ( #24855 ), #27165, .T. ) ;
#47177 = ORIENTED_EDGE ( 'NONE', *, *, #17886, .T. ) ;
#47178 = CARTESIAN_POINT ( 'NONE',  ( 11.99999999999999822, -28.89263327155693517, -71.91182617369219088 ) ) ;
#47179 = ORIENTED_EDGE ( 'NONE', *, *, #41408, .T. ) ;
#47180 = AXIS2_PLACEMENT_3D ( 'NONE', #47821, #42973, #9421 ) ;
#47181 = CIRCLE ( 'NONE', #21382, 82.00000000000000000 ) ;
#47182 = CIRCLE ( 'NONE', #41697, 77.49899999999998101 ) ;
#47183 = EDGE_CURVE ( 'NONE', #1839, #35935, #2820, .T. ) ;
#47184 = FACE_OUTER_BOUND ( 'NONE', #32373, .T. ) ;
#47185 = CARTESIAN_POINT ( 'NONE',  ( 11.99999999999999822, 51.02545421589324803, 55.20638768913779870 ) ) ;
#47186 = CYLINDRICAL_SURFACE ( 'NONE', #41790, 16.00000000000000000 ) ;
#47187 = CARTESIAN_POINT ( 'NONE',  ( 10.00000000000000000, -0.6853352020793173072, 37.58145647212453611 ) ) ;
#47188 = EDGE_CURVE ( 'NONE', #2793, #13936, #17752, .T. ) ;
#47189 = CARTESIAN_POINT ( 'NONE',  ( 10.00000000000000000, 35.92658777277525672, -10.74501242461245809 ) ) ;
#47190 = ORIENTED_EDGE ( 'NONE', *, *, #29058, .F. ) ;
#47191 = CIRCLE ( 'NONE', #22939, 77.49899999999999523 ) ;
#47192 = AXIS2_PLACEMENT_3D ( 'NONE', #32907, #14577, #18475 ) ;
#47193 = CARTESIAN_POINT ( 'NONE',  ( -13.05994868825747446, -139.5943292883446532, 2.500000000000000000 ) ) ;
#47194 = CARTESIAN_POINT ( 'NONE',  ( 4.999999999999999112, -9.188173127307004862, -40.98264845739759465 ) ) ;
#47195 = DIRECTION ( 'NONE',  ( 0.000000000000000000, 0.2334453638559058908, -0.9723699203976764460 ) ) ;
#47196 = ORIENTED_EDGE ( 'NONE', *, *, #7800, .F. ) ;
#47197 = VECTOR ( 'NONE', #31611, 1000.000000000000000 ) ;
#47198 = VECTOR ( 'NONE', #24208, 1000.000000000000114 ) ;
#47199 = DIRECTION ( 'NONE',  ( -1.000000000000000000, 0.000000000000000000, 0.000000000000000000 ) ) ;
#47200 = SURFACE_SIDE_STYLE ('',( #9269 ) ) ;
#47201 = CIRCLE ( 'NONE', #1898, 77.49899999999999523 ) ;
#47202 = EDGE_CURVE ( 'NONE', #37915, #5067, #7591, .T. ) ;
#47203 = ADVANCED_FACE ( 'NONE', ( #10895 ), #14579, .T. ) ;
#47204 = ORIENTED_EDGE ( 'NONE', *, *, #21900, .T. ) ;
#47205 = EDGE_LOOP ( 'NONE', ( #20718, #42546, #35012, #36721 ) ) ;
#47206 = CARTESIAN_POINT ( 'NONE',  ( 10.00000000000000000, 0.000000000000000000, 0.000000000000000000 ) ) ;
#47207 = CYLINDRICAL_SURFACE ( 'NONE', #45696, 16.00000000000000000 ) ;
#47208 = VERTEX_POINT ( 'NONE', #30230 ) ;
#47209 = AXIS2_PLACEMENT_3D ( 'NONE', #18042, #44250, #10725 ) ;
#47210 = EDGE_CURVE ( 'NONE', #16837, #42551, #29496, .T. ) ;
#47211 = AXIS2_PLACEMENT_3D ( 'NONE', #24789, #21094, #27990 ) ;
#47212 = CARTESIAN_POINT ( 'NONE',  ( 0.000000000000000000, 0.000000000000000000, 0.000000000000000000 ) ) ;
#47213 = VECTOR ( 'NONE', #35569, 1000.000000000000114 ) ;
#47214 = CIRCLE ( 'NONE', #26116, 42.00000000000000000 ) ;
#47215 = AXIS2_PLACEMENT_3D ( 'NONE', #601, #355, #16022 ) ;
#47216 = ORIENTED_EDGE ( 'NONE', *, *, #4763, .F. ) ;
#47217 = ORIENTED_EDGE ( 'NONE', *, *, #20053, .F. ) ;
#47218 = ORIENTED_EDGE ( 'NONE', *, *, #41018, .F. ) ;
#47219 = PRODUCT ( 'output shaft', 'output shaft', '', ( #30650 ) ) ;
#47220 = CARTESIAN_POINT ( 'NONE',  ( 32.50000000000000000, -120.0000000000000000, 102.9091629284897493 ) ) ;
#47221 = AXIS2_PLACEMENT_3D ( 'NONE', #35162, #38366, #18843 ) ;
#47222 = VECTOR ( 'NONE', #43879, 1000.000000000000000 ) ;
#47223 = VERTEX_POINT ( 'NONE', #4290 ) ;
#47224 = CARTESIAN_POINT ( 'NONE',  ( 0.000000000000000000, -41.81611651403859042, -3.925862922256606602 ) ) ;
#47225 = ORIENTED_EDGE ( 'NONE', *, *, #45312, .T. ) ;
#47226 = AXIS2_PLACEMENT_3D ( 'NONE', #4866, #936, #15884 ) ;
#47227 = CARTESIAN_POINT ( 'NONE',  ( 11.99999999999999822, 40.65526001592611749, 71.21200624218811015 ) ) ;
#47228 = AXIS2_PLACEMENT_3D ( 'NONE', #177, #26621, #41552 ) ;
#47229 = CARTESIAN_POINT ( 'NONE',  ( 0.000000000000000000, -10.45096189432344147, 21.10159698893426494 ) ) ;
#47230 = CARTESIAN_POINT ( 'NONE',  ( 5.999999999999999112, -55.16347631943085617, 60.67117009219117563 ) ) ;
#47232 = ORIENTED_EDGE ( 'NONE', *, *, #11556, .T. ) ;
#47231 = VECTOR ( 'NONE', #151, 1000.000000000000000 ) ;
#47233 = CARTESIAN_POINT ( 'NONE',  ( 11.99999999999999822, -6.903761155838323837, 77.19088730480521576 ) ) ;
#47234 = ORIENTED_EDGE ( 'NONE', *, *, #10271, .T. ) ;
#47235 = DIRECTION ( 'NONE',  ( 0.000000000000000000, 0.000000000000000000, 1.000000000000000000 ) ) ;
#47236 = DIRECTION ( 'NONE',  ( -1.000000000000000000, 0.000000000000000000, 0.000000000000000000 ) ) ;
#47237 = VERTEX_POINT ( 'NONE', #15053 ) ;
#47238 = VERTEX_POINT ( 'NONE', #19201 ) ;
#47239 = DIRECTION ( 'NONE',  ( -1.000000000000000000, -0.000000000000000000, -0.000000000000000000 ) ) ;
#47240 = CARTESIAN_POINT ( 'NONE',  ( 11.99999999999999822, 76.41127070299273782, 12.93880638057342836 ) ) ;
#47241 = ORIENTED_EDGE ( 'NONE', *, *, #29576, .F. ) ;
#47242 = ADVANCED_FACE ( 'NONE', ( #45380 ), #41720, .T. ) ;
#47243 = CARTESIAN_POINT ( 'NONE',  ( 0.000000000000000000, 50.95692526931414790, -58.39081064771693974 ) ) ;
#47244 = CARTESIAN_POINT ( 'NONE',  ( 0.000000000000000000, 6.555932627142418312, 37.01155633439060466 ) ) ;
#47245 = CARTESIAN_POINT ( 'NONE',  ( 0.000000000000000000, -3.925862922255855647, -41.81611651403866858 ) ) ;
#47247 = VERTEX_POINT ( 'NONE', #37325 ) ;
#47246 = CIRCLE ( 'NONE', #22227, 77.49899999999999523 ) ;
#47248 = CARTESIAN_POINT ( 'NONE',  ( 10.00000000000000000, -14.66109333815513160, 73.73191006444567108 ) ) ;
#47249 = EDGE_CURVE ( 'NONE', #41560, #747, #16984, .T. ) ;
#47250 = DIRECTION ( 'NONE',  ( 0.000000000000000000, 0.000000000000000000, 1.000000000000000000 ) ) ;
#47251 = VERTEX_POINT ( 'NONE', #22867 ) ;
#47252 = AXIS2_PLACEMENT_3D ( 'NONE', #10268, #47478, #39677 ) ;
#47253 = DIRECTION ( 'NONE',  ( 0.000000000000000000, 0.000000000000000000, 1.000000000000000000 ) ) ;
#47254 = DIRECTION ( 'NONE',  ( -1.000000000000000000, 0.000000000000000000, 0.000000000000000000 ) ) ;
#47255 = AXIS2_PLACEMENT_3D ( 'NONE', #20685, #39050, #13839 ) ;
#47256 = CARTESIAN_POINT ( 'NONE',  ( 11.99999999999999822, -14.66109333815513160, 73.73191006444567108 ) ) ;
#47258 = CIRCLE ( 'NONE', #22123, 82.00000000000000000 ) ;
#47257 = DIRECTION ( 'NONE',  ( 0.000000000000000000, 0.000000000000000000, 1.000000000000000000 ) ) ;
#47259 = CARTESIAN_POINT ( 'NONE',  ( 5.000000000000002665, 10.30890764327382847, 81.34940948281339956 ) ) ;
#47260 = CYLINDRICAL_SURFACE ( 'NONE', #32731, 82.00000000000000000 ) ;
#47261 = DIRECTION ( 'NONE',  ( 0.000000000000000000, -0.2079116908177554846, 0.9781476007338064660 ) ) ;
#47262 = ORIENTED_EDGE ( 'NONE', *, *, #35874, .T. ) ;
#47263 = EDGE_CURVE ( 'NONE', #6273, #30039, #27127, .T. ) ;
#47264 = ADVANCED_FACE ( 'NONE', ( #3785 ), #48331, .F. ) ;
#47265 = ORIENTED_EDGE ( 'NONE', *, *, #12577, .T. ) ;
#47266 = CIRCLE ( 'NONE', #41786, 16.00000000000000355 ) ;
#47267 = AXIS2_PLACEMENT_3D ( 'NONE', #45555, #34537, #30898 ) ;
#47268 = EDGE_CURVE ( 'NONE', #7063, #22787, #7699, .T. ) ;
#47269 = AXIS2_PLACEMENT_3D ( 'NONE', #25384, #33932, #22455 ) ;
#47270 = CARTESIAN_POINT ( 'NONE',  ( 0.000000000000000000, 26.50000000000000000, -1.500000000000001332 ) ) ;
#47271 = AXIS2_PLACEMENT_3D ( 'NONE', #35595, #32167, #24094 ) ;
#47272 = AXIS2_PLACEMENT_3D ( 'NONE', #43337, #21043, #39899 ) ;
#47273 = CARTESIAN_POINT ( 'NONE',  ( 11.99999999999999822, 0.000000000000000000, 0.000000000000000000 ) ) ;
#47274 = VECTOR ( 'NONE', #10701, 1000.000000000000114 ) ;
#47275 = ORIENTED_EDGE ( 'NONE', *, *, #41435, .T. ) ;
#47276 = ADVANCED_FACE ( 'NONE', ( #19423 ), #3547, .T. ) ;
#47277 = LINE ( 'NONE', #30715, #5474 ) ;
#47278 = CARTESIAN_POINT ( 'NONE',  ( 0.000000000000000000, 37.48860685352291000, 0.8828120875901893649 ) ) ;
#47279 = ORIENTED_EDGE ( 'NONE', *, *, #11543, .F. ) ;
#47280 = DIRECTION ( 'NONE',  ( -1.000000000000000000, -0.000000000000000000, 0.000000000000000000 ) ) ;
#47281 = CIRCLE ( 'NONE', #6644, 15.99999999999999645 ) ;
#47282 = ORIENTED_EDGE ( 'NONE', *, *, #24262, .T. ) ;
#47283 = LINE ( 'NONE', #40647, #14396 ) ;
#47284 = DIRECTION ( 'NONE',  ( 0.9435911131814395114, -0.3311129884571304971, 0.000000000000000000 ) ) ;
#47285 = VECTOR ( 'NONE', #4975, 1000.000000000000000 ) ;
#47286 = CARTESIAN_POINT ( 'NONE',  ( 11.99999999999999822, 75.54627589209944460, 17.28742895386110945 ) ) ;
#47287 = ORIENTED_EDGE ( 'NONE', *, *, #47482, .T. ) ;
#47288 = CARTESIAN_POINT ( 'NONE',  ( 4.999999999999999112, -38.55633173627022359, 16.65560815589396526 ) ) ;
#47289 = ORIENTED_EDGE ( 'NONE', *, *, #24103, .T. ) ;
#47290 = FACE_OUTER_BOUND ( 'NONE', #4439, .T. ) ;
#47291 = CARTESIAN_POINT ( 'NONE',  ( 0.000000000000000000, 37.58145647212453611, 0.6853352020791767529 ) ) ;
#47293 = VERTEX_POINT ( 'NONE', #7932 ) ;
#47292 = CARTESIAN_POINT ( 'NONE',  ( 11.99999999999999822, -30.41916302227062019, -71.27951684758059514 ) ) ;
#47294 = DIRECTION ( 'NONE',  ( 0.000000000000000000, 0.000000000000000000, 1.000000000000000000 ) ) ;
#47295 = AXIS2_PLACEMENT_3D ( 'NONE', #10627, #22362, #2783 ) ;
#47296 = CIRCLE ( 'NONE', #22281, 37.49900000000000233 ) ;
#47297 = ORIENTED_EDGE ( 'NONE', *, *, #44156, .T. ) ;
#47298 = CARTESIAN_POINT ( 'NONE',  ( 10.00000000000000000, 0.000000000000000000, 0.000000000000000000 ) ) ;
#47299 = ORIENTED_EDGE ( 'NONE', *, *, #7520, .F. ) ;
#47300 = ORIENTED_EDGE ( 'NONE', *, *, #10743, .F. ) ;
#47301 = ADVANCED_FACE ( 'NONE', ( #37804 ), #26061, .T. ) ;
#47302 = CARTESIAN_POINT ( 'NONE',  ( 10.00000000000000000, 74.65374052328660071, -8.840884882374309583 ) ) ;
#47303 = ORIENTED_EDGE ( 'NONE', *, *, #17449, .F. ) ;
#47304 = EDGE_CURVE ( 'NONE', #19294, #15803, #27194, .T. ) ;
#47305 = CARTESIAN_POINT ( 'NONE',  ( 10.00000000000000000, 10.74501242461333028, -35.92658777277499382 ) ) ;
#47306 = VECTOR ( 'NONE', #19708, 1000.000000000000000 ) ;
#47307 = CARTESIAN_POINT ( 'NONE',  ( 15.00000000000000000, 23.49999999999999645, -1.500000000000003997 ) ) ;
#47308 = DIRECTION ( 'NONE',  ( -1.000000000000000000, -0.000000000000000000, -0.000000000000000000 ) ) ;
#47309 = ORIENTED_EDGE ( 'NONE', *, *, #37685, .F. ) ;
#47310 = DIRECTION ( 'NONE',  ( -0.000000000000000000, -0.000000000000000000, -1.000000000000000000 ) ) ;
#47311 = EDGE_CURVE ( 'NONE', #41579, #23140, #6855, .T. ) ;
#47312 = AXIS2_PLACEMENT_3D ( 'NONE', #11175, #34630, #42478 ) ;
#47313 = FACE_OUTER_BOUND ( 'NONE', #45478, .T. ) ;
#47314 = EDGE_CURVE ( 'NONE', #38352, #23243, #45928, .T. ) ;
#47315 = AXIS2_PLACEMENT_3D ( 'NONE', #33065, #22308, #14958 ) ;
#47316 = CARTESIAN_POINT ( 'NONE',  ( 2.117611129180199558, -93.54218975225703048, 2.500000000000000000 ) ) ;
#47317 = CARTESIAN_POINT ( 'NONE',  ( 10.00000000000000000, 0.000000000000000000, 0.000000000000000000 ) ) ;
#47318 = DIRECTION ( 'NONE',  ( -1.000000000000000000, 0.000000000000000000, 0.000000000000000000 ) ) ;
#47320 = EDGE_CURVE ( 'NONE', #4369, #20259, #29730, .T. ) ;
#47319 = DIRECTION ( 'NONE',  ( 1.000000000000000000, 0.000000000000000000, -0.000000000000000000 ) ) ;
#47321 = LINE ( 'NONE', #36531, #19308 ) ;
#47322 = FACE_OUTER_BOUND ( 'NONE', #45391, .T. ) ;
#47323 = AXIS2_PLACEMENT_3D ( 'NONE', #11010, #7815, #22742 ) ;
#47324 = DIRECTION ( 'NONE',  ( -1.000000000000000000, -0.000000000000000000, -0.000000000000000000 ) ) ;
#47325 = CARTESIAN_POINT ( 'NONE',  ( 5.000000000000002665, -71.87247863392386193, -39.47590169984923136 ) ) ;
#47326 = ORIENTED_EDGE ( 'NONE', *, *, #6239, .T. ) ;
#47327 = FACE_OUTER_BOUND ( 'NONE', #36708, .T. ) ;
#47328 = VERTEX_POINT ( 'NONE', #45156 ) ;
#47329 = EDGE_CURVE ( 'NONE', #8466, #43027, #11623, .T. ) ;
#47330 = CYLINDRICAL_SURFACE ( 'NONE', #5706, 31.99999999999998579 ) ;
#47331 = CARTESIAN_POINT ( 'NONE',  ( 10.00000000000000000, -76.69515212745996280, -29.01471420065644580 ) ) ;
#47332 = ORIENTED_EDGE ( 'NONE', *, *, #36306, .T. ) ;
#47333 = EDGE_LOOP ( 'NONE', ( #5686, #34558, #16894, #34195 ) ) ;
#47334 = ADVANCED_FACE ( 'NONE', ( #7470 ), #26312, .T. ) ;
#47335 = CIRCLE ( 'NONE', #20742, 31.99999999999998579 ) ;
#47336 = VECTOR ( 'NONE', #7473, 1000.000000000000000 ) ;
#47337 = DIRECTION ( 'NONE',  ( -1.000000000000000000, -0.000000000000000000, -0.000000000000000000 ) ) ;
#47338 = CIRCLE ( 'NONE', #5135, 42.00000000000000000 ) ;
#47340 = ORIENTED_EDGE ( 'NONE', *, *, #2640, .T. ) ;
#47339 = ADVANCED_BREP_SHAPE_REPRESENTATION ( '', ( #19421, #11636 ), #10062 ) ;
#47341 = ADVANCED_FACE ( 'NONE', ( #12120 ), #43106, .T. ) ;
#47342 = ORIENTED_EDGE ( 'NONE', *, *, #39145, .T. ) ;
#47343 = AXIS2_PLACEMENT_3D ( 'NONE', #47057, #32376, #13522 ) ;
#47344 = CIRCLE ( 'NONE', #27010, 42.00000000000000000 ) ;
#47345 = EDGE_CURVE ( 'NONE', #28702, #27047, #6101, .T. ) ;
#47346 = AXIS2_PLACEMENT_3D ( 'NONE', #21834, #9867, #6437 ) ;
#47347 = DIRECTION ( 'NONE',  ( -1.000000000000000000, 0.000000000000000000, 0.000000000000000000 ) ) ;
#47348 = ORIENTED_EDGE ( 'NONE', *, *, #28393, .F. ) ;
#47349 = DIRECTION ( 'NONE',  ( -1.000000000000000000, 0.000000000000000000, -0.000000000000000000 ) ) ;
#47350 = DIRECTION ( 'NONE',  ( -1.000000000000000000, -0.000000000000000000, -0.000000000000000000 ) ) ;
#47351 = VERTEX_POINT ( 'NONE', #39195 ) ;
#47352 = CARTESIAN_POINT ( 'NONE',  ( 5.999999999999999112, -77.16300072079641836, -27.74655509720751922 ) ) ;
#47353 = ORIENTED_EDGE ( 'NONE', *, *, #27356, .T. ) ;
#47354 = AXIS2_PLACEMENT_3D ( 'NONE', #48093, #10894, #44182 ) ;
#47355 = EDGE_LOOP ( 'NONE', ( #17773, #6776, #19090, #17578 ) ) ;
#47356 = CARTESIAN_POINT ( 'NONE',  ( 0.000000000000000000, -40.98264845739743123, -9.188173127307734944 ) ) ;
#47357 = FACE_OUTER_BOUND ( 'NONE', #36326, .T. ) ;
#47358 = CARTESIAN_POINT ( 'NONE',  ( 0.000000000000000000, -36.73666225445845157, -65.58780272294114866 ) ) ;
#47359 = ADVANCED_FACE ( 'NONE', ( #32331 ), #41976, .F. ) ;
#47360 = VECTOR ( 'NONE', #1504, 1000.000000000000000 ) ;
#47361 = VERTEX_POINT ( 'NONE', #5664 ) ;
#47362 = FACE_OUTER_BOUND ( 'NONE', #17496, .T. ) ;
#47363 = EDGE_LOOP ( 'NONE', ( #41043, #30439, #47654, #10358 ) ) ;
#47364 = ORIENTED_EDGE ( 'NONE', *, *, #14198, .F. ) ;
#47365 = EDGE_CURVE ( 'NONE', #16326, #47293, #26391, .T. ) ;
#47366 = DIRECTION ( 'NONE',  ( 0.000000000000000000, 0.000000000000000000, -1.000000000000000000 ) ) ;
#47367 = CARTESIAN_POINT ( 'NONE',  ( 0.000000000000000000, 16.00000000000000000, -2.500000000000000000 ) ) ;
#47368 = CARTESIAN_POINT ( 'NONE',  ( 4.999999999999999112, -21.40280677340345505, -36.13751322684441192 ) ) ;
#47369 = DIRECTION ( 'NONE',  ( 1.000000000000000000, 0.000000000000000000, 0.000000000000000000 ) ) ;
#47370 = ADVANCED_FACE ( 'NONE', ( #23351 ), #12354, .T. ) ;
#47371 = CARTESIAN_POINT ( 'NONE',  ( 11.99999999999999822, -41.19522573413780009, 65.64334221924896440 ) ) ;
#47372 = CARTESIAN_POINT ( 'NONE',  ( 10.00000000000000000, -10.74501242461308159, 35.92658777277507909 ) ) ;
#47373 = DIRECTION ( 'NONE',  ( -1.000000000000000000, 0.000000000000000000, 0.000000000000000000 ) ) ;
#47374 = DIRECTION ( 'NONE',  ( -1.000000000000000000, -0.000000000000000000, -0.000000000000000000 ) ) ;
#47375 = LINE ( 'NONE', #32203, #47835 ) ;
#47376 = CARTESIAN_POINT ( 'NONE',  ( 10.00000000000000000, 16.23288003029543347, -33.80338159004267595 ) ) ;
#47377 = VECTOR ( 'NONE', #20799, 1000.000000000000000 ) ;
#47378 = ORIENTED_EDGE ( 'NONE', *, *, #924, .F. ) ;
#47380 = ADVANCED_FACE ( 'NONE', ( #19663 ), #17148, .T. ) ;
#47379 = CARTESIAN_POINT ( 'NONE',  ( 11.99999999999999822, -74.65491531819124305, 8.830959090342128448 ) ) ;
#47381 = AXIS2_PLACEMENT_3D ( 'NONE', #42185, #23836, #4743 ) ;
#47382 = CARTESIAN_POINT ( 'NONE',  ( 10.00000000000000000, -75.11764819372145041, -2.946379043147127064 ) ) ;
#47383 = CARTESIAN_POINT ( 'NONE',  ( 10.00000000000000000, 65.59268652807210742, 36.72794159290264560 ) ) ;
#47384 = DIRECTION ( 'NONE',  ( -0.000000000000000000, -0.000000000000000000, -1.000000000000000000 ) ) ;
#47385 = DIRECTION ( 'NONE',  ( -1.000000000000000000, 0.000000000000000000, 0.000000000000000000 ) ) ;
#47386 = DIRECTION ( 'NONE',  ( -1.000000000000000000, -0.000000000000000000, -0.000000000000000000 ) ) ;
#47387 = AXIS2_PLACEMENT_3D ( 'NONE', #3787, #8187, #37806 ) ;
#47388 = EDGE_LOOP ( 'NONE', ( #21093, #29514, #14789, #30326 ) ) ;
#47389 = CARTESIAN_POINT ( 'NONE',  ( 5.000000000000000000, 2.543863470248396208, 81.96053171279903893 ) ) ;
#47390 = AXIS2_PLACEMENT_3D ( 'NONE', #518, #259, #11301 ) ;
#47391 = DIRECTION ( 'NONE',  ( -1.000000000000000000, 0.000000000000000000, 0.000000000000000000 ) ) ;
#47392 = VERTEX_POINT ( 'NONE', #1075 ) ;
#47393 = ORIENTED_EDGE ( 'NONE', *, *, #15985, .F. ) ;
#47394 = AXIS2_PLACEMENT_3D ( 'NONE', #15416, #4872, #30345 ) ;
#47395 = EDGE_LOOP ( 'NONE', ( #27795, #6945, #33191, #13132 ) ) ;
#47396 = DIRECTION ( 'NONE',  ( -1.000000000000000000, -0.000000000000000000, -0.000000000000000000 ) ) ;
#47397 = ORIENTED_EDGE ( 'NONE', *, *, #14426, .F. ) ;
#47398 = ORIENTED_EDGE ( 'NONE', *, *, #46995, .F. ) ;
#47399 = AXIS2_PLACEMENT_3D ( 'NONE', #45970, #46700, #35901 ) ;
#47400 = CARTESIAN_POINT ( 'NONE',  ( -3.000000000000000000, 23.50000000000000000, 1.499999999999997780 ) ) ;
#47401 = CARTESIAN_POINT ( 'NONE',  ( -10.00000000000000000, 0.000000000000000000, 0.000000000000000000 ) ) ;
#47402 = ORIENTED_EDGE ( 'NONE', *, *, #18272, .F. ) ;
#47403 = AXIS2_PLACEMENT_3D ( 'NONE', #35020, #19587, #42372 ) ;
#47404 = ORIENTED_EDGE ( 'NONE', *, *, #27703, .F. ) ;
#47405 = DIRECTION ( 'NONE',  ( -1.000000000000000000, 0.000000000000000000, 0.000000000000000000 ) ) ;
#47406 = CARTESIAN_POINT ( 'NONE',  ( -10.00000000000000000, 0.000000000000000000, 0.000000000000000000 ) ) ;
#47407 = CARTESIAN_POINT ( 'NONE',  ( 10.00000000000000000, -41.76106447765533147, 62.50884508063410294 ) ) ;
#47408 = ORIENTED_EDGE ( 'NONE', *, *, #39456, .F. ) ;
#47409 = AXIS2_PLACEMENT_3D ( 'NONE', #2384, #24676, #20763 ) ;
#47410 = VERTEX_POINT ( 'NONE', #21060 ) ;
#47411 = CARTESIAN_POINT ( 'NONE',  ( -3.000000000000000000, -22.32062822937489344, 14.36278369418800160 ) ) ;
#47412 = ORIENTED_EDGE ( 'NONE', *, *, #39640, .T. ) ;
#47413 = CARTESIAN_POINT ( 'NONE',  ( 11.99999999999999822, -44.99326035066103202, 68.55367621811127776 ) ) ;
#47414 = FACE_BOUND ( 'NONE', #24792, .T. ) ;
#47415 = CARTESIAN_POINT ( 'NONE',  ( 0.000000000000000000, -31.46837873495025306, 68.27212725128265447 ) ) ;
#47416 = EDGE_CURVE ( 'NONE', #29028, #13811, #39681, .T. ) ;
#47417 = CYLINDRICAL_SURFACE ( 'NONE', #24438, 42.00000000000000000 ) ;
#47418 = AXIS2_PLACEMENT_3D ( 'NONE', #23404, #41539, #34182 ) ;
#47420 = EDGE_CURVE ( 'NONE', #44570, #15125, #42821, .T. ) ;
#47419 = SURFACE_STYLE_FILL_AREA ( #32496 ) ;
#47421 = CIRCLE ( 'NONE', #17711, 77.49899999999999523 ) ;
#47422 = FACE_OUTER_BOUND ( 'NONE', #48020, .T. ) ;
#47423 = ORIENTED_EDGE ( 'NONE', *, *, #25793, .T. ) ;
#47425 = EDGE_CURVE ( 'NONE', #2149, #9566, #27969, .T. ) ;
#47424 = CYLINDRICAL_SURFACE ( 'NONE', #20983, 82.00000000000000000 ) ;
#47426 = VERTEX_POINT ( 'NONE', #35519 ) ;
#47427 = CYLINDRICAL_SURFACE ( 'NONE', #37149, 82.00000000000000000 ) ;
#47428 = DIRECTION ( 'NONE',  ( -1.000000000000000000, 0.000000000000000000, -0.000000000000000000 ) ) ;
#47429 = EDGE_CURVE ( 'NONE', #14290, #31219, #45888, .T. ) ;
#47430 = ORIENTED_EDGE ( 'NONE', *, *, #5203, .F. ) ;
#47431 = CARTESIAN_POINT ( 'NONE',  ( 11.99999999999999822, 73.95703589263975175, 23.16143007188452785 ) ) ;
#47432 = DIRECTION ( 'NONE',  ( 1.000000000000000000, 0.000000000000000000, 0.000000000000000000 ) ) ;
#47433 = DIRECTION ( 'NONE',  ( -1.000000000000000000, -0.000000000000000000, -0.000000000000000000 ) ) ;
#47434 = DIRECTION ( 'NONE',  ( -1.000000000000000000, -0.000000000000000000, -0.000000000000000000 ) ) ;
#47435 = AXIS2_PLACEMENT_3D ( 'NONE', #32949, #18014, #26096 ) ;
#47436 = DIRECTION ( 'NONE',  ( -1.000000000000000000, 0.000000000000000000, 0.000000000000000000 ) ) ;
#47437 = CARTESIAN_POINT ( 'NONE',  ( 0.000000000000000000, 81.34940948281337114, 10.30890764327411979 ) ) ;
#47438 = CARTESIAN_POINT ( 'NONE',  ( 0.000000000000000000, 37.22597642581158084, -5.202137450156524068 ) ) ;
#47439 = LINE ( 'NONE', #13427, #15139 ) ;
#47440 = EDGE_LOOP ( 'NONE', ( #11635, #3580, #20260, #8594 ) ) ;
#47441 = AXIS2_PLACEMENT_3D ( 'NONE', #20390, #35578, #16494 ) ;
#47442 = ORIENTED_EDGE ( 'NONE', *, *, #30848, .F. ) ;
#47443 = DIRECTION ( 'NONE',  ( 0.000000000000000000, 0.2079116908177664480, -0.9781476007338041345 ) ) ;
#47444 = VECTOR ( 'NONE', #1389, 1000.000000000000000 ) ;
#47445 = DIRECTION ( 'NONE',  ( 0.000000000000000000, 0.000000000000000000, 1.000000000000000000 ) ) ;
#47446 = ORIENTED_EDGE ( 'NONE', *, *, #3543, .F. ) ;
#47447 = CIRCLE ( 'NONE', #13855, 77.49899999999999523 ) ;
#47448 = EDGE_CURVE ( 'NONE', #42424, #38396, #35989, .T. ) ;
#47449 = LINE ( 'NONE', #36899, #21039 ) ;
#47450 = ADVANCED_FACE ( 'NONE', ( #20835 ), #43586, .T. ) ;
#47451 = ORIENTED_EDGE ( 'NONE', *, *, #38441, .T. ) ;
#47452 = ORIENTED_EDGE ( 'NONE', *, *, #22555, .T. ) ;
#47453 = ORIENTED_EDGE ( 'NONE', *, *, #15432, .F. ) ;
#47454 = EDGE_CURVE ( 'NONE', #24216, #3270, #9197, .T. ) ;
#47455 = AXIS2_PLACEMENT_3D ( 'NONE', #29947, #32890, #3268 ) ;
#47456 = DIRECTION ( 'NONE',  ( 0.000000000000000000, 0.000000000000000000, 1.000000000000000000 ) ) ;
#47457 = VERTEX_POINT ( 'NONE', #27044 ) ;
#47458 = CARTESIAN_POINT ( 'NONE',  ( 12.00000000000000000, -25.60904388321925040, -6.976881207771165272 ) ) ;
#47459 = ORIENTED_EDGE ( 'NONE', *, *, #19923, .T. ) ;
#47460 = LINE ( 'NONE', #17595, #1746 ) ;
#47461 = AXIS2_PLACEMENT_3D ( 'NONE', #45442, #34183, #41540 ) ;
#47462 = DIRECTION ( 'NONE',  ( -1.000000000000000000, 0.000000000000000000, 0.000000000000000000 ) ) ;
#47463 = DIRECTION ( 'NONE',  ( 1.000000000000000000, 0.000000000000000000, -0.000000000000000000 ) ) ;
#47464 = EDGE_LOOP ( 'NONE', ( #12133, #16587, #36388, #18629 ) ) ;
#47465 = EDGE_CURVE ( 'NONE', #13778, #11582, #46790, .T. ) ;
#47466 = CARTESIAN_POINT ( 'NONE',  ( 0.000000000000000000, 6.903761155837774943, 77.19088730480525840 ) ) ;
#47467 = EDGE_CURVE ( 'NONE', #13807, #20955, #34975, .T. ) ;
#47468 = ORIENTED_EDGE ( 'NONE', *, *, #6753, .F. ) ;
#47469 = DIRECTION ( 'NONE',  ( 0.000000000000000000, -0.9510565162951565288, 0.3090169943749382919 ) ) ;
#47470 = FACE_OUTER_BOUND ( 'NONE', #6116, .T. ) ;
#47471 = AXIS2_PLACEMENT_3D ( 'NONE', #23409, #12410, #34410 ) ;
#47472 = ORIENTED_EDGE ( 'NONE', *, *, #45948, .T. ) ;
#47473 = EDGE_LOOP ( 'NONE', ( #23586, #24581, #45138, #3928 ) ) ;
#47474 = CARTESIAN_POINT ( 'NONE',  ( 0.000000000000000000, 37.16516213103285082, -4.992566952384588141 ) ) ;
#47475 = DIRECTION ( 'NONE',  ( 0.000000000000000000, 0.5000000000000039968, -0.8660254037844363761 ) ) ;
#47476 = ORIENTED_EDGE ( 'NONE', *, *, #1090, .F. ) ;
#47477 = ORIENTED_EDGE ( 'NONE', *, *, #23695, .T. ) ;
#47478 = DIRECTION ( 'NONE',  ( -1.000000000000000000, 0.000000000000000000, -0.000000000000000000 ) ) ;
#47479 = CARTESIAN_POINT ( 'NONE',  ( 0.000000000000000000, 0.000000000000000000, -54.99999999999998579 ) ) ;
#47480 = CYLINDRICAL_SURFACE ( 'NONE', #26080, 82.00000000000000000 ) ;
#47481 = CARTESIAN_POINT ( 'NONE',  ( 5.000000000000002665, 8.966570791700698706, 81.50828551894228724 ) ) ;
#47482 = EDGE_CURVE ( 'NONE', #1013, #40177, #17776, .T. ) ;
#47483 = AXIS2_PLACEMENT_3D ( 'NONE', #18599, #47491, #25933 ) ;
#47484 = CYLINDRICAL_SURFACE ( 'NONE', #9879, 82.00000000000000000 ) ;
#47485 = CARTESIAN_POINT ( 'NONE',  ( 5.000000000000002665, -34.94270380257693631, 74.18225833017875459 ) ) ;
#47486 = DIRECTION ( 'NONE',  ( 0.000000000000000000, 0.000000000000000000, 1.000000000000000000 ) ) ;
#47487 = CARTESIAN_POINT ( 'NONE',  ( 0.000000000000000000, -10.41901085202107247, 40.68715046381925049 ) ) ;
#47488 = CARTESIAN_POINT ( 'NONE',  ( 12.00000000000000000, 22.07842321921480888, -8.187992925817425771 ) ) ;
#47489 = LINE ( 'NONE', #47259, #5342 ) ;
#47490 = SHAPE_REPRESENTATION_RELATIONSHIP ( 'NONE' , 'NONE' ,  #2782, #1820 ) ;
#47491 = DIRECTION ( 'NONE',  ( -1.000000000000000000, 0.000000000000000000, -0.000000000000000000 ) ) ;
#47492 = ORIENTED_EDGE ( 'NONE', *, *, #471, .T. ) ;
#47493 = ORIENTED_EDGE ( 'NONE', *, *, #17073, .T. ) ;
#47494 = AXIS2_PLACEMENT_3D ( 'NONE', #47751, #14240, #29158 ) ;
#47495 = FACE_OUTER_BOUND ( 'NONE', #32739, .T. ) ;
#47496 = CONTEXT_DEPENDENT_SHAPE_REPRESENTATION ( #30090, #38292 ) ;
#47497 = AXIS2_PLACEMENT_3D ( 'NONE', #5782, #13127, #29188 ) ;
#47498 = CARTESIAN_POINT ( 'NONE',  ( 0.000000000000000000, 30.80686688397041451, -21.53537804866048688 ) ) ;
#47499 = ORIENTED_EDGE ( 'NONE', *, *, #31067, .F. ) ;
#47500 = ORIENTED_EDGE ( 'NONE', *, *, #45493, .F. ) ;
#47501 = EDGE_CURVE ( 'NONE', #22663, #24556, #21295, .T. ) ;
#47502 = DIRECTION ( 'NONE',  ( 0.000000000000000000, 0.3090169943749442316, 0.9510565162951545304 ) ) ;
#47503 = FACE_OUTER_BOUND ( 'NONE', #48409, .T. ) ;
#47504 = EDGE_CURVE ( 'NONE', #28861, #36901, #44304, .T. ) ;
#47505 = EDGE_LOOP ( 'NONE', ( #12259, #13657, #29865, #2696 ) ) ;
#47506 = EDGE_CURVE ( 'NONE', #19563, #36269, #18354, .T. ) ;
#47507 = VECTOR ( 'NONE', #47879, 1000.000000000000000 ) ;
#47508 = EDGE_LOOP ( 'NONE', ( #12252, #42961, #10641, #9564 ) ) ;
#47509 = DIRECTION ( 'NONE',  ( -1.000000000000000000, 0.000000000000000000, 0.000000000000000000 ) ) ;
#47510 = DIRECTION ( 'NONE',  ( -1.000000000000000000, 0.000000000000000000, -0.000000000000000000 ) ) ;
#47511 = ORIENTED_EDGE ( 'NONE', *, *, #18333, .F. ) ;
#47512 = DIRECTION ( 'NONE',  ( 0.000000000000000000, 0.000000000000000000, 1.000000000000000000 ) ) ;
#47513 = VERTEX_POINT ( 'NONE', #40873 ) ;
#47514 = FACE_OUTER_BOUND ( 'NONE', #36442, .T. ) ;
#47515 = ORIENTED_EDGE ( 'NONE', *, *, #22385, .F. ) ;
#47516 = DIRECTION ( 'NONE',  ( -0.000000000000000000, -0.000000000000000000, -1.000000000000000000 ) ) ;
#47517 = ADVANCED_FACE ( 'NONE', ( #11013 ), #29852, .T. ) ;
#47518 = CARTESIAN_POINT ( 'NONE',  ( 0.000000000000000000, 33.00180498840072829, -17.80606268964504935 ) ) ;
#47519 = CARTESIAN_POINT ( 'NONE',  ( 0.000000000000000000, -22.90783923731685334, 78.73519480814945837 ) ) ;
#47520 = ADVANCED_FACE ( 'NONE', ( #29379 ), #6620, .F. ) ;
#47522 = DIRECTION ( 'NONE',  ( -1.000000000000000000, -0.000000000000000000, -0.000000000000000000 ) ) ;
#47521 = CIRCLE ( 'NONE', #36590, 31.99999999999998579 ) ;
#47523 = DIRECTION ( 'NONE',  ( -1.000000000000000000, 0.000000000000000000, -0.000000000000000000 ) ) ;
#47524 = ORIENTED_EDGE ( 'NONE', *, *, #26550, .T. ) ;
#47525 = CARTESIAN_POINT ( 'NONE',  ( 10.00000000000000000, -2.663952781845854378, -41.91543099594820632 ) ) ;
#47526 = ORIENTED_EDGE ( 'NONE', *, *, #23068, .F. ) ;
#47527 = EDGE_LOOP ( 'NONE', ( #2494, #37168, #10590, #38996 ) ) ;
#47528 = DIRECTION ( 'NONE',  ( -0.4796670183876294291, 0.8774505977381983346, 0.000000000000000000 ) ) ;
#47529 = LINE ( 'NONE', #43859, #2706 ) ;
#47530 = VERTEX_POINT ( 'NONE', #29121 ) ;
#47531 = VECTOR ( 'NONE', #6385, 1000.000000000000000 ) ;
#47532 = CARTESIAN_POINT ( 'NONE',  ( -12.49999999999999645, 0.000000000000000000, -125.0000000000000000 ) ) ;
#47533 = CARTESIAN_POINT ( 'NONE',  ( 0.1915406271734537980, -118.5122795329289858, 2.500000000000000000 ) ) ;
#47534 = DIRECTION ( 'NONE',  ( -1.000000000000000000, 0.000000000000000000, 0.000000000000000000 ) ) ;
#47535 = VERTEX_POINT ( 'NONE', #28884 ) ;
#47536 = CARTESIAN_POINT ( 'NONE',  ( 0.000000000000000000, -19.89357724624987256, -12.59942793731086041 ) ) ;
#47537 = DIRECTION ( 'NONE',  ( -0.000000000000000000, 0.1045284632676437703, -0.9945218953682742891 ) ) ;
#47538 = ADVANCED_FACE ( 'NONE', ( #48216 ), #21554, .T. ) ;
#47539 = CARTESIAN_POINT ( 'NONE',  ( 0.000000000000000000, -120.0000000000000000, 5.500000000000000000 ) ) ;
#47540 = DIRECTION ( 'NONE',  ( 0.000000000000000000, 0.000000000000000000, 1.000000000000000000 ) ) ;
#47541 = DIRECTION ( 'NONE',  ( 0.000000000000000000, 0.000000000000000000, 1.000000000000000000 ) ) ;
#47542 = DIRECTION ( 'NONE',  ( 0.000000000000000000, 0.8090169943749486725, -0.5877852522924714718 ) ) ;
#47543 = CARTESIAN_POINT ( 'NONE',  ( 12.50000000000000000, -107.5000000000000000, 40.00000000000000000 ) ) ;
#47544 = ORIENTED_EDGE ( 'NONE', *, *, #36824, .F. ) ;
#47545 = CARTESIAN_POINT ( 'NONE',  ( 11.99999999999999822, -14.67089635893658794, -73.72996012237454977 ) ) ;
#47546 = DIRECTION ( 'NONE',  ( 0.000000000000000000, 0.000000000000000000, 1.000000000000000000 ) ) ;
#47547 = STYLED_ITEM ( 'NONE', ( #20227 ), #29206 ) ;
#47548 = VECTOR ( 'NONE', #29671, 1000.000000000000000 ) ;
#47549 = VERTEX_POINT ( 'NONE', #40159 ) ;
#47550 = DIRECTION ( 'NONE',  ( 0.000000000000000000, 0.000000000000000000, 1.000000000000000000 ) ) ;
#47551 = ORIENTED_EDGE ( 'NONE', *, *, #29512, .T. ) ;
#47552 = DIRECTION ( 'NONE',  ( 1.000000000000000000, -0.000000000000000000, -0.000000000000000000 ) ) ;
#47553 = CARTESIAN_POINT ( 'NONE',  ( 5.000000000000000000, -27.75498641678764855, 31.52238457039590358 ) ) ;
#47554 = ORIENTED_EDGE ( 'NONE', *, *, #21547, .T. ) ;
#47555 = DIRECTION ( 'NONE',  ( 0.000000000000000000, 0.000000000000000000, 1.000000000000000000 ) ) ;
#47557 = EDGE_CURVE ( 'NONE', #45718, #30853, #38908, .T. ) ;
#47556 = AXIS2_PLACEMENT_3D ( 'NONE', #33240, #40108, #25157 ) ;
#47558 = ORIENTED_EDGE ( 'NONE', *, *, #34309, .T. ) ;
#47559 = EDGE_CURVE ( 'NONE', #8929, #16330, #22477, .T. ) ;
#47560 = AXIS2_PLACEMENT_3D ( 'NONE', #46146, #35611, #42468 ) ;
#47561 = ADVANCED_FACE ( 'NONE', ( #25683 ), #10778, .F. ) ;
#47562 = FACE_OUTER_BOUND ( 'NONE', #10854, .T. ) ;
#47563 = ORIENTED_EDGE ( 'NONE', *, *, #29172, .T. ) ;
#47564 = EDGE_CURVE ( 'NONE', #5271, #47208, #3413, .T. ) ;
#47565 = DIRECTION ( 'NONE',  ( 1.000000000000000000, 0.000000000000000000, 0.000000000000000000 ) ) ;
#47566 = CARTESIAN_POINT ( 'NONE',  ( 11.99999999999999822, 36.73666225445988687, -65.58780272294035285 ) ) ;
#47567 = ORIENTED_EDGE ( 'NONE', *, *, #5690, .T. ) ;
#47568 = CARTESIAN_POINT ( 'NONE',  ( 0.000000000000000000, -0.6853352020787742971, -37.58145647212455032 ) ) ;
#47569 = ORIENTED_EDGE ( 'NONE', *, *, #29459, .F. ) ;
#47570 = DIRECTION ( 'NONE',  ( 0.000000000000000000, 0.000000000000000000, 1.000000000000000000 ) ) ;
#47571 = CARTESIAN_POINT ( 'NONE',  ( 0.5480546763151027401, -96.50639159107802811, -2.500000000000000000 ) ) ;
#47572 = ADVANCED_FACE ( 'NONE', ( #33520 ), #48448, .T. ) ;
#47573 = CARTESIAN_POINT ( 'NONE',  ( 10.00000000000000000, 35.95386929396241271, 10.96151621346552751 ) ) ;
#47574 = CIRCLE ( 'NONE', #29620, 31.99999999999999289 ) ;
#47575 = ORIENTED_EDGE ( 'NONE', *, *, #24155, .T. ) ;
#47576 = CARTESIAN_POINT ( 'NONE',  ( 11.99999999999999822, -59.03961581697432592, 46.53671651293927880 ) ) ;
#47577 = ORIENTED_EDGE ( 'NONE', *, *, #24818, .F. ) ;
#47578 = ORIENTED_EDGE ( 'NONE', *, *, #11621, .F. ) ;
#47579 = EDGE_CURVE ( 'NONE', #37275, #10994, #2939, .T. ) ;
#47580 = APPLICATION_CONTEXT ( 'automotive_design' ) ;
#47581 = FACE_BOUND ( 'NONE', #17185, .T. ) ;
#47582 = DIRECTION ( 'NONE',  ( 0.000000000000000000, -0.9238795325112822976, -0.3826834323651008285 ) ) ;
#47583 = LINE ( 'NONE', #13583, #40762 ) ;
#47584 = LINE ( 'NONE', #14064, #35295 ) ;
#47585 = EDGE_LOOP ( 'NONE', ( #15788, #28555, #47167, #33297 ) ) ;
#47586 = DIRECTION ( 'NONE',  ( 0.000000000000000000, 0.000000000000000000, 1.000000000000000000 ) ) ;
#47587 = DIRECTION ( 'NONE',  ( 0.000000000000000000, 0.8090169943749445647, 0.5877852522924771339 ) ) ;
#47588 = FACE_OUTER_BOUND ( 'NONE', #32685, .T. ) ;
#47589 = DIRECTION ( 'NONE',  ( 0.000000000000000000, -0.3090169943749548898, 0.9510565162951511997 ) ) ;
#47590 = DIRECTION ( 'NONE',  ( 1.000000000000000000, 0.000000000000000000, 0.000000000000000000 ) ) ;
#47591 = EDGE_CURVE ( 'NONE', #39073, #34102, #28730, .T. ) ;
#47592 = DIRECTION ( 'NONE',  ( 1.000000000000000000, 0.000000000000000000, -0.000000000000000000 ) ) ;
#47593 = ORIENTED_EDGE ( 'NONE', *, *, #32542, .T. ) ;
#47594 = CIRCLE ( 'NONE', #33544, 77.49899999999999523 ) ;
#47595 = DIRECTION ( 'NONE',  ( 1.000000000000000000, 0.000000000000000000, 0.000000000000000000 ) ) ;
#47596 = VECTOR ( 'NONE', #25105, 1000.000000000000227 ) ;
#47597 = FACE_OUTER_BOUND ( 'NONE', #15190, .T. ) ;
#47598 = CARTESIAN_POINT ( 'NONE',  ( 10.00000000000000000, -17.67226234102849958, 33.17418723428301774 ) ) ;
#47599 = AXIS2_PLACEMENT_3D ( 'NONE', #44634, #4007, #34095 ) ;
#47600 = DIRECTION ( 'NONE',  ( -1.000000000000000000, 0.000000000000000000, -0.000000000000000000 ) ) ;
#47601 = ADVANCED_FACE ( 'NONE', ( #17864 ), #32788, .T. ) ;
#47602 = DIRECTION ( 'NONE',  ( 0.6862798483830533369, 0.7273375899149812085, -0.000000000000000000 ) ) ;
#47603 = CARTESIAN_POINT ( 'NONE',  ( 11.99999999999999822, -39.78640506895559525, -66.50666863322042843 ) ) ;
#47604 = ORIENTED_EDGE ( 'NONE', *, *, #436, .T. ) ;
#47605 = DIRECTION ( 'NONE',  ( -0.000000000000000000, -0.000000000000000000, -1.000000000000000000 ) ) ;
#47606 = CARTESIAN_POINT ( 'NONE',  ( 11.99999999999999822, 73.44644590900094272, -24.73286445877629802 ) ) ;
#47607 = VERTEX_POINT ( 'NONE', #21781 ) ;
#47608 = EDGE_LOOP ( 'NONE', ( #46453, #22900, #41541, #47749 ) ) ;
#47609 = ORIENTED_EDGE ( 'NONE', *, *, #31092, .F. ) ;
#47610 = ORIENTED_EDGE ( 'NONE', *, *, #45919, .T. ) ;
#47611 = EDGE_CURVE ( 'NONE', #31567, #11474, #3166, .T. ) ;
#47612 = ORIENTED_EDGE ( 'NONE', *, *, #36125, .T. ) ;
#47613 = EDGE_CURVE ( 'NONE', #16358, #33111, #36548, .T. ) ;
#47614 = CARTESIAN_POINT ( 'NONE',  ( 0.000000000000000000, -69.42325613327415113, -34.44570377933673200 ) ) ;
#47615 = VERTEX_POINT ( 'NONE', #37681 ) ;
#47616 = EDGE_CURVE ( 'NONE', #39296, #40664, #45037, .T. ) ;
#47617 = ORIENTED_EDGE ( 'NONE', *, *, #11250, .T. ) ;
#47618 = CIRCLE ( 'NONE', #22619, 82.00000000000000000 ) ;
#47619 = DIRECTION ( 'NONE',  ( 0.000000000000000000, 0.000000000000000000, 1.000000000000000000 ) ) ;
#47620 = EDGE_CURVE ( 'NONE', #37035, #21662, #35821, .T. ) ;
#47621 = DIRECTION ( 'NONE',  ( 0.000000000000000000, 1.000000000000000000, 7.228014483236689653E-16 ) ) ;
#47623 = ORIENTED_EDGE ( 'NONE', *, *, #42506, .F. ) ;
#47622 = CARTESIAN_POINT ( 'NONE',  ( 0.000000000000000000, 0.000000000000000000, 0.000000000000000000 ) ) ;
#47624 = AXIS2_PLACEMENT_3D ( 'NONE', #6760, #14097, #39584 ) ;
#47625 = VERTEX_POINT ( 'NONE', #8535 ) ;
#47626 = LINE ( 'NONE', #14108, #14892 ) ;
#47627 = ORIENTED_EDGE ( 'NONE', *, *, #42063, .T. ) ;
#47628 = EDGE_LOOP ( 'NONE', ( #39083, #28366, #46026, #9278 ) ) ;
#47629 = ORIENTED_EDGE ( 'NONE', *, *, #46120, .F. ) ;
#47630 = LINE ( 'NONE', #14112, #44393 ) ;
#47631 = DIRECTION ( 'NONE',  ( 0.000000000000000000, 0.000000000000000000, 1.000000000000000000 ) ) ;
#47632 = DIRECTION ( 'NONE',  ( -1.000000000000000000, 0.000000000000000000, 0.000000000000000000 ) ) ;
#47633 = ORIENTED_EDGE ( 'NONE', *, *, #5376, .F. ) ;
#47634 = AXIS2_PLACEMENT_3D ( 'NONE', #38633, #1424, #5099 ) ;
#47635 = CARTESIAN_POINT ( 'NONE',  ( 15.00000000000000000, -10.45096189432314127, 21.10159698893440350 ) ) ;
#47636 = ORIENTED_EDGE ( 'NONE', *, *, #7937, .T. ) ;
#47637 = FACE_OUTER_BOUND ( 'NONE', #27203, .T. ) ;
#47638 = DIRECTION ( 'NONE',  ( -1.000000000000000000, 0.000000000000000000, -0.000000000000000000 ) ) ;
#47639 = CARTESIAN_POINT ( 'NONE',  ( 0.000000000000000000, 0.000000000000000000, 0.000000000000000000 ) ) ;
#47640 = LINE ( 'NONE', #3093, #17465 ) ;
#47641 = CARTESIAN_POINT ( 'NONE',  ( 0.000000000000000000, 0.000000000000000000, 0.000000000000000000 ) ) ;
#47642 = CARTESIAN_POINT ( 'NONE',  ( 0.000000000000000000, -22.64427369931148348, -30.00120703465229965 ) ) ;
#47643 = CARTESIAN_POINT ( 'NONE',  ( -3.000000000000000000, 0.000000000000000000, 0.000000000000000000 ) ) ;
#47644 = CARTESIAN_POINT ( 'NONE',  ( -3.000000000000000000, -13.04903810567647682, -19.60159698893442481 ) ) ;
#47645 = EDGE_LOOP ( 'NONE', ( #17412, #32458, #15115, #3243 ) ) ;
#47646 = CARTESIAN_POINT ( 'NONE',  ( 10.00000000000000000, 29.01471420065674423, -76.69515212745983490 ) ) ;
#47647 = VERTEX_POINT ( 'NONE', #45273 ) ;
#47648 = DIRECTION ( 'NONE',  ( 0.000000000000000000, 0.3826834323650842862, 0.9238795325112890700 ) ) ;
#47649 = DIRECTION ( 'NONE',  ( 0.000000000000000000, 0.000000000000000000, 1.000000000000000000 ) ) ;
#47650 = CARTESIAN_POINT ( 'NONE',  ( -235.0000123116479926, -117.0000000000000142, -2.500000000000000000 ) ) ;
#47651 = DIRECTION ( 'NONE',  ( -1.000000000000000000, -0.000000000000000000, 0.000000000000000000 ) ) ;
#47652 = CARTESIAN_POINT ( 'NONE',  ( 0.1915406271734537980, -118.5122795329289858, -2.500000000000000000 ) ) ;
#47653 = VECTOR ( 'NONE', #16909, 1000.000000000000000 ) ;
#47654 = ORIENTED_EDGE ( 'NONE', *, *, #35855, .T. ) ;
#47655 = DIRECTION ( 'NONE',  ( -1.000000000000000000, 0.000000000000000000, -0.000000000000000000 ) ) ;
#47656 = CARTESIAN_POINT ( 'NONE',  ( 0.000000000000000000, 80.55351364060589958, 15.33399622253511829 ) ) ;
#47657 = CIRCLE ( 'NONE', #39082, 77.49899999999999523 ) ;
#47658 = LINE ( 'NONE', #2884, #26252 ) ;
#47659 = AXIS2_PLACEMENT_3D ( 'NONE', #23130, #19211, #40766 ) ;
#47660 = CARTESIAN_POINT ( 'NONE',  ( 11.99999999999999822, 0.000000000000000000, 0.000000000000000000 ) ) ;
#47661 = SURFACE_STYLE_USAGE ( .BOTH. , #7035 ) ;
#47662 = AXIS2_PLACEMENT_3D ( 'NONE', #47643, #18023, #2866 ) ;
#47663 = VERTEX_POINT ( 'NONE', #34003 ) ;
#47664 = CONICAL_SURFACE ( 'NONE', #26581, 15.39727592589476579, 0.2094395102393128150 ) ;
#47665 = EDGE_CURVE ( 'NONE', #22663, #2423, #22517, .T. ) ;
#47666 = ORIENTED_EDGE ( 'NONE', *, *, #18505, .F. ) ;
#47667 = FACE_OUTER_BOUND ( 'NONE', #22775, .T. ) ;
#47668 = EDGE_CURVE ( 'NONE', #34199, #14963, #38170, .T. ) ;
#47669 = DIRECTION ( 'NONE',  ( -1.000000000000000000, -6.951859121168206841E-17, 0.000000000000000000 ) ) ;
#47670 = VERTEX_POINT ( 'NONE', #12238 ) ;
#47671 = EDGE_CURVE ( 'NONE', #20465, #43248, #4412, .T. ) ;
#47672 = DIRECTION ( 'NONE',  ( 0.000000000000000000, 0.3090169943749482839, -0.9510565162951533091 ) ) ;
#47673 = EDGE_LOOP ( 'NONE', ( #40818, #20587, #25832, #30665 ) ) ;
#47674 = ORIENTED_EDGE ( 'NONE', *, *, #12478, .F. ) ;
#47675 = EDGE_CURVE ( 'NONE', #17321, #31583, #44414, .T. ) ;
#47676 = ORIENTED_EDGE ( 'NONE', *, *, #41931, .T. ) ;
#47677 = DIRECTION ( 'NONE',  ( 1.000000000000000000, 0.000000000000000000, 0.000000000000000000 ) ) ;
#47679 = ORIENTED_EDGE ( 'NONE', *, *, #322, .F. ) ;
#47678 = VECTOR ( 'NONE', #10072, 1000.000000000000000 ) ;
#47680 = DIRECTION ( 'NONE',  ( -1.000000000000000000, -0.000000000000000000, 0.000000000000000000 ) ) ;
#47681 = ORIENTED_EDGE ( 'NONE', *, *, #16163, .T. ) ;
#47682 = LINE ( 'NONE', #14419, #17336 ) ;
#47683 = AXIS2_PLACEMENT_3D ( 'NONE', #11377, #19409, #27026 ) ;
#47684 = CIRCLE ( 'NONE', #23483, 77.49899999999999523 ) ;
#47685 = DIRECTION ( 'NONE',  ( -1.000000000000000000, 0.000000000000000000, -0.000000000000000000 ) ) ;
#47686 = DIRECTION ( 'NONE',  ( -1.000000000000000000, 0.000000000000000000, -0.000000000000000000 ) ) ;
#47687 = ORIENTED_EDGE ( 'NONE', *, *, #15431, .F. ) ;
#47688 = AXIS2_PLACEMENT_3D ( 'NONE', #27968, #42890, #28190 ) ;
#47689 = ORIENTED_EDGE ( 'NONE', *, *, #13086, .T. ) ;
#47690 = CIRCLE ( 'NONE', #34420, 16.00000000000000000 ) ;
#47691 = LINE ( 'NONE', #3645, #12542 ) ;
#47692 = CYLINDRICAL_SURFACE ( 'NONE', #43108, 31.99999999999999289 ) ;
#47693 = EDGE_LOOP ( 'NONE', ( #31587, #40310, #11759, #15007 ) ) ;
#47694 = VECTOR ( 'NONE', #8570, 1000.000000000000000 ) ;
#47695 = ORIENTED_EDGE ( 'NONE', *, *, #40629, .F. ) ;
#47696 = CYLINDRICAL_SURFACE ( 'NONE', #15061, 1.000000000000000000 ) ;
#47697 = CARTESIAN_POINT ( 'NONE',  ( -10.90076147243505211, 1.679381574624689562E-15, -13.71319123027096865 ) ) ;
#47698 = ORIENTED_EDGE ( 'NONE', *, *, #6422, .F. ) ;
#47699 = EDGE_LOOP ( 'NONE', ( #16211, #43538 ) ) ;
#47700 = DIRECTION ( 'NONE',  ( -0.7071067811865474617, 8.659560562354932858E-17, -0.7071067811865474617 ) ) ;
#47701 = CARTESIAN_POINT ( 'NONE',  ( -12.50000000000000000, -132.5000000000000000, -40.00000000000000000 ) ) ;
#47702 = CYLINDRICAL_SURFACE ( 'NONE', #27710, 42.00000000000000000 ) ;
#47703 = CARTESIAN_POINT ( 'NONE',  ( 20.85212586905262100, -130.9402397935870965, 5.500000000000000000 ) ) ;
#47704 = DIRECTION ( 'NONE',  ( -1.000000000000000000, 0.000000000000000000, 0.000000000000000000 ) ) ;
#47705 = EDGE_CURVE ( 'NONE', #14023, #2189, #17046, .T. ) ;
#47706 = CARTESIAN_POINT ( 'NONE',  ( 0.000000000000000000, 16.00000000000000000, 2.500000000000000000 ) ) ;
#47707 = CARTESIAN_POINT ( 'NONE',  ( 0.000000000000000000, 0.8261519478431255115, 77.49459641780886443 ) ) ;
#47708 = EDGE_CURVE ( 'NONE', #35935, #36518, #5323, .T. ) ;
#47709 = FACE_OUTER_BOUND ( 'NONE', #35163, .T. ) ;
#47710 = DIRECTION ( 'NONE',  ( -1.000000000000000000, 0.000000000000000000, -0.000000000000000000 ) ) ;
#47711 =( LENGTH_UNIT ( ) NAMED_UNIT ( * ) SI_UNIT ( .MILLI., .METRE. ) );
#47712 = EDGE_CURVE ( 'NONE', #16632, #46304, #19073, .T. ) ;
#47713 = CARTESIAN_POINT ( 'NONE',  ( -3.702536634196095910, 8.043911037661889196, 32.98187577049606745 ) ) ;
#47714 = VERTEX_POINT ( 'NONE', #946 ) ;
#47715 = ORIENTED_EDGE ( 'NONE', *, *, #9629, .T. ) ;
#47716 = ORIENTED_EDGE ( 'NONE', *, *, #5096, .F. ) ;
#47717 = CIRCLE ( 'NONE', #26632, 42.00000000000000000 ) ;
#47718 = AXIS2_PLACEMENT_3D ( 'NONE', #1649, #16577, #46445 ) ;
#47719 = UNCERTAINTY_MEASURE_WITH_UNIT (LENGTH_MEASURE( 1.000000000000000082E-05 ), #4820, 'distance_accuracy_value', 'NONE');
#47720 = CARTESIAN_POINT ( 'NONE',  ( -7.469491406282094736, 4.756046723998911929, 42.00000000000001421 ) ) ;
#47721 = AXIS2_PLACEMENT_3D ( 'NONE', #17591, #47456, #2902 ) ;
#47722 = EDGE_CURVE ( 'NONE', #4001, #3020, #487, .T. ) ;
#47723 = DIRECTION ( 'NONE',  ( 0.000000000000000000, 0.9723699203976773342, -0.2334453638559024213 ) ) ;
#47724 = ORIENTED_EDGE ( 'NONE', *, *, #43947, .T. ) ;
#47725 = CIRCLE ( 'NONE', #17226, 31.99999999999999645 ) ;
#47726 = ADVANCED_FACE ( 'NONE', ( #26672 ), #23308, .T. ) ;
#47727 = ADVANCED_FACE ( 'NONE', ( #18821 ), #15180, .F. ) ;
#47728 = VECTOR ( 'NONE', #2438, 1000.000000000000000 ) ;
#47729 = VECTOR ( 'NONE', #39112, 1000.000000000000000 ) ;
#47730 = DIRECTION ( 'NONE',  ( 0.000000000000000000, 0.000000000000000000, 1.000000000000000000 ) ) ;
#47731 = PLANE ( 'NONE',  #26076 ) ;
#47732 = ORIENTED_EDGE ( 'NONE', *, *, #22330, .T. ) ;
#47733 =( NAMED_UNIT ( * ) SI_UNIT ( $, .STERADIAN. ) SOLID_ANGLE_UNIT ( ) );
#47734 = DIRECTION ( 'NONE',  ( 0.000000000000000000, 0.000000000000000000, 1.000000000000000000 ) ) ;
#47735 = DIRECTION ( 'NONE',  ( -1.000000000000000000, -0.000000000000000000, -0.000000000000000000 ) ) ;
#47736 = ORIENTED_EDGE ( 'NONE', *, *, #17472, .F. ) ;
#47737 = DIRECTION ( 'NONE',  ( 1.000000000000000000, 0.000000000000000000, 0.000000000000000000 ) ) ;
#47738 = ORIENTED_EDGE ( 'NONE', *, *, #2466, .T. ) ;
#47739 = DIRECTION ( 'NONE',  ( 0.000000000000000000, 0.000000000000000000, 1.000000000000000000 ) ) ;
#47740 = ORIENTED_EDGE ( 'NONE', *, *, #24717, .F. ) ;
#47741 = CARTESIAN_POINT ( 'NONE',  ( 0.000000000000000000, 15.33399622253601713, -80.55351364060572905 ) ) ;
#47742 = ORIENTED_EDGE ( 'NONE', *, *, #21564, .T. ) ;
#47743 = LINE ( 'NONE', #9840, #1920 ) ;
#47744 = DIRECTION ( 'NONE',  ( 0.000000000000000000, 0.000000000000000000, 1.000000000000000000 ) ) ;
#47745 = AXIS2_PLACEMENT_3D ( 'NONE', #40676, #7149, #22801 ) ;
#47747 = ORIENTED_EDGE ( 'NONE', *, *, #8126, .F. ) ;
#47746 = DIRECTION ( 'NONE',  ( -1.000000000000000000, 0.000000000000000000, 0.000000000000000000 ) ) ;
#47748 = DIRECTION ( 'NONE',  ( 0.000000000000000000, 0.000000000000000000, 1.000000000000000000 ) ) ;
#47749 = ORIENTED_EDGE ( 'NONE', *, *, #16567, .T. ) ;
#47750 = AXIS2_PLACEMENT_3D ( 'NONE', #5278, #1362, #16524 ) ;
#47751 = CARTESIAN_POINT ( 'NONE',  ( 11.99999999999999822, -75.11725578898466438, -2.956366410621452001 ) ) ;
#47752 = ORIENTED_EDGE ( 'NONE', *, *, #39973, .T. ) ;
#47753 = ORIENTED_EDGE ( 'NONE', *, *, #33044, .F. ) ;
#47754 = DIRECTION ( 'NONE',  ( -0.8774505977381983346, -0.4796670183876294291, 0.000000000000000000 ) ) ;
#47755 = CARTESIAN_POINT ( 'NONE',  ( 11.99999999999999822, -77.19088730480518734, -6.903761155838607166 ) ) ;
#47756 = AXIS2_PLACEMENT_3D ( 'NONE', #24946, #28146, #20806 ) ;
#47757 = CIRCLE ( 'NONE', #47012, 42.00000000000000000 ) ;
#47758 = CARTESIAN_POINT ( 'NONE',  ( 0.000000000000000000, -41.19522573413780009, 65.64334221924896440 ) ) ;
#47759 = DIRECTION ( 'NONE',  ( -1.000000000000000000, 0.000000000000000000, -0.000000000000000000 ) ) ;
#47760 = DIRECTION ( 'NONE',  ( 0.000000000000000000, 0.9876883405951383255, -0.1564344650402276216 ) ) ;
#47761 = VERTEX_POINT ( 'NONE', #22746 ) ;
#47762 = LINE ( 'NONE', #14253, #9338 ) ;
#47763 = CIRCLE ( 'NONE', #37618, 37.49900000000000233 ) ;
#47765 = EDGE_CURVE ( 'NONE', #22825, #9001, #30343, .T. ) ;
#47764 = LINE ( 'NONE', #41184, #21201 ) ;
#47766 = AXIS2_PLACEMENT_3D ( 'NONE', #38950, #35504, #8352 ) ;
#47767 = LINE ( 'NONE', #18144, #26272 ) ;
#47768 = ADVANCED_FACE ( 'NONE', ( #34240 ), #30577, .F. ) ;
#47769 = CYLINDRICAL_SURFACE ( 'NONE', #11383, 37.49900000000000233 ) ;
#47770 = CARTESIAN_POINT ( 'NONE',  ( -10.00000000000000000, 0.000000000000000000, 0.000000000000000000 ) ) ;
#47771 = LINE ( 'NONE', #17435, #6053 ) ;
#47772 = DIRECTION ( 'NONE',  ( -1.000000000000000000, -0.000000000000000000, 0.000000000000000000 ) ) ;
#47773 = AXIS2_PLACEMENT_3D ( 'NONE', #13220, #43322, #17118 ) ;
#47774 = EDGE_CURVE ( 'NONE', #7495, #40831, #25638, .T. ) ;
#47775 = ORIENTED_EDGE ( 'NONE', *, *, #30713, .F. ) ;
#47776 = ORIENTED_EDGE ( 'NONE', *, *, #11873, .T. ) ;
#47777 = DIRECTION ( 'NONE',  ( -1.000000000000000000, -0.000000000000000000, -0.000000000000000000 ) ) ;
#47778 = DIRECTION ( 'NONE',  ( 0.000000000000000000, 0.000000000000000000, 1.000000000000000000 ) ) ;
#47779 = DIRECTION ( 'NONE',  ( 0.000000000000000000, 0.000000000000000000, 1.000000000000000000 ) ) ;
#47780 = CARTESIAN_POINT ( 'NONE',  ( 6.000000000000000000, -81.50828551894234408, 8.966570791700414489 ) ) ;
#47781 = ADVANCED_FACE ( 'NONE', ( #18516 ), #3332, .T. ) ;
#47782 = ORIENTED_EDGE ( 'NONE', *, *, #4103, .F. ) ;
#47783 = VERTEX_POINT ( 'NONE', #22665 ) ;
#47784 = DIRECTION ( 'NONE',  ( 0.000000000000000000, 0.000000000000000000, 1.000000000000000000 ) ) ;
#47785 = EDGE_LOOP ( 'NONE', ( #35738, #30964, #16179, #19154 ) ) ;
#47786 = DIRECTION ( 'NONE',  ( 0.000000000000000000, 0.9510565162951521989, 0.3090169943749515591 ) ) ;
#47787 = APPLICATION_PROTOCOL_DEFINITION ( 'draft international standard', 'automotive_design', 1998, #39159 ) ;
#47788 = CARTESIAN_POINT ( 'NONE',  ( 11.41210121379327980, -99.40233154247455616, -2.500000000000000000 ) ) ;
#47789 = EDGE_LOOP ( 'NONE', ( #35045, #14242, #14713, #36801 ) ) ;
#47790 = ADVANCED_FACE ( 'NONE', ( #33673 ), #29766, .T. ) ;
#47791 = ADVANCED_FACE ( 'NONE', ( #44949 ), #2859, .T. ) ;
#47792 = AXIS2_PLACEMENT_3D ( 'NONE', #27737, #16238, #12799 ) ;
#47793 = CIRCLE ( 'NONE', #39218, 82.00000000000000000 ) ;
#47794 = CARTESIAN_POINT ( 'NONE',  ( 0.000000000000000000, 0.000000000000000000, 0.000000000000000000 ) ) ;
#47795 = ORIENTED_EDGE ( 'NONE', *, *, #1402, .F. ) ;
#47796 = CIRCLE ( 'NONE', #11866, 31.99999999999998934 ) ;
#47797 = EDGE_LOOP ( 'NONE', ( #15749, #19435, #40060, #22310 ) ) ;
#47798 = VECTOR ( 'NONE', #32026, 1000.000000000000114 ) ;
#47799 = EDGE_CURVE ( 'NONE', #29160, #16510, #18741, .T. ) ;
#47800 = DIRECTION ( 'NONE',  ( 0.000000000000000000, 0.3090169943749480064, -0.9510565162951534202 ) ) ;
#47801 = DIRECTION ( 'NONE',  ( 0.000000000000000000, 0.000000000000000000, 1.000000000000000000 ) ) ;
#47802 = DIRECTION ( 'NONE',  ( -0.000000000000000000, -0.000000000000000000, -1.000000000000000000 ) ) ;
#47803 = VECTOR ( 'NONE', #19752, 1000.000000000000000 ) ;
#47804 = ORIENTED_EDGE ( 'NONE', *, *, #11632, .F. ) ;
#47805 = DIRECTION ( 'NONE',  ( 0.000000000000000000, 0.000000000000000000, -1.000000000000000000 ) ) ;
#47806 = ORIENTED_EDGE ( 'NONE', *, *, #3866, .T. ) ;
#47807 = VERTEX_POINT ( 'NONE', #21937 ) ;
#47808 = DIRECTION ( 'NONE',  ( 0.000000000000000000, 0.000000000000000000, 1.000000000000000000 ) ) ;
#47809 = DIRECTION ( 'NONE',  ( -1.000000000000000000, 0.000000000000000000, 0.000000000000000000 ) ) ;
#47810 = DIRECTION ( 'NONE',  ( -1.000000000000000000, -0.000000000000000000, -0.000000000000000000 ) ) ;
#47811 = VERTEX_POINT ( 'NONE', #40329 ) ;
#47812 = ORIENTED_EDGE ( 'NONE', *, *, #14626, .F. ) ;
#47813 = CARTESIAN_POINT ( 'NONE',  ( 6.000000000000000000, 39.47590169984945163, -71.87247863392373404 ) ) ;
#47814 = EDGE_LOOP ( 'NONE', ( #3952, #40983, #48268, #943 ) ) ;
#47815 = EDGE_LOOP ( 'NONE', ( #26363, #22502, #40758, #19998 ) ) ;
#47816 = CARTESIAN_POINT ( 'NONE',  ( 0.000000000000000000, 0.000000000000000000, 0.000000000000000000 ) ) ;
#47817 = DIRECTION ( 'NONE',  ( -1.000000000000000000, -0.000000000000000000, 0.000000000000000000 ) ) ;
#47818 = DIRECTION ( 'NONE',  ( 0.000000000000000000, 0.000000000000000000, -1.000000000000000000 ) ) ;
#47819 = CARTESIAN_POINT ( 'NONE',  ( 10.00000000000000000, 41.76937507738788469, 62.50329211542452157 ) ) ;
#47820 = ORIENTED_EDGE ( 'NONE', *, *, #43142, .F. ) ;
#47821 = CARTESIAN_POINT ( 'NONE',  ( 15.00000000000000000, 0.000000000000000000, 0.000000000000000000 ) ) ;
#47822 = DIRECTION ( 'NONE',  ( -0.000000000000000000, -0.000000000000000000, -1.000000000000000000 ) ) ;
#47823 = CARTESIAN_POINT ( 'NONE',  ( 0.000000000000000000, 0.000000000000000000, 0.000000000000000000 ) ) ;
#47824 = CIRCLE ( 'NONE', #20471, 31.99999999999999289 ) ;
#47825 = CARTESIAN_POINT ( 'NONE',  ( 5.999999999999999112, -33.71516098798793593, 74.74816331893417498 ) ) ;
#47826 = CARTESIAN_POINT ( 'NONE',  ( 0.000000000000000000, -14.67089635893764665, 73.72996012237435082 ) ) ;
#47827 = ORIENTED_EDGE ( 'NONE', *, *, #13792, .T. ) ;
#47828 = VERTEX_POINT ( 'NONE', #141 ) ;
#47829 = CYLINDRICAL_SURFACE ( 'NONE', #32612, 32.00000000000000000 ) ;
#47830 = VECTOR ( 'NONE', #35240, 1000.000000000000000 ) ;
#47831 = ADVANCED_FACE ( 'NONE', ( #14619 ), #44698, .T. ) ;
#47832 = CARTESIAN_POINT ( 'NONE',  ( 11.99999999999999822, -73.95703589263990807, 23.16143007188399139 ) ) ;
#47833 = CARTESIAN_POINT ( 'NONE',  ( 11.99999999999999822, 0.8261519478431255115, 77.49459641780886443 ) ) ;
#47834 = EDGE_CURVE ( 'NONE', #11083, #16358, #28007, .T. ) ;
#47835 = VECTOR ( 'NONE', #28764, 1000.000000000000000 ) ;
#47836 = DIRECTION ( 'NONE',  ( -1.000000000000000000, -0.000000000000000000, 0.000000000000000000 ) ) ;
#47837 = DIRECTION ( 'NONE',  ( -1.000000000000000000, -0.000000000000000000, -0.000000000000000000 ) ) ;
#47838 = DIRECTION ( 'NONE',  ( -1.000000000000000000, 0.000000000000000000, 0.000000000000000000 ) ) ;
#47840 = EDGE_CURVE ( 'NONE', #6182, #21856, #40550, .T. ) ;
#47839 = ORIENTED_EDGE ( 'NONE', *, *, #35142, .F. ) ;
#47841 = DIRECTION ( 'NONE',  ( -1.000000000000000000, 0.000000000000000000, -0.000000000000000000 ) ) ;
#47842 = AXIS2_PLACEMENT_3D ( 'NONE', #37411, #8024, #3880 ) ;
#47843 = FACE_OUTER_BOUND ( 'NONE', #45147, .T. ) ;
#47844 = VERTEX_POINT ( 'NONE', #33206 ) ;
#47845 = ORIENTED_EDGE ( 'NONE', *, *, #33982, .T. ) ;
#47846 = EDGE_CURVE ( 'NONE', #25169, #11204, #628, .T. ) ;
#47847 = ORIENTED_EDGE ( 'NONE', *, *, #10041, .T. ) ;
#47848 = EDGE_CURVE ( 'NONE', #5621, #37239, #17785, .T. ) ;
#47849 = EDGE_LOOP ( 'NONE', ( #1971, #42020 ) ) ;
#47850 = CIRCLE ( 'NONE', #43950, 31.99999999999998579 ) ;
#47851 = LINE ( 'NONE', #2347, #47596 ) ;
#47852 = ORIENTED_EDGE ( 'NONE', *, *, #12430, .F. ) ;
#47853 = EDGE_LOOP ( 'NONE', ( #40502, #37989, #14004, #40800 ) ) ;
#47854 = EDGE_CURVE ( 'NONE', #43377, #26074, #6881, .T. ) ;
#47855 = AXIS2_PLACEMENT_3D ( 'NONE', #40921, #37241, #44826 ) ;
#47856 = DIRECTION ( 'NONE',  ( 0.000000000000000000, 0.000000000000000000, 1.000000000000000000 ) ) ;
#47857 = CARTESIAN_POINT ( 'NONE',  ( 11.99999999999999822, 77.19088730480524418, 6.903761155838049390 ) ) ;
#47858 = VECTOR ( 'NONE', #20019, 1000.000000000000000 ) ;
#47860 = ORIENTED_EDGE ( 'NONE', *, *, #8776, .F. ) ;
#47859 = CARTESIAN_POINT ( 'NONE',  ( 5.000000000000002665, -29.01471420065617224, 76.69515212746007649 ) ) ;
#47861 = ORIENTED_EDGE ( 'NONE', *, *, #46239, .T. ) ;
#47862 = DIRECTION ( 'NONE',  ( -1.000000000000000000, -0.000000000000000000, -0.000000000000000000 ) ) ;
#47863 = ORIENTED_EDGE ( 'NONE', *, *, #18890, .F. ) ;
#47864 = CIRCLE ( 'NONE', #36134, 31.99999999999998579 ) ;
#47865 = VERTEX_POINT ( 'NONE', #30018 ) ;
#47866 = DIRECTION ( 'NONE',  ( -1.000000000000000000, 0.000000000000000000, -0.000000000000000000 ) ) ;
#47868 = ORIENTED_EDGE ( 'NONE', *, *, #19034, .T. ) ;
#47867 = CARTESIAN_POINT ( 'NONE',  ( 0.000000000000000000, -37.58145647212453611, -0.6853352020794456489 ) ) ;
#47869 = EDGE_CURVE ( 'NONE', #23071, #35415, #41283, .T. ) ;
#47870 = CARTESIAN_POINT ( 'NONE',  ( -7.001685179585692254, -14.98378029539707512, 0.000000000000000000 ) ) ;
#47871 = ORIENTED_EDGE ( 'NONE', *, *, #47564, .T. ) ;
#47872 = VECTOR ( 'NONE', #30501, 1000.000000000000000 ) ;
#47873 = VERTEX_POINT ( 'NONE', #40790 ) ;
#47874 = VERTEX_POINT ( 'NONE', #14122 ) ;
#47875 = DIRECTION ( 'NONE',  ( -1.000000000000000000, 0.000000000000000000, 0.000000000000000000 ) ) ;
#47876 = VERTEX_POINT ( 'NONE', #7738 ) ;
#47877 = CARTESIAN_POINT ( 'NONE',  ( 5.000000000000000000, -39.04073710021332744, -15.48615015657624205 ) ) ;
#47878 = VECTOR ( 'NONE', #42035, 1000.000000000000000 ) ;
#47879 = DIRECTION ( 'NONE',  ( 1.000000000000000000, -0.000000000000000000, -0.000000000000000000 ) ) ;
#47880 = CARTESIAN_POINT ( 'NONE',  ( 10.00000000000000000, -73.95703589263990807, 23.16143007188399139 ) ) ;
#47881 = ORIENTED_EDGE ( 'NONE', *, *, #15046, .T. ) ;
#47882 = DIRECTION ( 'NONE',  ( -1.000000000000000000, -0.000000000000000000, 0.000000000000000000 ) ) ;
#47883 = FACE_OUTER_BOUND ( 'NONE', #18340, .T. ) ;
#47884 = CARTESIAN_POINT ( 'NONE',  ( -6.880223345695647197, -142.5202692415819854, -5.500000000000000000 ) ) ;
#47885 = DIRECTION ( 'NONE',  ( -1.000000000000000000, 0.000000000000000000, -0.000000000000000000 ) ) ;
#47886 = DIRECTION ( 'NONE',  ( 1.000000000000000000, 0.000000000000000000, 0.000000000000000000 ) ) ;
#47887 = ORIENTED_EDGE ( 'NONE', *, *, #36519, .T. ) ;
#47888 = ADVANCED_FACE ( 'NONE', ( #48369 ), #7509, .T. ) ;
#47889 = LINE ( 'NONE', #44239, #24893 ) ;
#47890 = AXIS2_PLACEMENT_3D ( 'NONE', #32312, #31365, #17359 ) ;
#47891 = EDGE_CURVE ( 'NONE', #21969, #46126, #26428, .T. ) ;
#47892 = CARTESIAN_POINT ( 'NONE',  ( 0.000000000000000000, 37.16516213103285082, -4.992566952384588141 ) ) ;
#47893 = CYLINDRICAL_SURFACE ( 'NONE', #31402, 42.00000000000000000 ) ;
#47894 = DIRECTION ( 'NONE',  ( 1.000000000000000000, 0.000000000000000000, 0.000000000000000000 ) ) ;
#47895 = EDGE_CURVE ( 'NONE', #31027, #14287, #23385, .T. ) ;
#47896 = CARTESIAN_POINT ( 'NONE',  ( 11.99999999999999822, 77.16300072079661732, 27.74655509720698277 ) ) ;
#47898 = AXIS2_PLACEMENT_3D ( 'NONE', #2223, #10282, #32786 ) ;
#47897 = DIRECTION ( 'NONE',  ( -1.000000000000000000, 0.000000000000000000, 0.000000000000000000 ) ) ;
#47899 = AXIS2_PLACEMENT_3D ( 'NONE', #1254, #23035, #34046 ) ;
#47900 = CARTESIAN_POINT ( 'NONE',  ( 0.000000000000000000, -36.13751322684434797, 21.40280677340357940 ) ) ;
#47901 = FACE_OUTER_BOUND ( 'NONE', #43987, .T. ) ;
#47902 = EDGE_CURVE ( 'NONE', #37588, #18992, #12380, .T. ) ;
#47903 = VECTOR ( 'NONE', #8464, 1000.000000000000000 ) ;
#47904 = LINE ( 'NONE', #7034, #42531 ) ;
#47905 = PRESENTATION_STYLE_ASSIGNMENT (( #25875 ) ) ;
#47906 = CIRCLE ( 'NONE', #30733, 31.99999999999998224 ) ;
#47907 = CARTESIAN_POINT ( 'NONE',  ( 10.00000000000000000, 0.000000000000000000, 0.000000000000000000 ) ) ;
#47908 = EDGE_LOOP ( 'NONE', ( #13521, #29673, #13592, #40990 ) ) ;
#47909 = ORIENTED_EDGE ( 'NONE', *, *, #16082, .T. ) ;
#47910 = CIRCLE ( 'NONE', #47150, 31.99999999999999289 ) ;
#47911 = ORIENTED_EDGE ( 'NONE', *, *, #19450, .F. ) ;
#47912 = VECTOR ( 'NONE', #20904, 1000.000000000000000 ) ;
#47913 = CARTESIAN_POINT ( 'NONE',  ( 0.000000000000000000, -74.65491531819111515, -8.830959090343204920 ) ) ;
#47914 = FACE_OUTER_BOUND ( 'NONE', #6284, .T. ) ;
#47915 = ORIENTED_EDGE ( 'NONE', *, *, #40316, .T. ) ;
#47916 = EDGE_CURVE ( 'NONE', #43886, #36733, #15565, .T. ) ;
#47917 = PLANE ( 'NONE',  #1489 ) ;
#47918 = ORIENTED_EDGE ( 'NONE', *, *, #5262, .F. ) ;
#47919 = AXIS2_PLACEMENT_3D ( 'NONE', #27959, #23537, #38475 ) ;
#47920 = ADVANCED_FACE ( 'NONE', ( #16060 ), #8460, .T. ) ;
#47921 = AXIS2_PLACEMENT_3D ( 'NONE', #29119, #25680, #44536 ) ;
#47922 = EDGE_CURVE ( 'NONE', #22545, #20106, #38324, .T. ) ;
#47923 = CARTESIAN_POINT ( 'NONE',  ( 10.00000000000000000, -21.40280677340345505, -36.13751322684441902 ) ) ;
#47924 = EDGE_LOOP ( 'NONE', ( #45087, #9924, #13526, #28333 ) ) ;
#47925 = FACE_OUTER_BOUND ( 'NONE', #23429, .T. ) ;
#47926 = ORIENTED_EDGE ( 'NONE', *, *, #193, .T. ) ;
#47927 = FACE_OUTER_BOUND ( 'NONE', #47508, .T. ) ;
#47928 = AXIS2_PLACEMENT_3D ( 'NONE', #27812, #42736, #24126 ) ;
#47929 = AXIS2_PLACEMENT_3D ( 'NONE', #5344, #43264, #12935 ) ;
#47930 = AXIS2_PLACEMENT_3D ( 'NONE', #22690, #41079, #18043 ) ;
#47931 = FACE_OUTER_BOUND ( 'NONE', #29585, .T. ) ;
#47932 = CARTESIAN_POINT ( 'NONE',  ( 10.00000000000000000, 17.67226234102826510, 33.17418723428314564 ) ) ;
#47933 = VECTOR ( 'NONE', #15583, 1000.000000000000000 ) ;
#47934 = ORIENTED_EDGE ( 'NONE', *, *, #6454, .T. ) ;
#47935 = ORIENTED_EDGE ( 'NONE', *, *, #38407, .F. ) ;
#47936 = LINE ( 'NONE', #28638, #4 ) ;
#47937 = DIRECTION ( 'NONE',  ( -1.000000000000000000, 0.000000000000000000, 0.000000000000000000 ) ) ;
#47938 = AXIS2_PLACEMENT_3D ( 'NONE', #13750, #13499, #9107 ) ;
#47939 = CIRCLE ( 'NONE', #29995, 77.49899999999999523 ) ;
#47940 = EDGE_LOOP ( 'NONE', ( #38084, #45298, #27068, #8807 ) ) ;
#47941 = ORIENTED_EDGE ( 'NONE', *, *, #24413, .T. ) ;
#47942 = AXIS2_PLACEMENT_3D ( 'NONE', #23514, #42130, #998 ) ;
#47943 = EDGE_CURVE ( 'NONE', #11046, #38237, #45958, .T. ) ;
#47944 = FACE_OUTER_BOUND ( 'NONE', #613, .T. ) ;
#47945 = DIRECTION ( 'NONE',  ( 0.000000000000000000, 0.000000000000000000, -1.000000000000000000 ) ) ;
#47946 = ORIENTED_EDGE ( 'NONE', *, *, #35791, .T. ) ;
#47947 = ORIENTED_EDGE ( 'NONE', *, *, #30116, .T. ) ;
#47948 = CIRCLE ( 'NONE', #11207, 32.00000000000000000 ) ;
#47949 = CARTESIAN_POINT ( 'NONE',  ( -14.87942725330654348, -141.9795960975983178, -5.500000000000000000 ) ) ;
#47950 = FACE_OUTER_BOUND ( 'NONE', #37998, .T. ) ;
#47951 = DIRECTION ( 'NONE',  ( 0.000000000000000000, 0.000000000000000000, -1.000000000000000000 ) ) ;
#47952 = ADVANCED_FACE ( 'NONE', ( #37598 ), #4554, .T. ) ;
#47953 = LINE ( 'NONE', #21768, #15846 ) ;
#47954 = FACE_OUTER_BOUND ( 'NONE', #37457, .T. ) ;
#47955 = AXIS2_PLACEMENT_3D ( 'NONE', #37450, #15187, #8063 ) ;
#47956 = CARTESIAN_POINT ( 'NONE',  ( 22.94323693612312809, -114.6983135802921083, -5.500000000000000000 ) ) ;
#47957 = FACE_OUTER_BOUND ( 'NONE', #19403, .T. ) ;
#47958 = CARTESIAN_POINT ( 'NONE',  ( 10.00000000000000000, -72.35160999960831418, 20.41045688087797672 ) ) ;
#47959 = EDGE_CURVE ( 'NONE', #37233, #28726, #13143, .T. ) ;
#47960 = EDGE_CURVE ( 'NONE', #46530, #43176, #46767, .T. ) ;
#47961 = CARTESIAN_POINT ( 'NONE',  ( 9.984461079971730157, -95.40710393340120277, 5.500000000000000000 ) ) ;
#47962 = DIRECTION ( 'NONE',  ( -0.3311129884571281101, -0.9435911131814402886, 0.000000000000000000 ) ) ;
#47963 = SURFACE_STYLE_FILL_AREA ( #40872 ) ;
#47964 = DIRECTION ( 'NONE',  ( 0.000000000000000000, -0.9945218953682730678, -0.1045284632676570929 ) ) ;
#47965 = EDGE_LOOP ( 'NONE', ( #3578, #33185 ) ) ;
#47966 = CIRCLE ( 'NONE', #22952, 31.99999999999999289 ) ;
#47967 = VERTEX_POINT ( 'NONE', #4792 ) ;
#47968 = ORIENTED_EDGE ( 'NONE', *, *, #47119, .T. ) ;
#47969 = AXIS2_PLACEMENT_3D ( 'NONE', #7388, #17421, #43864 ) ;
#47970 = DIRECTION ( 'NONE',  ( 0.9781476007338069101, 2.546183866652752180E-17, 0.2079116908177528755 ) ) ;
#47971 = CIRCLE ( 'NONE', #26887, 42.00000000000000000 ) ;
#47972 = VECTOR ( 'NONE', #19664, 1000.000000000000000 ) ;
#47973 = LINE ( 'NONE', #44068, #27667 ) ;
#47974 = ORIENTED_EDGE ( 'NONE', *, *, #29855, .F. ) ;
#47975 = ORIENTED_EDGE ( 'NONE', *, *, #42945, .T. ) ;
#47976 = CIRCLE ( 'NONE', #8920, 31.99999999999999289 ) ;
#47977 = AXIS2_PLACEMENT_3D ( 'NONE', #32849, #43, #47778 ) ;
#47978 = VECTOR ( 'NONE', #1444, 1000.000000000000114 ) ;
#47979 = LINE ( 'NONE', #14707, #12422 ) ;
#47980 = CIRCLE ( 'NONE', #20640, 31.99999999999999289 ) ;
#47981 = VECTOR ( 'NONE', #43462, 1000.000000000000000 ) ;
#47982 = ORIENTED_EDGE ( 'NONE', *, *, #35139, .T. ) ;
#47983 = CARTESIAN_POINT ( 'NONE',  ( 11.99999999999999822, 77.49459641780886443, 0.8261519478433866359 ) ) ;
#47984 = ORIENTED_EDGE ( 'NONE', *, *, #17936, .F. ) ;
#47985 = DIRECTION ( 'NONE',  ( 0.000000000000000000, 0.000000000000000000, 1.000000000000000000 ) ) ;
#47986 = VECTOR ( 'NONE', #11356, 1000.000000000000000 ) ;
#47987 = DIRECTION ( 'NONE',  ( -1.000000000000000000, -0.000000000000000000, 0.000000000000000000 ) ) ;
#47988 = ORIENTED_EDGE ( 'NONE', *, *, #17092, .F. ) ;
#47989 = ORIENTED_EDGE ( 'NONE', *, *, #20324, .F. ) ;
#47990 = FACE_OUTER_BOUND ( 'NONE', #11456, .T. ) ;
#47991 = ADVANCED_FACE ( 'NONE', ( #11657 ), #42480, .F. ) ;
#47992 = ORIENTED_EDGE ( 'NONE', *, *, #36461, .F. ) ;
#47993 = DIRECTION ( 'NONE',  ( 0.000000000000000000, 0.000000000000000000, 1.000000000000000000 ) ) ;
#47994 = DIRECTION ( 'NONE',  ( 0.000000000000000000, -0.3826834323650772363, -0.9238795325112919565 ) ) ;
#47995 = ORIENTED_EDGE ( 'NONE', *, *, #37639, .F. ) ;
#47996 = LINE ( 'NONE', #45979, #1833 ) ;
#47997 = DIRECTION ( 'NONE',  ( 0.000000000000000000, 0.9238795325112851842, 0.3826834323650937786 ) ) ;
#47998 = CARTESIAN_POINT ( 'NONE',  ( 10.00000000000000000, -63.18004540533059554, 44.88180994100355292 ) ) ;
#47999 = CYLINDRICAL_SURFACE ( 'NONE', #5547, 31.99999999999998579 ) ;
#48000 = ORIENTED_EDGE ( 'NONE', *, *, #46558, .T. ) ;
#48001 = CARTESIAN_POINT ( 'NONE',  ( 10.00000000000000000, 39.78640506895604290, 66.50666863322015843 ) ) ;
#48002 = VERTEX_POINT ( 'NONE', #15344 ) ;
#48003 = ORIENTED_EDGE ( 'NONE', *, *, #18505, .T. ) ;
#48004 = DIRECTION ( 'NONE',  ( 0.000000000000000000, -1.000000000000000000, -2.312964634635746211E-15 ) ) ;
#48005 = CIRCLE ( 'NONE', #8915, 31.99999999999998579 ) ;
#48006 = CARTESIAN_POINT ( 'NONE',  ( 10.00000000000000000, 55.19960302592141232, -51.03279382321027668 ) ) ;
#48007 = VECTOR ( 'NONE', #40945, 1000.000000000000000 ) ;
#48008 = CARTESIAN_POINT ( 'NONE',  ( 0.000000000000000000, -55.16347631943085617, 60.67117009219117563 ) ) ;
#48009 = EDGE_LOOP ( 'NONE', ( #21629, #8005, #37208, #45780 ) ) ;
#48010 = DIRECTION ( 'NONE',  ( 0.000000000000000000, -0.9238795325112821866, -0.3826834323651006065 ) ) ;
#48011 = CARTESIAN_POINT ( 'NONE',  ( -3.000000000000002665, 0.000000000000000000, 0.000000000000000000 ) ) ;
#48012 = EDGE_LOOP ( 'NONE', ( #36742, #1177, #41016, #46679 ) ) ;
#48013 = AXIS2_PLACEMENT_3D ( 'NONE', #34561, #42903, #19630 ) ;
#48014 = EDGE_CURVE ( 'NONE', #28097, #9186, #18981, .T. ) ;
#48015 = LINE ( 'NONE', #21347, #45285 ) ;
#48016 = EDGE_CURVE ( 'NONE', #11149, #15029, #37350, .T. ) ;
#48017 = ADVANCED_FACE ( 'NONE', ( #397 ), #4072, .F. ) ;
#48018 = DIRECTION ( 'NONE',  ( 1.000000000000000000, 0.000000000000000000, 0.000000000000000000 ) ) ;
#48019 = CARTESIAN_POINT ( 'NONE',  ( 5.000000000000000000, -22.48208911017525580, 35.47612816024516036 ) ) ;
#48020 = EDGE_LOOP ( 'NONE', ( #14605, #37215, #803, #22945 ) ) ;
#48021 = AXIS2_PLACEMENT_3D ( 'NONE', #31217, #34149, #23371 ) ;
#48022 = VECTOR ( 'NONE', #28880, 1000.000000000000000 ) ;
#48023 = DIRECTION ( 'NONE',  ( -1.000000000000000000, 0.000000000000000000, 0.000000000000000000 ) ) ;
#48024 = DIRECTION ( 'NONE',  ( -1.000000000000000000, 0.000000000000000000, 0.000000000000000000 ) ) ;
#48025 = CARTESIAN_POINT ( 'NONE',  ( 30.50000000000000000, -120.0000000000000000, 5.500000000000000888 ) ) ;
#48027 = AXIS2_PLACEMENT_3D ( 'NONE', #43991, #17560, #6318 ) ;
#48026 = LINE ( 'NONE', #36048, #41137 ) ;
#48028 = EDGE_CURVE ( 'NONE', #35932, #16941, #28790, .T. ) ;
#48029 = AXIS2_PLACEMENT_3D ( 'NONE', #18051, #40360, #14402 ) ;
#48030 = ADVANCED_FACE ( 'NONE', ( #34888 ), #27317, .T. ) ;
#48031 = CYLINDRICAL_SURFACE ( 'NONE', #36914, 42.00000000000000000 ) ;
#48032 = CYLINDRICAL_SURFACE ( 'NONE', #22971, 77.49899999999999523 ) ;
#48033 = DIRECTION ( 'NONE',  ( -1.000000000000000000, -0.000000000000000000, 0.000000000000000000 ) ) ;
#48034 = CYLINDRICAL_SURFACE ( 'NONE', #38975, 37.49900000000000233 ) ;
#48035 = VECTOR ( 'NONE', #30026, 1000.000000000000000 ) ;
#48036 = ORIENTED_EDGE ( 'NONE', *, *, #38190, .T. ) ;
#48037 = FACE_OUTER_BOUND ( 'NONE', #6416, .T. ) ;
#48038 = ORIENTED_EDGE ( 'NONE', *, *, #12501, .F. ) ;
#48039 = DIRECTION ( 'NONE',  ( -0.9038112904824853189, 0.4279312458752977943, 0.000000000000000000 ) ) ;
#48040 =( LENGTH_UNIT ( ) NAMED_UNIT ( * ) SI_UNIT ( .MILLI., .METRE. ) );
#48041 = CARTESIAN_POINT ( 'NONE',  ( 7.543218489614351263, -11.91259227951415056, 0.000000000000000000 ) ) ;
#48042 = ORIENTED_EDGE ( 'NONE', *, *, #6046, .F. ) ;
#48043 = EDGE_CURVE ( 'NONE', #44937, #24691, #16297, .T. ) ;
#48044 = CIRCLE ( 'NONE', #16019, 31.99999999999999645 ) ;
#48045 = CIRCLE ( 'NONE', #43349, 82.00000000000000000 ) ;
#48046 = VECTOR ( 'NONE', #50, 1000.000000000000114 ) ;
#48047 = DIRECTION ( 'NONE',  ( -1.000000000000000000, -0.000000000000000000, 0.000000000000000000 ) ) ;
#48048 = VERTEX_POINT ( 'NONE', #31235 ) ;
#48049 = EDGE_CURVE ( 'NONE', #39824, #43844, #46157, .T. ) ;
#48050 = EDGE_CURVE ( 'NONE', #43965, #9118, #37390, .T. ) ;
#48051 = CIRCLE ( 'NONE', #46538, 77.49899999999999523 ) ;
#48052 = AXIS2_PLACEMENT_3D ( 'NONE', #43703, #20954, #39806 ) ;
#48053 = CYLINDRICAL_SURFACE ( 'NONE', #43296, 16.00000000000000000 ) ;
#48054 = ORIENTED_EDGE ( 'NONE', *, *, #26483, .F. ) ;
#48055 = AXIS2_PLACEMENT_3D ( 'NONE', #28228, #41535, #16310 ) ;
#48056 = CARTESIAN_POINT ( 'NONE',  ( 0.000000000000000000, 0.000000000000000000, 37.49900000000000233 ) ) ;
#48057 = FACE_OUTER_BOUND ( 'NONE', #6832, .T. ) ;
#48058 = ADVANCED_FACE ( 'NONE', ( #25749 ), #10606, .T. ) ;
#48059 = VERTEX_POINT ( 'NONE', #21618 ) ;
#48060 = CARTESIAN_POINT ( 'NONE',  ( 0.000000000000000000, 0.000000000000000000, 0.000000000000000000 ) ) ;
#48061 = VECTOR ( 'NONE', #40669, 1000.000000000000000 ) ;
#48062 = ADVANCED_FACE ( 'NONE', ( #44369 ), #14265, .T. ) ;
#48063 = VERTEX_POINT ( 'NONE', #6924 ) ;
#48064 = AXIS2_PLACEMENT_3D ( 'NONE', #9195, #42241, #20439 ) ;
#48065 = AXIS2_PLACEMENT_3D ( 'NONE', #9, #44087, #40654 ) ;
#48066 = DIRECTION ( 'NONE',  ( 0.000000000000000000, 0.5877852522924683631, 0.8090169943749510040 ) ) ;
#48067 = CARTESIAN_POINT ( 'NONE',  ( -10.90076147243505211, 0.000000000000000000, 13.71319123027096865 ) ) ;
#48068 = LINE ( 'NONE', #39776, #28241 ) ;
#48069 = FACE_OUTER_BOUND ( 'NONE', #33481, .T. ) ;
#48070 = ORIENTED_EDGE ( 'NONE', *, *, #19942, .T. ) ;
#48071 = CARTESIAN_POINT ( 'NONE',  ( 0.000000000000000000, 22.74946021919133088, 29.81001611431016229 ) ) ;
#48072 = ORIENTED_EDGE ( 'NONE', *, *, #20660, .F. ) ;
#48073 = ORIENTED_EDGE ( 'NONE', *, *, #5597, .T. ) ;
#48074 = FACE_OUTER_BOUND ( 'NONE', #25687, .T. ) ;
#48075 = CARTESIAN_POINT ( 'NONE',  ( 5.000000000000000000, -22.48208911017474065, -35.47612816024548721 ) ) ;
#48076 = CARTESIAN_POINT ( 'NONE',  ( 10.00000000000000000, -33.00180498840035170, -17.80606268964575278 ) ) ;
#48077 = FACE_OUTER_BOUND ( 'NONE', #48278, .T. ) ;
#48078 = ORIENTED_EDGE ( 'NONE', *, *, #18560, .F. ) ;
#48079 = DIRECTION ( 'NONE',  ( -1.000000000000000000, 0.000000000000000000, -0.000000000000000000 ) ) ;
#48080 = FACE_OUTER_BOUND ( 'NONE', #38878, .T. ) ;
#48081 = EDGE_CURVE ( 'NONE', #43442, #33302, #3730, .T. ) ;
#48082 = EDGE_CURVE ( 'NONE', #42057, #33952, #666, .T. ) ;
#48083 = LINE ( 'NONE', #40993, #44621 ) ;
#48084 = CARTESIAN_POINT ( 'NONE',  ( 15.00000000000000000, -19.89357724624986545, 12.59942793731086219 ) ) ;
#48085 = AXIS2_PLACEMENT_3D ( 'NONE', #28716, #47068, #31926 ) ;
#48086 = FACE_OUTER_BOUND ( 'NONE', #26959, .T. ) ;
#48087 = ORIENTED_EDGE ( 'NONE', *, *, #35646, .T. ) ;
#48088 = DIRECTION ( 'NONE',  ( -1.000000000000000000, 0.000000000000000000, -0.000000000000000000 ) ) ;
#48089 = DIRECTION ( 'NONE',  ( -1.000000000000000000, 0.000000000000000000, 0.000000000000000000 ) ) ;
#48090 = CIRCLE ( 'NONE', #37111, 31.99999999999998579 ) ;
#48091 = CARTESIAN_POINT ( 'NONE',  ( 0.000000000000000000, 23.50000000000000000, -1.500000000000001332 ) ) ;
#48092 = CARTESIAN_POINT ( 'NONE',  ( 10.00000000000000000, 0.000000000000000000, 0.000000000000000000 ) ) ;
#48093 = CARTESIAN_POINT ( 'NONE',  ( 10.00000000000000000, 0.000000000000000000, 0.000000000000000000 ) ) ;
#48094 = EDGE_CURVE ( 'NONE', #6805, #29267, #48348, .T. ) ;
#48095 = AXIS2_PLACEMENT_3D ( 'NONE', #45852, #8388, #27005 ) ;
#48096 = AXIS2_PLACEMENT_3D ( 'NONE', #14288, #34998, #27428 ) ;
#48097 = DIRECTION ( 'NONE',  ( 0.000000000000000000, 1.000000000000000000, 3.469446951953614189E-15 ) ) ;
#48098 = DIRECTION ( 'NONE',  ( 1.000000000000000000, 0.000000000000000000, 0.000000000000000000 ) ) ;
#48099 = ORIENTED_EDGE ( 'NONE', *, *, #47087, .F. ) ;
#48100 = DIRECTION ( 'NONE',  ( -0.000000000000000000, -0.000000000000000000, -1.000000000000000000 ) ) ;
#48101 = AXIS2_PLACEMENT_3D ( 'NONE', #9079, #31366, #32082 ) ;
#48102 = DIRECTION ( 'NONE',  ( -1.000000000000000000, -0.000000000000000000, -0.000000000000000000 ) ) ;
#48103 = AXIS2_PLACEMENT_3D ( 'NONE', #20932, #20684, #6244 ) ;
#48104 = AXIS2_PLACEMENT_3D ( 'NONE', #25173, #47462, #40844 ) ;
#48105 = ORIENTED_EDGE ( 'NONE', *, *, #11111, .F. ) ;
#48106 = ORIENTED_EDGE ( 'NONE', *, *, #32452, .F. ) ;
#48107 = AXIS2_PLACEMENT_3D ( 'NONE', #35930, #28115, #24918 ) ;
#48108 = DIRECTION ( 'NONE',  ( -1.000000000000000000, 0.000000000000000000, 0.000000000000000000 ) ) ;
#48109 = EDGE_LOOP ( 'NONE', ( #6508, #16900, #10628 ) ) ;
#48110 = ORIENTED_EDGE ( 'NONE', *, *, #40964, .T. ) ;
#48111 = AXIS2_PLACEMENT_3D ( 'NONE', #31132, #41187, #30636 ) ;
#48112 = EDGE_CURVE ( 'NONE', #20812, #2760, #33496, .T. ) ;
#48113 = LINE ( 'NONE', #14599, #25366 ) ;
#48114 = CARTESIAN_POINT ( 'NONE',  ( 10.00000000000000000, -40.68715046381921496, -10.41901085202121457 ) ) ;
#48115 = CARTESIAN_POINT ( 'NONE',  ( 11.99999999999999822, 0.000000000000000000, 0.000000000000000000 ) ) ;
#48116 = EDGE_CURVE ( 'NONE', #17971, #37535, #36767, .T. ) ;
#48117 = ORIENTED_EDGE ( 'NONE', *, *, #36676, .T. ) ;
#48118 = CARTESIAN_POINT ( 'NONE',  ( 0.000000000000000000, 0.000000000000000000, 0.000000000000000000 ) ) ;
#48119 = ORIENTED_EDGE ( 'NONE', *, *, #18616, .F. ) ;
#48120 = EDGE_LOOP ( 'NONE', ( #28856, #44404, #29777, #25300 ) ) ;
#48121 = EDGE_CURVE ( 'NONE', #48217, #6313, #41313, .T. ) ;
#48122 = ORIENTED_EDGE ( 'NONE', *, *, #31903, .T. ) ;
#48123 = DIRECTION ( 'NONE',  ( -0.9918136447140101231, 0.1276937514489694114, 0.000000000000000000 ) ) ;
#48124 = DIRECTION ( 'NONE',  ( 0.000000000000000000, -0.000000000000000000, 1.000000000000000000 ) ) ;
#48125 = CYLINDRICAL_SURFACE ( 'NONE', #1698, 37.49900000000000233 ) ;
#48126 = VECTOR ( 'NONE', #36671, 1000.000000000000000 ) ;
#48127 = VERTEX_POINT ( 'NONE', #25515 ) ;
#48128 = VERTEX_POINT ( 'NONE', #37502 ) ;
#48129 = CARTESIAN_POINT ( 'NONE',  ( 10.00000000000000000, 0.000000000000000000, 0.000000000000000000 ) ) ;
#48130 = ORIENTED_EDGE ( 'NONE', *, *, #39640, .F. ) ;
#48131 = DIRECTION ( 'NONE',  ( -1.000000000000000000, 0.000000000000000000, -0.000000000000000000 ) ) ;
#48132 = DIRECTION ( 'NONE',  ( 1.000000000000000000, -0.000000000000000000, -0.000000000000000000 ) ) ;
#48133 = LINE ( 'NONE', #14620, #26039 ) ;
#48134 = CARTESIAN_POINT ( 'NONE',  ( 10.00000000000000000, -22.74946021919110706, -29.81001611431033282 ) ) ;
#48135 = CARTESIAN_POINT ( 'NONE',  ( 10.00000000000000000, -68.26794271651239399, -31.47745569255214093 ) ) ;
#48136 = CIRCLE ( 'NONE', #27051, 12.50000000000000000 ) ;
#48137 = DIRECTION ( 'NONE',  ( -0.000000000000000000, 0.5000000000000019984, 0.8660254037844374864 ) ) ;
#48138 = EDGE_CURVE ( 'NONE', #19466, #25524, #14757, .T. ) ;
#48139 = EDGE_CURVE ( 'NONE', #36422, #7117, #18884, .T. ) ;
#48140 = CARTESIAN_POINT ( 'NONE',  ( 11.99999999999999822, -59.75363087400035056, -56.15606465355020305 ) ) ;
#48141 = CARTESIAN_POINT ( 'NONE',  ( 10.00000000000000000, -22.64427369931191336, 30.00120703465197280 ) ) ;
#48142 = LINE ( 'NONE', #7018, #905 ) ;
#48143 = ORIENTED_EDGE ( 'NONE', *, *, #29339, .T. ) ;
#48144 = CLOSED_SHELL ( 'NONE', ( #18446, #9490, #36466, #29644, #43596, #47276, #47726, #39076, #5384, #3624, #17283, #18283, #32338, #34578, #39795, #46140, #30280, #40163, #10723, #30348, #40424, #47176, #43283, #30857, #23169, #45968, #19600, #7226, #40775, #34935, #15912, #3054, #4646, #29116, #2730 ) ) ;
#48145 = EDGE_CURVE ( 'NONE', #41319, #18807, #3233, .T. ) ;
#48146 = DIRECTION ( 'NONE',  ( 0.000000000000000000, 0.1564344650402244019, 0.9876883405951387696 ) ) ;
#48147 = CARTESIAN_POINT ( 'NONE',  ( 10.00000000000000000, 75.11764819372149304, 29.05362095685338986 ) ) ;
#48148 = AXIS2_PLACEMENT_3D ( 'NONE', #4463, #541, #23294 ) ;
#48149 = CARTESIAN_POINT ( 'NONE',  ( 0.000000000000000000, -79.10210256391353312, -21.60688246758670061 ) ) ;
#48150 = CARTESIAN_POINT ( 'NONE',  ( 0.000000000000000000, 0.000000000000000000, -54.99999999999998579 ) ) ;
#48151 = CIRCLE ( 'NONE', #5151, 31.99999999999998579 ) ;
#48152 = DIRECTION ( 'NONE',  ( 0.000000000000000000, 0.000000000000000000, 1.000000000000000000 ) ) ;
#48153 = DIRECTION ( 'NONE',  ( -0.000000000000000000, -0.000000000000000000, -1.000000000000000000 ) ) ;
#48154 = ADVANCED_FACE ( 'NONE', ( #14022 ), #48034, .T. ) ;
#48155 = AXIS2_PLACEMENT_3D ( 'NONE', #11009, #44054, #13953 ) ;
#48156 = ORIENTED_EDGE ( 'NONE', *, *, #27736, .F. ) ;
#48157 = DIRECTION ( 'NONE',  ( -0.9435911131814402886, 0.3311129884571281101, 0.000000000000000000 ) ) ;
#48158 = CARTESIAN_POINT ( 'NONE',  ( 10.00000000000000000, -51.29473840253178452, -63.97538442413483750 ) ) ;
#48159 = DIRECTION ( 'NONE',  ( 0.000000000000000000, 1.000000000000000000, 3.469446951953614189E-15 ) ) ;
#48160 = CIRCLE ( 'NONE', #5979, 37.49900000000000944 ) ;
#48161 = DIRECTION ( 'NONE',  ( 0.000000000000000000, 0.000000000000000000, 1.000000000000000000 ) ) ;
#48162 = EDGE_LOOP ( 'NONE', ( #33787, #20079, #18966, #8104 ) ) ;
#48163 = CIRCLE ( 'NONE', #1288, 77.49899999999999523 ) ;
#48164 = EDGE_LOOP ( 'NONE', ( #32006, #37706, #38702, #43297 ) ) ;
#48165 = AXIS2_PLACEMENT_3D ( 'NONE', #2752, #36042, #47067 ) ;
#48166 = CARTESIAN_POINT ( 'NONE',  ( 10.00000000000000000, 0.000000000000000000, 0.000000000000000000 ) ) ;
#48167 = CARTESIAN_POINT ( 'NONE',  ( 0.000000000000000000, 27.75498641678742473, 31.52238457039609187 ) ) ;
#48168 = ORIENTED_EDGE ( 'NONE', *, *, #37134, .F. ) ;
#48169 = VERTEX_POINT ( 'NONE', #40691 ) ;
#48170 = VECTOR ( 'NONE', #29968, 1000.000000000000000 ) ;
#48171 = CIRCLE ( 'NONE', #31013, 16.00000000000000000 ) ;
#48172 = CARTESIAN_POINT ( 'NONE',  ( 10.00000000000000000, -37.22597642581153821, 10.79786254984320415 ) ) ;
#48173 = EDGE_CURVE ( 'NONE', #24574, #19822, #29442, .T. ) ;
#48174 = ORIENTED_EDGE ( 'NONE', *, *, #10966, .F. ) ;
#48175 = AXIS2_PLACEMENT_3D ( 'NONE', #16201, #38724, #24743 ) ;
#48176 = ORIENTED_EDGE ( 'NONE', *, *, #26791, .F. ) ;
#48177 = EDGE_CURVE ( 'NONE', #14712, #19563, #28945, .T. ) ;
#48178 = EDGE_CURVE ( 'NONE', #34100, #43888, #45224, .T. ) ;
#48179 = VECTOR ( 'NONE', #40095, 1000.000000000000000 ) ;
#48180 = EDGE_CURVE ( 'NONE', #22636, #27232, #28035, .T. ) ;
#48181 = CARTESIAN_POINT ( 'NONE',  ( 0.000000000000000000, -27.74655509720617985, -77.16300072079690153 ) ) ;
#48182 = ORIENTED_EDGE ( 'NONE', *, *, #36034, .F. ) ;
#48183 = DIRECTION ( 'NONE',  ( 0.000000000000000000, -0.5224985647159561264, 0.8526401643540878483 ) ) ;
#48184 = EDGE_CURVE ( 'NONE', #29406, #26733, #33583, .T. ) ;
#48185 = ORIENTED_EDGE ( 'NONE', *, *, #6966, .T. ) ;
#48186 = DIRECTION ( 'NONE',  ( 1.000000000000000000, 0.000000000000000000, 0.000000000000000000 ) ) ;
#48187 = CARTESIAN_POINT ( 'NONE',  ( 10.00000000000000000, 71.91182617369189245, 28.89263327155772743 ) ) ;
#48188 = DIRECTION ( 'NONE',  ( 0.000000000000000000, 0.9723699203976756689, 0.2334453638559095823 ) ) ;
#48189 = EDGE_LOOP ( 'NONE', ( #10235, #6817, #44518, #20524 ) ) ;
#48190 = ORIENTED_EDGE ( 'NONE', *, *, #37463, .F. ) ;
#48191 = EDGE_CURVE ( 'NONE', #11246, #40230, #3001, .T. ) ;
#48192 = CARTESIAN_POINT ( 'NONE',  ( 10.00000000000000000, 46.54456581323888997, -59.03342792756214408 ) ) ;
#48193 = CARTESIAN_POINT ( 'NONE',  ( 10.00000000000000000, 0.000000000000000000, 0.000000000000000000 ) ) ;
#48194 = VERTEX_POINT ( 'NONE', #23777 ) ;
#48195 = VERTEX_POINT ( 'NONE', #41919 ) ;
#48196 = EDGE_CURVE ( 'NONE', #34129, #27354, #8592, .T. ) ;
#48197 = CARTESIAN_POINT ( 'NONE',  ( 11.99999999999999822, 0.000000000000000000, 0.000000000000000000 ) ) ;
#48198 = DIRECTION ( 'NONE',  ( -1.000000000000000000, 0.000000000000000000, 0.000000000000000000 ) ) ;
#48199 = ORIENTED_EDGE ( 'NONE', *, *, #42077, .T. ) ;
#48200 = DIRECTION ( 'NONE',  ( 1.000000000000000000, 0.000000000000000000, 0.000000000000000000 ) ) ;
#48201 = DIRECTION ( 'NONE',  ( 0.7585478161175716050, 0.6516173805718067369, 0.000000000000000000 ) ) ;
#48202 = CIRCLE ( 'NONE', #10687, 31.99999999999998934 ) ;
#48203 = DIRECTION ( 'NONE',  ( -1.000000000000000000, 0.000000000000000000, 0.000000000000000000 ) ) ;
#48204 = CARTESIAN_POINT ( 'NONE',  ( 0.000000000000000000, 27.75498641678742473, 31.52238457039609187 ) ) ;
#48205 = DIRECTION ( 'NONE',  ( 0.000000000000000000, 0.000000000000000000, 1.000000000000000000 ) ) ;
#48206 = DIRECTION ( 'NONE',  ( -1.000000000000000000, -0.000000000000000000, -0.000000000000000000 ) ) ;
#48207 = DIRECTION ( 'NONE',  ( 1.000000000000000000, 0.000000000000000000, 0.000000000000000000 ) ) ;
#48208 = EDGE_CURVE ( 'NONE', #25973, #9186, #41657, .T. ) ;
#48209 = CARTESIAN_POINT ( 'NONE',  ( 10.00000000000000000, 63.18004540533029001, 44.88180994100400767 ) ) ;
#48210 = CARTESIAN_POINT ( 'NONE',  ( 11.99999999999999822, 71.27951684758069462, -30.41916302227037150 ) ) ;
#48211 = ORIENTED_EDGE ( 'NONE', *, *, #27581, .F. ) ;
#48212 = DIRECTION ( 'NONE',  ( 0.000000000000000000, 0.000000000000000000, 1.000000000000000000 ) ) ;
#48213 = CARTESIAN_POINT ( 'NONE',  ( 0.000000000000000000, -46.54456581323847786, 59.03342792756247093 ) ) ;
#48214 = CONICAL_SURFACE ( 'NONE', #27124, 17.45460580326810174, 1.361356816555583826 ) ;
#48215 = SURFACE_STYLE_USAGE ( .BOTH. , #22016 ) ;
#48216 = FACE_OUTER_BOUND ( 'NONE', #28362, .T. ) ;
#48217 = VERTEX_POINT ( 'NONE', #31139 ) ;
#48218 = VERTEX_POINT ( 'NONE', #12056 ) ;
#48219 = ADVANCED_FACE ( 'NONE', ( #4694 ), #30176, .T. ) ;
#48220 = CARTESIAN_POINT ( 'NONE',  ( 0.000000000000000000, -120.0000000000000000, 2.500000000000000000 ) ) ;
#48221 = CARTESIAN_POINT ( 'NONE',  ( 10.00000000000000000, 0.000000000000000000, 0.000000000000000000 ) ) ;
#48222 = VERTEX_POINT ( 'NONE', #8123 ) ;
#48223 = CIRCLE ( 'NONE', #38070, 37.49900000000000233 ) ;
#48224 = ADVANCED_FACE ( 'NONE', ( #16208 ), #11802, .T. ) ;
#48225 = ORIENTED_EDGE ( 'NONE', *, *, #45976, .T. ) ;
#48226 = CIRCLE ( 'NONE', #31066, 16.00000000000000355 ) ;
#48227 =( REPRESENTATION_RELATIONSHIP ('NONE','NONE', #5957, #12525 ) REPRESENTATION_RELATIONSHIP_WITH_TRANSFORMATION ( #15970 )SHAPE_REPRESENTATION_RELATIONSHIP( ) );
#48228 = EDGE_CURVE ( 'NONE', #18781, #14446, #13183, .T. ) ;
#48229 = CARTESIAN_POINT ( 'NONE',  ( 10.00000000000000000, 33.17418723428307459, 17.67226234102837878 ) ) ;
#48230 = ORIENTED_EDGE ( 'NONE', *, *, #6041, .T. ) ;
#48231 = CARTESIAN_POINT ( 'NONE',  ( 10.00000000000000000, -37.16516213103273714, -4.992566952385376844 ) ) ;
#48232 = EDGE_LOOP ( 'NONE', ( #37301, #41201, #45808, #7564 ) ) ;
#48233 = ORIENTED_EDGE ( 'NONE', *, *, #34864, .F. ) ;
#48234 = ORIENTED_EDGE ( 'NONE', *, *, #33489, .F. ) ;
#48235 = DIRECTION ( 'NONE',  ( -1.000000000000000000, -0.000000000000000000, -0.000000000000000000 ) ) ;
#48236 = EDGE_CURVE ( 'NONE', #29872, #15938, #36603, .T. ) ;
#48237 = FACE_OUTER_BOUND ( 'NONE', #1051, .T. ) ;
#48238 = ORIENTED_EDGE ( 'NONE', *, *, #4482, .F. ) ;
#48239 = CIRCLE ( 'NONE', #44328, 82.00000000000000000 ) ;
#48240 = ORIENTED_EDGE ( 'NONE', *, *, #26800, .F. ) ;
#48241 = EDGE_CURVE ( 'NONE', #44547, #34735, #46063, .T. ) ;
#48242 = EDGE_LOOP ( 'NONE', ( #22292, #48105, #46791, #16768 ) ) ;
#48243 = DIRECTION ( 'NONE',  ( 0.000000000000000000, 0.000000000000000000, 1.000000000000000000 ) ) ;
#48244 = ORIENTED_EDGE ( 'NONE', *, *, #32459, .T. ) ;
#48245 = DIRECTION ( 'NONE',  ( 1.000000000000000000, 0.000000000000000000, 0.000000000000000000 ) ) ;
#48246 = PLANE ( 'NONE',  #19668 ) ;
#48247 = ORIENTED_EDGE ( 'NONE', *, *, #20472, .T. ) ;
#48248 = LINE ( 'NONE', #14725, #15117 ) ;
#48249 = DIRECTION ( 'NONE',  ( 0.000000000000000000, 0.5877852522924742473, -0.8090169943749466741 ) ) ;
#48250 = VERTEX_POINT ( 'NONE', #38232 ) ;
#48251 = VECTOR ( 'NONE', #47385, 1000.000000000000000 ) ;
#48252 = DIRECTION ( 'NONE',  ( -1.000000000000000000, 0.000000000000000000, 0.000000000000000000 ) ) ;
#48253 = DIRECTION ( 'NONE',  ( 1.000000000000000000, 0.000000000000000000, 0.000000000000000000 ) ) ;
#48254 = EDGE_LOOP ( 'NONE', ( #24215, #44738, #4843, #22582 ) ) ;
#48255 = CARTESIAN_POINT ( 'NONE',  ( 10.00000000000000000, 0.000000000000000000, 0.000000000000000000 ) ) ;
#48256 = ORIENTED_EDGE ( 'NONE', *, *, #16583, .T. ) ;
#48257 = EDGE_LOOP ( 'NONE', ( #19647, #2436, #724, #42600 ) ) ;
#48258 = CARTESIAN_POINT ( 'NONE',  ( 11.99999999999999822, 5.256550761633951296, -77.32052557432835727 ) ) ;
#48259 = FACE_OUTER_BOUND ( 'NONE', #43368, .T. ) ;
#48260 = ORIENTED_EDGE ( 'NONE', *, *, #33237, .F. ) ;
#48261 = DIRECTION ( 'NONE',  ( 0.000000000000000000, 0.000000000000000000, -1.000000000000000000 ) ) ;
#48262 = CYLINDRICAL_SURFACE ( 'NONE', #17995, 11.59999999999999787 ) ;
#48263 = CARTESIAN_POINT ( 'NONE',  ( 10.00000000000000000, -54.21277698773715059, 55.38113227695762930 ) ) ;
#48264 = DIRECTION ( 'NONE',  ( 0.000000000000000000, 0.000000000000000000, 1.000000000000000000 ) ) ;
#48265 = DIRECTION ( 'NONE',  ( 0.000000000000000000, 0.000000000000000000, 1.000000000000000000 ) ) ;
#48266 = FACE_OUTER_BOUND ( 'NONE', #29373, .T. ) ;
#48267 = VECTOR ( 'NONE', #2973, 1000.000000000000000 ) ;
#48268 = ORIENTED_EDGE ( 'NONE', *, *, #2759, .T. ) ;
#48269 = CARTESIAN_POINT ( 'NONE',  ( 11.99999999999999822, -41.76106447765443619, -62.50884508063471401 ) ) ;
#48270 = CARTESIAN_POINT ( 'NONE',  ( 10.00000000000000000, -41.19522573413687638, -65.64334221924953283 ) ) ;
#48271 = CARTESIAN_POINT ( 'NONE',  ( 0.000000000000000000, 0.000000000000000000, 0.000000000000000000 ) ) ;
#48272 = LINE ( 'NONE', #8114, #493 ) ;
#48273 = CARTESIAN_POINT ( 'NONE',  ( 10.00000000000000000, -80.55351364060578589, -15.33399622253569028 ) ) ;
#48274 = DIRECTION ( 'NONE',  ( 0.000000000000000000, 0.000000000000000000, 1.000000000000000000 ) ) ;
#48275 = DIRECTION ( 'NONE',  ( -1.000000000000000000, 0.000000000000000000, -0.000000000000000000 ) ) ;
#48276 = DIRECTION ( 'NONE',  ( -1.000000000000000000, -0.000000000000000000, 0.000000000000000000 ) ) ;
#48277 = ORIENTED_EDGE ( 'NONE', *, *, #10976, .T. ) ;
#48278 = EDGE_LOOP ( 'NONE', ( #38318, #19160, #3802, #22181, #12248 ) ) ;
#48279 = DIRECTION ( 'NONE',  ( -1.000000000000000000, 0.000000000000000000, 0.000000000000000000 ) ) ;
#48280 = VECTOR ( 'NONE', #9319, 1000.000000000000114 ) ;
#48281 = ORIENTED_EDGE ( 'NONE', *, *, #21305, .F. ) ;
#48282 = CYLINDRICAL_SURFACE ( 'NONE', #11191, 31.99999999999999289 ) ;
#48283 = SHAPE_DEFINITION_REPRESENTATION ( #28461, #21223 ) ;
#48284 = DIRECTION ( 'NONE',  ( -1.000000000000000000, 0.000000000000000000, -0.000000000000000000 ) ) ;
#48285 = VERTEX_POINT ( 'NONE', #27221 ) ;
#48286 = EDGE_CURVE ( 'NONE', #45432, #7133, #25658, .T. ) ;
#48287 = EDGE_CURVE ( 'NONE', #10988, #44380, #4933, .T. ) ;
#48288 = DIRECTION ( 'NONE',  ( 0.000000000000000000, -1.000000000000000000, -1.040834085586084730E-14 ) ) ;
#48289 = EDGE_LOOP ( 'NONE', ( #45915, #39229, #46962, #10759 ) ) ;
#48290 = EDGE_CURVE ( 'NONE', #17154, #18357, #34788, .T. ) ;
#48291 = AXIS2_PLACEMENT_3D ( 'NONE', #46770, #46276, #24234 ) ;
#48292 = CARTESIAN_POINT ( 'NONE',  ( 0.000000000000000000, -11.30684508768284680, -76.66974797899850103 ) ) ;
#48293 = ADVANCED_FACE ( 'NONE', ( #37743 ), #26732, .F. ) ;
#48294 = CARTESIAN_POINT ( 'NONE',  ( -21.33958957442910886, -129.9559990355020034, 5.500000000000000000 ) ) ;
#48296 = EDGE_LOOP ( 'NONE', ( #5678, #24010, #29226, #43817 ) ) ;
#48295 = LINE ( 'NONE', #40969, #41815 ) ;
#48297 = ORIENTED_EDGE ( 'NONE', *, *, #44353, .F. ) ;
#48298 = PRESENTATION_LAYER_ASSIGNMENT (  '', '', ( #34989 ) ) ;
#48299 = DIRECTION ( 'NONE',  ( -1.000000000000000000, 0.000000000000000000, 0.000000000000000000 ) ) ;
#48300 = EDGE_CURVE ( 'NONE', #43833, #24088, #12417, .T. ) ;
#48301 = CIRCLE ( 'NONE', #24863, 31.99999999999998579 ) ;
#48302 = EDGE_LOOP ( 'NONE', ( #31463, #26087, #11470, #10674 ) ) ;
#48303 = CARTESIAN_POINT ( 'NONE',  ( 0.000000000000000000, 73.73191006444572793, -14.66109333815486515 ) ) ;
#48304 = DIRECTION ( 'NONE',  ( -1.000000000000000000, -0.000000000000000000, 0.000000000000000000 ) ) ;
#48305 = CARTESIAN_POINT ( 'NONE',  ( -12.49999999999999822, -120.0000000000000000, 125.0000000000000000 ) ) ;
#48306 = CARTESIAN_POINT ( 'NONE',  ( 10.00000000000000000, 0.000000000000000000, 0.000000000000000000 ) ) ;
#48307 = ORIENTED_EDGE ( 'NONE', *, *, #20722, .T. ) ;
#48308 = DIRECTION ( 'NONE',  ( 0.000000000000000000, 0.000000000000000000, 1.000000000000000000 ) ) ;
#48309 = ORIENTED_EDGE ( 'NONE', *, *, #7949, .F. ) ;
#48310 = ORIENTED_EDGE ( 'NONE', *, *, #36423, .F. ) ;
#48311 = CARTESIAN_POINT ( 'NONE',  ( 0.000000000000000000, 59.03961581697465277, -46.53671651293886669 ) ) ;
#48312 = LINE ( 'NONE', #10147, #11347 ) ;
#48313 = LINE ( 'NONE', #14792, #6388 ) ;
#48314 = DIRECTION ( 'NONE',  ( -1.000000000000000000, 0.000000000000000000, 0.000000000000000000 ) ) ;
#48315 = EDGE_LOOP ( 'NONE', ( #19204, #16503, #33395, #34203 ) ) ;
#48317 = CYLINDRICAL_SURFACE ( 'NONE', #18232, 37.49900000000000233 ) ;
#48316 =( GEOMETRIC_REPRESENTATION_CONTEXT ( 3 ) GLOBAL_UNCERTAINTY_ASSIGNED_CONTEXT ( ( #41859 ) ) GLOBAL_UNIT_ASSIGNED_CONTEXT ( ( #22933, #15121, #31505 ) ) REPRESENTATION_CONTEXT ( 'NONE', 'WORKASPACE' ) );
#48318 = DIRECTION ( 'NONE',  ( 1.000000000000000000, 0.000000000000000000, 0.000000000000000000 ) ) ;
#48319 = FACE_OUTER_BOUND ( 'NONE', #10905, .T. ) ;
#48320 = AXIS2_PLACEMENT_3D ( 'NONE', #37113, #29534, #7010 ) ;
#48321 = FACE_OUTER_BOUND ( 'NONE', #16181, .T. ) ;
#48322 = FACE_OUTER_BOUND ( 'NONE', #12255, .T. ) ;
#48323 = CARTESIAN_POINT ( 'NONE',  ( -3.308722450212110699E-21, 16.95692799528845995, 2.500000000000000000 ) ) ;
#48324 = ORIENTED_EDGE ( 'NONE', *, *, #32682, .F. ) ;
#48325 = CARTESIAN_POINT ( 'NONE',  ( -2.977765906491215642, 0.000000000000000000, 0.000000000000000000 ) ) ;
#48326 = DIRECTION ( 'NONE',  ( -1.000000000000000000, -0.000000000000000000, 0.000000000000000000 ) ) ;
#48327 = CARTESIAN_POINT ( 'NONE',  ( -10.00000000000000000, 0.000000000000000000, 0.000000000000000000 ) ) ;
#48328 = DIRECTION ( 'NONE',  ( 0.000000000000000000, 0.3090169943749412895, 0.9510565162951556406 ) ) ;
#48329 = CARTESIAN_POINT ( 'NONE',  ( 19.12409105625795291, -101.5943176906707919, -5.500000000000000000 ) ) ;
#48330 = EDGE_CURVE ( 'NONE', #28663, #20905, #15247, .T. ) ;
#48331 = PLANE ( 'NONE',  #44337 ) ;
#48332 = CARTESIAN_POINT ( 'NONE',  ( 10.00000000000000000, 0.000000000000000000, 0.000000000000000000 ) ) ;
#48333 = FACE_OUTER_BOUND ( 'NONE', #39637, .T. ) ;
#48334 = LINE ( 'NONE', #40752, #47336 ) ;
#48335 = EDGE_CURVE ( 'NONE', #16500, #4758, #45999, .T. ) ;
#48336 = AXIS2_PLACEMENT_3D ( 'NONE', #20490, #34446, #38382 ) ;
#48337 = CIRCLE ( 'NONE', #44460, 37.49900000000000233 ) ;
#48338 = AXIS2_PLACEMENT_3D ( 'NONE', #32883, #43449, #28259 ) ;
#48339 = ADVANCED_FACE ( 'NONE', ( #45323 ), #34300, .T. ) ;
#48340 = CARTESIAN_POINT ( 'NONE',  ( 0.000000000000000000, -26.79245525562738095, 32.34446384429961796 ) ) ;
#48341 = ORIENTED_EDGE ( 'NONE', *, *, #30793, .T. ) ;
#48342 = ORIENTED_EDGE ( 'NONE', *, *, #37371, .T. ) ;
#48343 = LINE ( 'NONE', #14826, #14835 ) ;
#48344 = ADVANCED_FACE ( 'NONE', ( #13022 ), #5422, .T. ) ;
#48345 = ORIENTED_EDGE ( 'NONE', *, *, #36664, .F. ) ;
#48346 = ADVANCED_FACE ( 'NONE', ( #9808 ), #24498, .T. ) ;
#48347 = ADVANCED_FACE ( 'NONE', ( #35273 ), #46296, .F. ) ;
#48348 = CIRCLE ( 'NONE', #38192, 31.99999999999999289 ) ;
#48349 = CARTESIAN_POINT ( 'NONE',  ( 0.000000000000000000, -21.40280677340345505, -36.13751322684441192 ) ) ;
#48350 = VERTEX_POINT ( 'NONE', #1750 ) ;
#48351 = LINE ( 'NONE', #15326, #28862 ) ;
#48353 = ORIENTED_EDGE ( 'NONE', *, *, #38140, .T. ) ;
#48352 = CARTESIAN_POINT ( 'NONE',  ( 16.84844760790522855, -103.5491698323862124, 5.500000000000000000 ) ) ;
#48354 = VERTEX_POINT ( 'NONE', #42638 ) ;
#48355 = DIRECTION ( 'NONE',  ( 0.000000000000000000, 0.000000000000000000, 1.000000000000000000 ) ) ;
#48356 = ORIENTED_EDGE ( 'NONE', *, *, #1011, .F. ) ;
#48357 = ORIENTED_EDGE ( 'NONE', *, *, #14266, .T. ) ;
#48358 = VERTEX_POINT ( 'NONE', #16675 ) ;
#48359 = FACE_OUTER_BOUND ( 'NONE', #28145, .T. ) ;
#48360 = EDGE_CURVE ( 'NONE', #5353, #5571, #5914, .T. ) ;
#48361 = DIRECTION ( 'NONE',  ( 0.000000000000000000, -0.9969173337331287410, 0.07845909572783489605 ) ) ;
#48362 = DIRECTION ( 'NONE',  ( 0.000000000000000000, 0.8090169943749438985, -0.5877852522924780221 ) ) ;
#48363 = ORIENTED_EDGE ( 'NONE', *, *, #24605, .T. ) ;
#48364 = ORIENTED_EDGE ( 'NONE', *, *, #34252, .T. ) ;
#48365 = DIRECTION ( 'NONE',  ( 1.000000000000000000, 0.000000000000000000, 0.000000000000000000 ) ) ;
#48366 = EDGE_LOOP ( 'NONE', ( #34803, #15837, #41454, #27133 ) ) ;
#48367 = DIRECTION ( 'NONE',  ( -1.000000000000000000, 0.000000000000000000, 0.000000000000000000 ) ) ;
#48368 = VECTOR ( 'NONE', #42823, 1000.000000000000000 ) ;
#48369 = FACE_OUTER_BOUND ( 'NONE', #29105, .T. ) ;
#48371 = DIRECTION ( 'NONE',  ( -1.000000000000000000, -0.000000000000000000, -0.000000000000000000 ) ) ;
#48370 = AXIS2_PLACEMENT_3D ( 'NONE', #33928, #45680, #27092 ) ;
#48372 = DIRECTION ( 'NONE',  ( 0.000000000000000000, 0.000000000000000000, 1.000000000000000000 ) ) ;
#48373 = LINE ( 'NONE', #14853, #21180 ) ;
#48374 = CYLINDRICAL_SURFACE ( 'NONE', #2581, 32.00000000000000000 ) ;
#48375 = CIRCLE ( 'NONE', #46050, 82.00000000000000000 ) ;
#48376 = CARTESIAN_POINT ( 'NONE',  ( 10.00000000000000000, 40.98264845739763018, -9.188173127306866306 ) ) ;
#48377 = SURFACE_STYLE_FILL_AREA ( #403 ) ;
#48378 = CARTESIAN_POINT ( 'NONE',  ( 10.00000000000000000, -59.03961581697432592, 46.53671651293927880 ) ) ;
#48379 = ORIENTED_EDGE ( 'NONE', *, *, #39477, .F. ) ;
#48380 = CARTESIAN_POINT ( 'NONE',  ( 15.00000000000000000, -18.13022148937263012, -15.02647892043543898 ) ) ;
#48381 = ORIENTED_EDGE ( 'NONE', *, *, #29672, .T. ) ;
#48382 = DIRECTION ( 'NONE',  ( 0.000000000000000000, 0.5877852522924797984, -0.8090169943749426773 ) ) ;
#48383 = ORIENTED_EDGE ( 'NONE', *, *, #6757, .F. ) ;
#48384 = DIRECTION ( 'NONE',  ( 0.000000000000000000, 0.3090169943749480064, -0.9510565162951534202 ) ) ;
#48385 = DIRECTION ( 'NONE',  ( 0.000000000000000000, 0.000000000000000000, 1.000000000000000000 ) ) ;
#48386 = DIRECTION ( 'NONE',  ( -1.000000000000000000, 0.000000000000000000, -0.000000000000000000 ) ) ;
#48387 = DIRECTION ( 'NONE',  ( 0.000000000000000000, 0.000000000000000000, 1.000000000000000000 ) ) ;
#48388 = DIRECTION ( 'NONE',  ( 1.000000000000000000, 0.000000000000000000, 0.000000000000000000 ) ) ;
#48389 = EDGE_CURVE ( 'NONE', #30863, #38628, #46547, .T. ) ;
#48390 = DIRECTION ( 'NONE',  ( -1.000000000000000000, -0.000000000000000000, -0.000000000000000000 ) ) ;
#48391 = DIRECTION ( 'NONE',  ( 0.8774505977381983346, 0.4796670183876293736, 0.000000000000000000 ) ) ;
#48392 = ADVANCED_FACE ( 'NONE', ( #9098 ), #5663, .T. ) ;
#48393 = CARTESIAN_POINT ( 'NONE',  ( 0.000000000000000000, 0.000000000000000000, 0.000000000000000000 ) ) ;
#48394 = EDGE_CURVE ( 'NONE', #29150, #14780, #35079, .T. ) ;
#48395 = CARTESIAN_POINT ( 'NONE',  ( 5.000000000000000000, 77.16300072079660310, 27.74655509720696855 ) ) ;
#48396 = ORIENTED_EDGE ( 'NONE', *, *, #23157, .T. ) ;
#48397 = AXIS2_PLACEMENT_3D ( 'NONE', #1261, #45546, #4456 ) ;
#48398 = VECTOR ( 'NONE', #3867, 1000.000000000000000 ) ;
#48399 = ORIENTED_EDGE ( 'NONE', *, *, #25086, .F. ) ;
#48400 = CIRCLE ( 'NONE', #21803, 31.99999999999998579 ) ;
#48401 = ORIENTED_EDGE ( 'NONE', *, *, #41725, .T. ) ;
#48402 = DIRECTION ( 'NONE',  ( -1.000000000000000000, 0.000000000000000000, 0.000000000000000000 ) ) ;
#48403 = CYLINDRICAL_SURFACE ( 'NONE', #33870, 31.99999999999999289 ) ;
#48404 = EDGE_LOOP ( 'NONE', ( #13044, #46222, #29408, #21785 ) ) ;
#48405 = ADVANCED_FACE ( 'NONE', ( #32330 ), #16919, .F. ) ;
#48406 = ADVANCED_FACE ( 'NONE', ( #1511 ), #24970, .T. ) ;
#48407 = LINE ( 'NONE', #26145, #5399 ) ;
#48408 = ORIENTED_EDGE ( 'NONE', *, *, #19482, .T. ) ;
#48409 = EDGE_LOOP ( 'NONE', ( #27658, #6848, #24162, #468 ) ) ;
#48410 = CARTESIAN_POINT ( 'NONE',  ( 0.000000000000000000, 75.11764819372149304, -2.946379043146603482 ) ) ;
#48411 = ADVANCED_FACE ( 'NONE', ( #13248 ), #47260, .T. ) ;
#48412 = PLANE ( 'NONE',  #41490 ) ;
#48413 = EDGE_LOOP ( 'NONE', ( #12352, #39873, #43032, #2048 ) ) ;
#48414 = DIRECTION ( 'NONE',  ( -1.000000000000000000, -0.000000000000000000, -0.000000000000000000 ) ) ;
#48415 = ORIENTED_EDGE ( 'NONE', *, *, #33531, .F. ) ;
#48416 = VERTEX_POINT ( 'NONE', #43105 ) ;
#48417 = FACE_OUTER_BOUND ( 'NONE', #28356, .T. ) ;
#48418 = DIRECTION ( 'NONE',  ( 0.000000000000000000, 0.000000000000000000, 1.000000000000000000 ) ) ;
#48419 = DIRECTION ( 'NONE',  ( 0.000000000000000000, -0.1564344650402170744, -0.9876883405951398798 ) ) ;
#48420 = ORIENTED_EDGE ( 'NONE', *, *, #28883, .F. ) ;
#48421 = VERTEX_POINT ( 'NONE', #9555 ) ;
#48422 = FILL_AREA_STYLE ('',( #8032 ) ) ;
#48423 = CIRCLE ( 'NONE', #32799, 77.49899999999999523 ) ;
#48424 = DIRECTION ( 'NONE',  ( 0.000000000000000000, 1.000000000000000000, 3.491481338843133750E-15 ) ) ;
#48425 = ORIENTED_EDGE ( 'NONE', *, *, #21114, .T. ) ;
#48426 = AXIS2_PLACEMENT_3D ( 'NONE', #22168, #41031, #14832 ) ;
#48427 = ORIENTED_EDGE ( 'NONE', *, *, #45259, .F. ) ;
#48428 = CARTESIAN_POINT ( 'NONE',  ( 11.99999999999999822, 0.000000000000000000, 0.000000000000000000 ) ) ;
#48429 = CARTESIAN_POINT ( 'NONE',  ( 0.000000000000000000, 0.000000000000000000, 0.000000000000000000 ) ) ;
#48430 = VERTEX_POINT ( 'NONE', #35757 ) ;
#48431 = DIRECTION ( 'NONE',  ( 0.000000000000000000, 0.8090169943749486725, -0.5877852522924713607 ) ) ;
#48432 = DIRECTION ( 'NONE',  ( -0.5687579148473743684, 0.8225049752423791993, 0.000000000000000000 ) ) ;
#48433 = CARTESIAN_POINT ( 'NONE',  ( 11.99999999999999822, -41.76106447765533147, 62.50884508063410294 ) ) ;
#48434 = CARTESIAN_POINT ( 'NONE',  ( 11.99999999999999822, -55.19960302592029677, -51.03279382321147750 ) ) ;
#48435 = ORIENTED_EDGE ( 'NONE', *, *, #4137, .T. ) ;
#48436 = CARTESIAN_POINT ( 'NONE',  ( -3.000000000000000000, 16.83928648764923253, 16.46020748918050458 ) ) ;
#48437 = LINE ( 'NONE', #7580, #21869 ) ;
#48438 = VECTOR ( 'NONE', #5523, 1000.000000000000000 ) ;
#48439 = CARTESIAN_POINT ( 'NONE',  ( 0.000000000000000000, 71.87247863392471459, -39.47590169984770370 ) ) ;
#48440 = DIRECTION ( 'NONE',  ( 0.000000000000000000, -0.4067366430757908269, 0.9135454576426049744 ) ) ;
#48441 = CIRCLE ( 'NONE', #4709, 12.50000000000000000 ) ;
#48442 = DIRECTION ( 'NONE',  ( 0.000000000000000000, -0.5224985647159559043, 0.8526401643540878483 ) ) ;
#48443 = ORIENTED_EDGE ( 'NONE', *, *, #24470, .T. ) ;
#48444 = EDGE_CURVE ( 'NONE', #8436, #18013, #47574, .T. ) ;
#48445 = CARTESIAN_POINT ( 'NONE',  ( 10.00000000000000000, 36.88895765772642932, -6.736453364083163642 ) ) ;
#48446 = DIRECTION ( 'NONE',  ( 0.000000000000000000, 0.000000000000000000, 1.000000000000000000 ) ) ;
#48447 =( NAMED_UNIT ( * ) PLANE_ANGLE_UNIT ( ) SI_UNIT ( $, .RADIAN. ) );
#48448 = CYLINDRICAL_SURFACE ( 'NONE', #1378, 82.00000000000000000 ) ;
#48449 = EDGE_CURVE ( 'NONE', #44453, #24623, #43585, .T. ) ;
#48450 = ORIENTED_EDGE ( 'NONE', *, *, #40117, .T. ) ;
#48451 = EDGE_CURVE ( 'NONE', #35068, #31692, #45246, .T. ) ;
#48452 = CIRCLE ( 'NONE', #32852, 31.99999999999999645 ) ;
#48453 = NEXT_ASSEMBLY_USAGE_OCCURRENCE ( 'NAUO1', ' ', ' ', #16380, #16707, $ ) ;
#48454 = NEXT_ASSEMBLY_USAGE_OCCURRENCE ( 'NAUO2', ' ', ' ', #16380, #28304, $ ) ;
#48455 = NEXT_ASSEMBLY_USAGE_OCCURRENCE ( 'NAUO3', ' ', ' ', #16380, #10069, $ ) ;
#48456 = NEXT_ASSEMBLY_USAGE_OCCURRENCE ( 'NAUO4', ' ', ' ', #16380, #36966, $ ) ;
#48457 = NEXT_ASSEMBLY_USAGE_OCCURRENCE ( 'NAUO5', ' ', ' ', #16380, #1121, $ ) ;
#48458 = NEXT_ASSEMBLY_USAGE_OCCURRENCE ( 'NAUO6', ' ', ' ', #16380, #12192, $ ) ;
#48459 = NEXT_ASSEMBLY_USAGE_OCCURRENCE ( 'NAUO7', ' ', ' ', #16380, #22354, $ ) ;
#48460 = NEXT_ASSEMBLY_USAGE_OCCURRENCE ( 'NAUO8', ' ', ' ', #16380, #29525, $ ) ;
#48461 = NEXT_ASSEMBLY_USAGE_OCCURRENCE ( 'NAUO9', ' ', ' ', #16380, #46888, $ ) ;
#48462 = NEXT_ASSEMBLY_USAGE_OCCURRENCE ( 'NAUO10', ' ', ' ', #16380, #33713, $ ) ;
#48463 = NEXT_ASSEMBLY_USAGE_OCCURRENCE ( 'NAUO11', ' ', ' ', #16380, #33713, $ ) ;
#48464 = NEXT_ASSEMBLY_USAGE_OCCURRENCE ( 'NAUO12', ' ', ' ', #16380, #24442, $ ) ;
#48465 = NEXT_ASSEMBLY_USAGE_OCCURRENCE ( 'NAUO13', ' ', ' ', #16380, #24442, $ ) ;
#48466 = NEXT_ASSEMBLY_USAGE_OCCURRENCE ( 'NAUO14', ' ', ' ', #16380, #24442, $ ) ;
#48467 = NEXT_ASSEMBLY_USAGE_OCCURRENCE ( 'NAUO15', ' ', ' ', #16380, #24442, $ ) ;
#48468 = NEXT_ASSEMBLY_USAGE_OCCURRENCE ( 'NAUO16', ' ', ' ', #16380, #12192, $ ) ;
ENDSEC;
END-ISO-10303-21;
